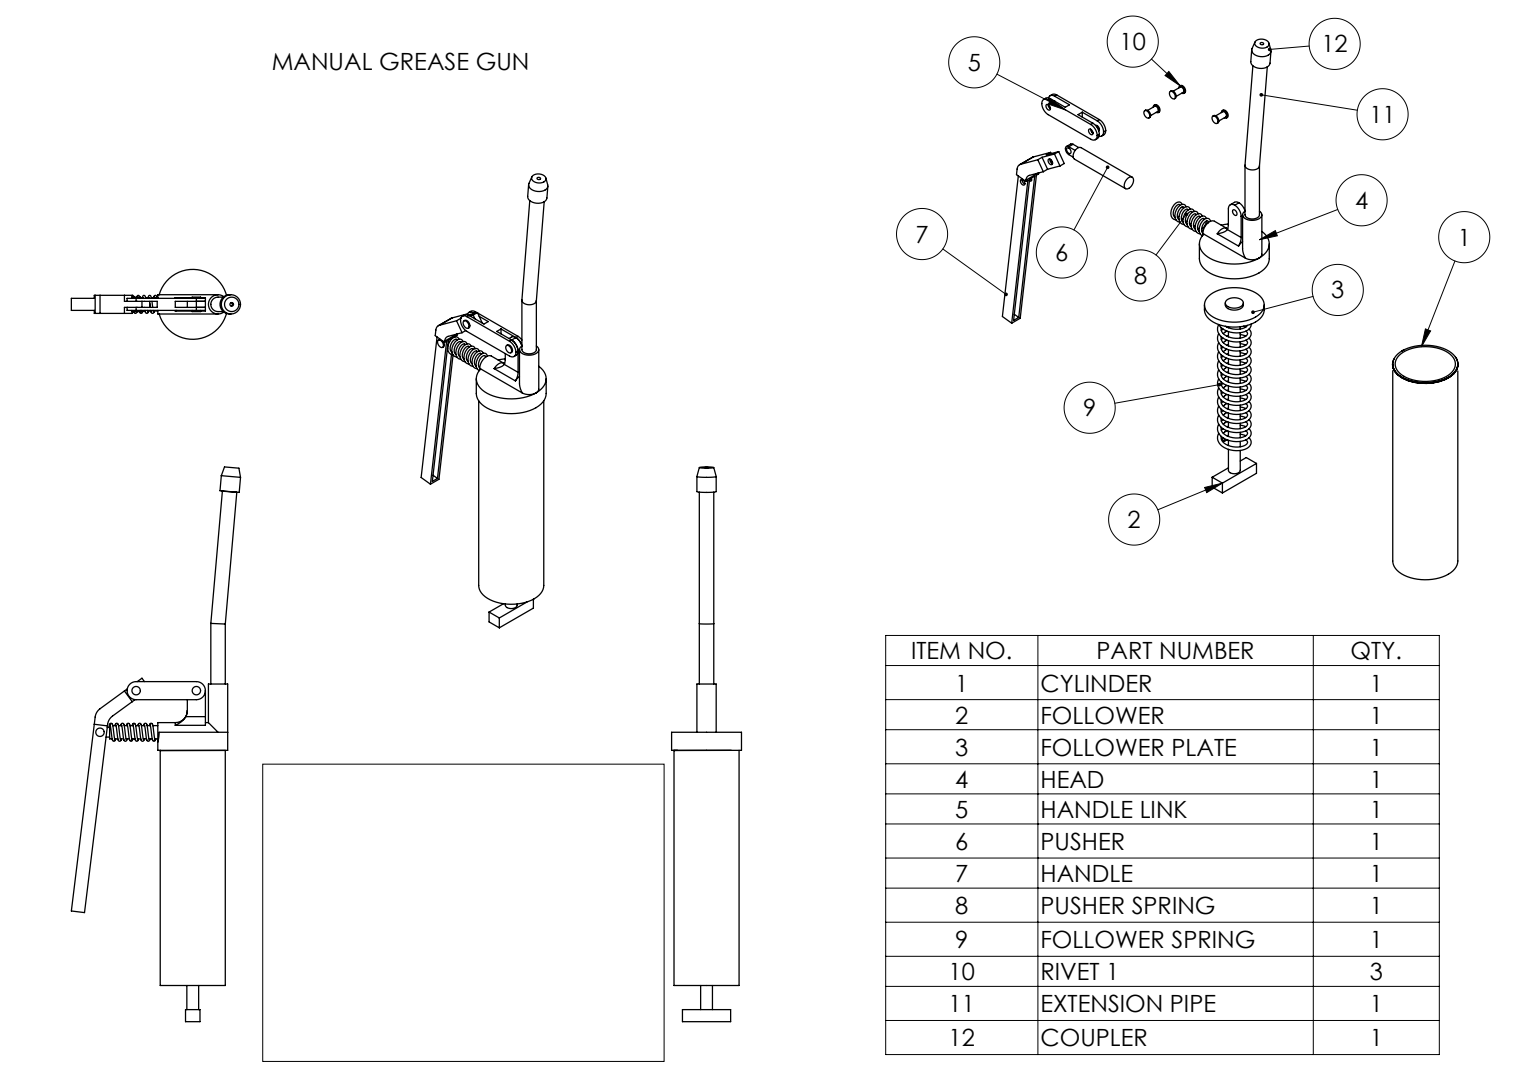
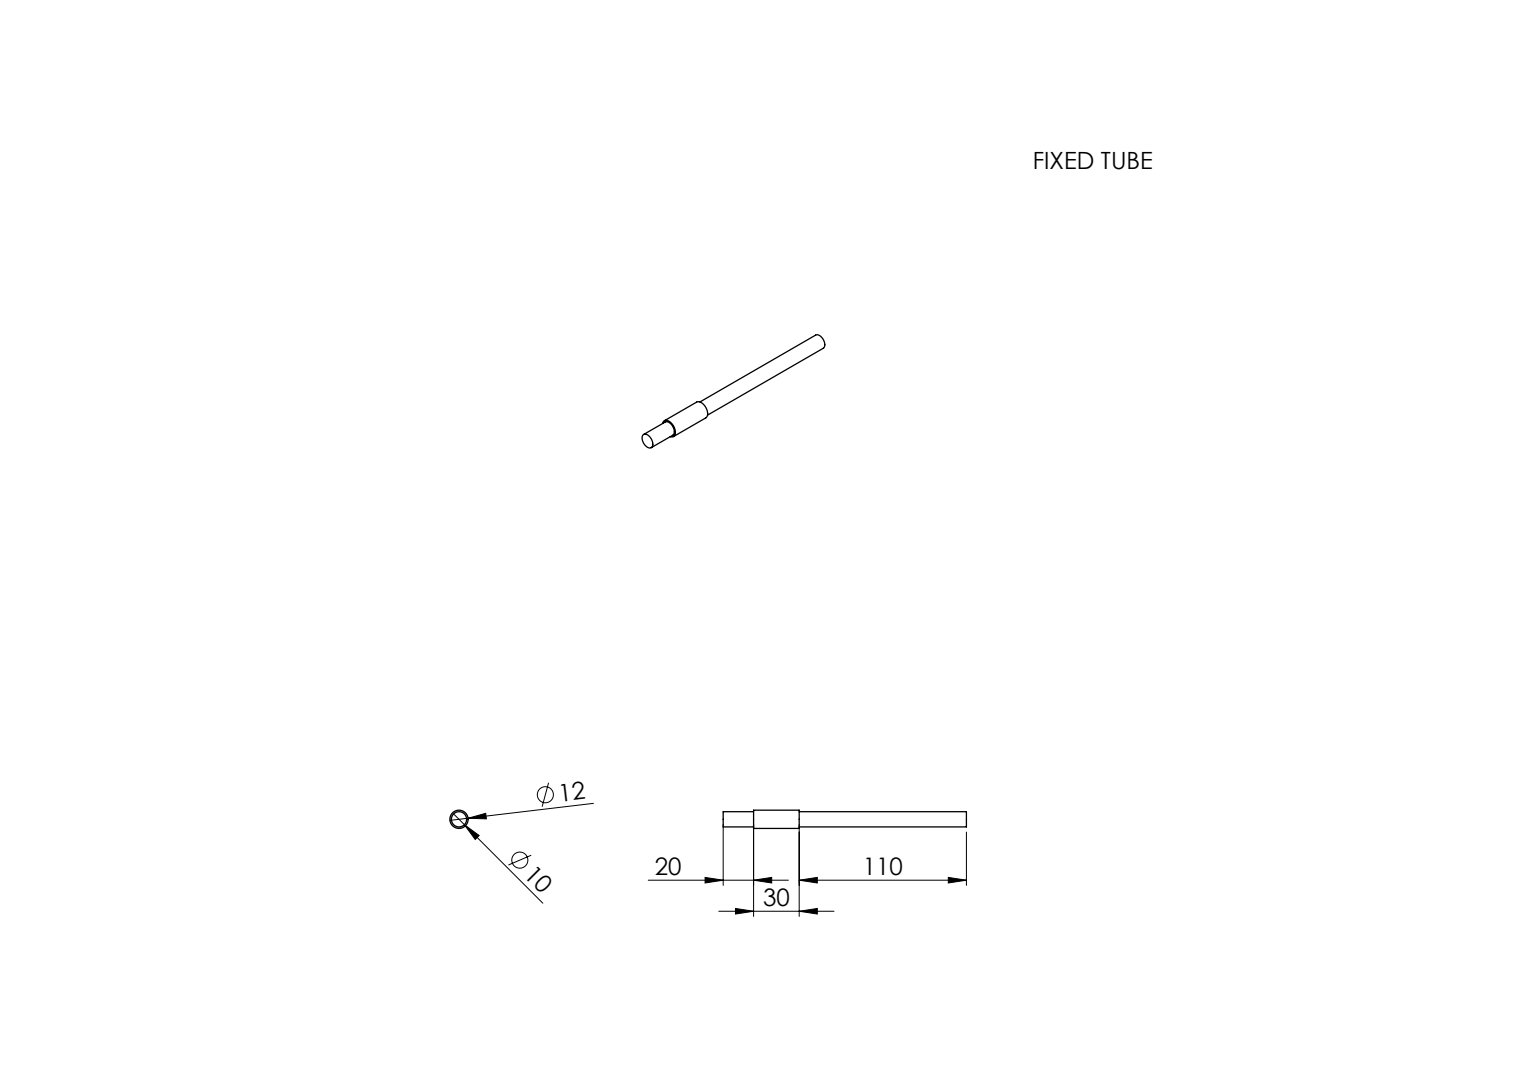
ISO-10303-21;
HEADER;
FILE_DESCRIPTION (('STEP AP214'),
    '1' );
FILE_NAME ('MAS-158',
    '2026-10-31T03:36:27',
    ( '' ),
    ( '' ),
    'SwSTEP 2.0',
    'SolidWorks 2026',
    '' );
FILE_SCHEMA (( 'AUTOMOTIVE_DESIGN' ));
ENDSEC;

DATA;
#1 = CARTESIAN_POINT ( 'NONE',  ( 20.99999999999999645, 6.928203230275506996, -4.556249998770971033 ) ) ;
#3 = ORIENTED_EDGE ( 'NONE', *, *, #2176, .T. ) ;
#2 = CIRCLE ( 'NONE', #23019, 1.000000000000002220 ) ;
#4 = CARTESIAN_POINT ( 'NONE',  ( 28.29077060037018043, 5.407089921784856479, 169.1523531505532674 ) ) ;
#5 = CARTESIAN_POINT ( 'NONE',  ( 6.840914352312096547, 71.36018628210143788, -6.594114490232313663 ) ) ;
#6 = CARTESIAN_POINT ( 'NONE',  ( -3.253724281355068545E-15, 198.6500000012290172, -27.00000000000000355 ) ) ;
#7 = CARTESIAN_POINT ( 'NONE',  ( 10.56230152254411081, 0.000000000000000000, -0.3374999987710014526 ) ) ;
#8 = DIRECTION ( 'NONE',  ( -1.000000000000000000, 0.000000000000000000, 0.000000000000000000 ) ) ;
#9 = CARTESIAN_POINT ( 'NONE',  ( -13.62178482187498396, 196.7843750006145456, 23.59362340125808188 ) ) ;
#10 = DIRECTION ( 'NONE',  ( 0.000000000000000000, 0.000000000000000000, 1.000000000000000000 ) ) ;
#11 = CARTESIAN_POINT ( 'NONE',  ( 31.25278368747686741, 6.928203230275514990, 167.1898537967678351 ) ) ;
#12 = CARTESIAN_POINT ( 'NONE',  ( 1.715153634034445762, 36.67731371789854933, -9.534712964251895073 ) ) ;
#13 = CARTESIAN_POINT ( 'NONE',  ( -1.926257025242585782E-15, 198.3968750006145285, -31.45816453501076637 ) ) ;
#14 = ORIENTED_EDGE ( 'NONE', *, *, #10865, .F. ) ;
#15 = ORIENTED_EDGE ( 'NONE', *, *, #13669, .F. ) ;
#16 = CARTESIAN_POINT ( 'NONE',  ( 18.00000000000000000, 239.6312500012290343, -5.196152422706630247 ) ) ;
#17 = CARTESIAN_POINT ( 'NONE',  ( 6.932735513424201024, 37.25231371789855217, -10.69584247140429412 ) ) ;
#18 = CARTESIAN_POINT ( 'NONE',  ( 19.68408634441911786, -5.407089921784861808, -9.046874999385529748 ) ) ;
#19 = CARTESIAN_POINT ( 'NONE',  ( 15.24356964375000167, -3.323476615752272600, -8.765624999385490668 ) ) ;
#20 = CARTESIAN_POINT ( 'NONE',  ( 13.23911966647199812, 140.7523137178985166, 8.632099005475788900 ) ) ;
#21 = VERTEX_POINT ( 'NONE', #9252 ) ;
#22 = CARTESIAN_POINT ( 'NONE',  ( 13.44051670066911619, -5.407089921784865361, -3.721874999385532679 ) ) ;
#23 = CARTESIAN_POINT ( 'NONE',  ( -13.62178482187500528, 199.2781250006145228, -23.59362340125807123 ) ) ;
#24 = CARTESIAN_POINT ( 'NONE',  ( 24.95044711734591658, -3.604726614523244610, 166.7907448923220954 ) ) ;
#25 = COLOUR_RGB ( '',0.8941176470588234615, 0.8941176470588234615, 0.8941176470588234615 ) ;
#26 = CARTESIAN_POINT ( 'NONE',  ( -33.37127896937850124, 216.5309553116391612, 1.626142955000506873 ) ) ;
#27 = CARTESIAN_POINT ( 'NONE',  ( 26.75643035624999655, 248.1718750006145342, -7.049594010296217766E-16 ) ) ;
#28 =( LENGTH_UNIT ( ) NAMED_UNIT ( * ) SI_UNIT ( .MILLI., .METRE. ) );
#29 = CARTESIAN_POINT ( 'NONE',  ( -17.60279642935561029, 194.9999999999999716, 20.73731651351060989 ) ) ;
#30 = CARTESIAN_POINT ( 'NONE',  ( -63.25669563604515844, 209.8844732041982297, -4.499999999999996447 ) ) ;
#31 = CARTESIAN_POINT ( 'NONE',  ( -50.99330436395489841, 210.1155267958017134, -6.500000000000000888 ) ) ;
#32 = CARTESIAN_POINT ( 'NONE',  ( 37.56819361912707222, 7.646167579472015790E-16, 167.7383919071516516 ) ) ;
#33 = EDGE_LOOP ( 'NONE', ( #36990, #5292, #11130, #31770 ) ) ;
#34 = CARTESIAN_POINT ( 'NONE',  ( 16.56230152254410726, 0.000000000000000000, -10.00000000000000000 ) ) ;
#35 = CARTESIAN_POINT ( 'NONE',  ( 23.99999999999999645, 5.196152422706631135, -0.5437499987709648597 ) ) ;
#36 = CARTESIAN_POINT ( 'NONE',  ( -13.23911966647199812, 25.75231371789854506, -8.632099005475788900 ) ) ;
#37 = CARTESIAN_POINT ( 'NONE',  ( -60.49330436395489130, 210.1155267958016850, -8.500000000000003553 ) ) ;
#38 = CARTESIAN_POINT ( 'NONE',  ( -9.500000000000005329, 141.5101862821014720, -0.1745138560725176813 ) ) ;
#39 = CARTESIAN_POINT ( 'NONE',  ( 2.311890736173175753, 56.12268628210144072, 12.53471296425194836 ) ) ;
#40 = CARTESIAN_POINT ( 'NONE',  ( 13.56230152254411792, -5.196152422706638241, -4.875000000000101252 ) ) ;
#41 = ORIENTED_EDGE ( 'NONE', *, *, #17124, .T. ) ;
#42 = CARTESIAN_POINT ( 'NONE',  ( -39.90997103062156270, 215.5714017266979852, 3.350049139982118618 ) ) ;
#43 = LINE ( 'NONE', #12559, #36906 ) ;
#44 = CARTESIAN_POINT ( 'NONE',  ( 13.62178482187501416, 195.9593750006145569, 23.59362340125806767 ) ) ;
#45 = CARTESIAN_POINT ( 'NONE',  ( 31.45868912971818432, 0.000000000000000000, 169.5433637710095809 ) ) ;
#46 = CARTESIAN_POINT ( 'NONE',  ( 37.19073179189800271, 7.347880794884117764E-16, 166.2186317273649934 ) ) ;
#47 = CARTESIAN_POINT ( 'NONE',  ( 22.60769515458672529, 246.3236538117967029, -6.000000000000004441 ) ) ;
#48 = CARTESIAN_POINT ( 'NONE',  ( 26.75643035624999655, 244.7218750006145456, -3.323476615752271712 ) ) ;
#49 = CARTESIAN_POINT ( 'NONE',  ( 8.843639120294245259, 94.46481371789855075, 3.474262827703527901 ) ) ;
#50 = LINE ( 'NONE', #15224, #14231 ) ;
#51 = VECTOR ( 'NONE', #30355, 1000.000000000000000 ) ;
#52 = ORIENTED_EDGE ( 'NONE', *, *, #4531, .T. ) ;
#53 = CARTESIAN_POINT ( 'NONE',  ( -55.74330436395489841, 210.1155267958017134, -6.500000000000000888 ) ) ;
#54 = CARTESIAN_POINT ( 'NONE',  ( 23.99999999999999645, 245.8562500012290570, -5.196152422706631135 ) ) ;
#55 = VERTEX_POINT ( 'NONE', #18167 ) ;
#56 = CARTESIAN_POINT ( 'NONE',  ( -10.49813415416004858, 106.8273137178985479, 7.228626920338840023 ) ) ;
#57 = CARTESIAN_POINT ( 'NONE',  ( 13.44051670066911441, -5.407089921784865361, -1.021874999385524729 ) ) ;
#58 = CARTESIAN_POINT ( 'NONE',  ( 24.36378002397578868, 0.000000000000000000, 160.0851093307920223 ) ) ;
#59 = CARTESIAN_POINT ( 'NONE',  ( 26.75643035624999655, 3.323476615752271712, -1.340624999385481075 ) ) ;
#60 = CARTESIAN_POINT ( 'NONE',  ( 0.1745138560722779009, 68.58981371789856496, 12.50000000000000355 ) ) ;
#61 = CARTESIAN_POINT ( 'NONE',  ( 27.00000000000001066, 196.1375000000000171, 15.58845726811988897 ) ) ;
#62 = EDGE_CURVE ( 'NONE', #31856, #6278, #12468, .T. ) ;
#63 = ORIENTED_EDGE ( 'NONE', *, *, #14775, .T. ) ;
#64 = ORIENTED_EDGE ( 'NONE', *, *, #31239, .F. ) ;
#65 = ORIENTED_EDGE ( 'NONE', *, *, #28486, .T. ) ;
#66 = CARTESIAN_POINT ( 'NONE',  ( 18.00000000000000355, -5.196152422706632912, -7.518749998770946519 ) ) ;
#67 = CARTESIAN_POINT ( 'NONE',  ( 23.87821517812499650, 4.985214923628404904, -6.140624999385474680 ) ) ;
#68 = CARTESIAN_POINT ( 'NONE',  ( 10.56230152254517307, 3.464101615138364565, -6.224999998771024501 ) ) ;
#69 = CARTESIAN_POINT ( 'NONE',  ( 23.87821517812499650, 246.8968750006145285, -4.985214923628404904 ) ) ;
#70 = CARTESIAN_POINT ( 'NONE',  ( 12.53471296425194836, 44.62268628210144783, -2.311890736173178418 ) ) ;
#71 =( BOUNDED_CURVE ( )  B_SPLINE_CURVE ( 2, ( #25117, #31002, #36483, #31184, #33841, #22103, #11088, #7506, #25303, #25677, #37040, #22287, #37228, #16414, #5388, #22845, #19080, #4648, #7879, #11276, #5022, #24930, #13939, #16602, #28145, #33652, #16967, #25488, #30632, #10526, #31363, #36855, #10899, #7691, #16229, #4836, #13565, #22472, #28510, #14121, #27961, #34021, #8065, #19272, #19642, #36675, #30813, #10713, #22664, #5207, #2366, #16783, #28328, #1992, #34208, #8252, #19826, #3481, #14864, #31546, #34574, #20184, #28698, #32288, #14673, #14488, #2918, #17156, #23026, #25859, #2734, #8803, #31734, #28883, #12011, #11824, #37407, #31918, #8433, #630, #20376, #11637, #14307, #26045, #5947, #34761, #259, #29446, #34943, #8614, #26223, #17711, #6330, #5761, #23395, #72, #23211, #17527, #29061, #17341, #11458, #3105, #8987, #5571, #20744, #20558, #32102, #6133, #29251, #3292, #26411, #445, #23583, #35126, #9176, #17901, #15050, #26599, #12197, #34392, #20002, #7093, #10110, #21503, #12580, #29821, #21681, #33046, #32473, #15615, #24517, #12767, #24336, #33233, #18662, #30202, #27169, #26790, #4043, #21125, #18472, #15240, #20939, #21313, #35877, #26980, #35310, #4415, #12391, #4228, #1192, #9919, #1386, #15997, #12957, #1007, #27545, #6897, #30013, #18847, #24147, #35689, #36067, #15805, #32850, #27355, #9742, #7272, #30392, #1571, #23771, #9365, #6518, #18093, #29634, #3670, #821, #23961, #35504, #9551, #32664, #6705, #18277, #3855, #15431, #16364, #22423, #24885, #34157, #21865, #2129, #13326, #5344 ),
 .UNSPECIFIED., .F., .F. ) 
 B_SPLINE_CURVE_WITH_KNOTS ( ( 3, 2, 2, 2, 2, 2, 2, 2, 2, 2, 2, 2, 2, 2, 2, 2, 2, 2, 2, 2, 2, 2, 2, 2, 2, 2, 2, 2, 2, 2, 2, 2, 2, 2, 2, 2, 2, 2, 2, 2, 2, 2, 2, 2, 2, 2, 2, 2, 2, 2, 2, 2, 2, 2, 2, 2, 2, 2, 2, 2, 2, 2, 2, 2, 2, 2, 2, 2, 2, 2, 2, 2, 2, 2, 2, 2, 2, 2, 2, 2, 2, 2, 2, 2, 2, 2, 2, 2, 2, 2, 2, 2, 2, 2, 2, 2, 3 ),
 ( 0.000000000000000000, 0.01041666666666666609, 0.02083333333333333218, 0.03125000000000000000, 0.04166666666666666435, 0.05208333333333333565, 0.06250000000000000000, 0.07291666666666667129, 0.08333333333333332871, 0.09375000000000000000, 0.1041666666666666713, 0.1145833333333333287, 0.1250000000000000000, 0.1354166666666666574, 0.1458333333333333426, 0.1562500000000000000, 0.1666666666666666574, 0.1770833333333333426, 0.1875000000000000000, 0.1979166666666666574, 0.2083333333333333426, 0.2187500000000000000, 0.2291666666666666574, 0.2395833333333333426, 0.2500000000000000000, 0.2604166666666666852, 0.2708333333333333148, 0.2812500000000000000, 0.2916666666666666852, 0.3020833333333333148, 0.3125000000000000000, 0.3229166666666666852, 0.3333333333333333148, 0.3437500000000000000, 0.3541666666666666852, 0.3645833333333333148, 0.3750000000000000000, 0.3854166666666666852, 0.3958333333333333148, 0.4062500000000000000, 0.4166666666666666852, 0.4270833333333333148, 0.4375000000000000000, 0.4479166666666666852, 0.4583333333333333148, 0.4687500000000000000, 0.4791666666666666852, 0.4895833333333333148, 0.5000000000000000000, 0.5104166666666666297, 0.5208333333333333703, 0.5312500000000000000, 0.5416666666666666297, 0.5520833333333333703, 0.5625000000000000000, 0.5729166666666666297, 0.5833333333333333703, 0.5937500000000000000, 0.6041666666666666297, 0.6145833333333333703, 0.6250000000000000000, 0.6354166666666666297, 0.6458333333333333703, 0.6562500000000000000, 0.6666666666666666297, 0.6770833333333333703, 0.6875000000000000000, 0.6979166666666666297, 0.7083333333333333703, 0.7187500000000000000, 0.7291666666666666297, 0.7395833333333333703, 0.7500000000000000000, 0.7604166666666666297, 0.7708333333333333703, 0.7812500000000000000, 0.7916666666666666297, 0.8020833333333333703, 0.8125000000000000000, 0.8229166666666666297, 0.8333333333333333703, 0.8437500000000000000, 0.8541666666666666297, 0.8645833333333333703, 0.8750000000000000000, 0.8854166666666666297, 0.8958333333333333703, 0.9062500000000000000, 0.9166666666666666297, 0.9270833333333333703, 0.9375000000000000000, 0.9479166666666666297, 0.9583333333333333703, 0.9687500000000000000, 0.9791666666666666297, 0.9895833333333333703, 1.000000000000000000 ),
 .UNSPECIFIED. ) 
 CURVE ( )  GEOMETRIC_REPRESENTATION_ITEM ( )  RATIONAL_B_SPLINE_CURVE ( ( 1.000000000000000000, 0.9659258262890683122, 1.000000000000000000, 0.9659258262890683122, 1.000000000000000000, 0.9659258262890683122, 1.000000000000000000, 0.9659258262890683122, 1.000000000000000000, 0.9659258262890683122, 1.000000000000000000, 0.9659258262890683122, 1.000000000000000000, 0.9659258262890683122, 1.000000000000000000, 0.9659258262890683122, 1.000000000000000000, 0.9659258262890683122, 1.000000000000000000, 0.9659258262890683122, 1.000000000000000000, 0.9659258262890683122, 1.000000000000000000, 0.9659258262890683122, 1.000000000000000000, 0.9659258262890683122, 1.000000000000000000, 0.9659258262890683122, 1.000000000000000000, 0.9659258262890683122, 1.000000000000000000, 0.9659258262890683122, 1.000000000000000000, 0.9659258262890683122, 1.000000000000000000, 0.9659258262890683122, 1.000000000000000000, 0.9659258262890683122, 1.000000000000000000, 0.9659258262890683122, 1.000000000000000000, 0.9659258262890683122, 1.000000000000000000, 0.9659258262890683122, 1.000000000000000000, 0.9659258262890683122, 1.000000000000000000, 0.9659258262890683122, 1.000000000000000000, 0.9659258262890683122, 1.000000000000000000, 0.9659258262890683122, 1.000000000000000000, 0.9659258262890683122, 1.000000000000000000, 0.9659258262890683122, 1.000000000000000000, 0.9659258262890683122, 1.000000000000000000, 0.9659258262890683122, 1.000000000000000000, 0.9659258262890683122, 1.000000000000000000, 0.9659258262890683122, 1.000000000000000000, 0.9659258262890683122, 1.000000000000000000, 0.9659258262890683122, 1.000000000000000000, 0.9659258262890683122, 1.000000000000000000, 0.9659258262890683122, 1.000000000000000000, 0.9659258262890683122, 1.000000000000000000, 0.9659258262890683122, 1.000000000000000000, 0.9659258262890683122, 1.000000000000000000, 0.9659258262890683122, 1.000000000000000000, 0.9659258262890683122, 1.000000000000000000, 0.9659258262890683122, 1.000000000000000000, 0.9659258262890683122, 1.000000000000000000, 0.9659258262890683122, 1.000000000000000000, 0.9659258262890683122, 1.000000000000000000, 0.9659258262890683122, 1.000000000000000000, 0.9659258262890683122, 1.000000000000000000, 0.9659258262890683122, 1.000000000000000000, 0.9659258262890683122, 1.000000000000000000, 0.9659258262890683122, 1.000000000000000000, 0.9659258262890683122, 1.000000000000000000, 0.9659258262890683122, 1.000000000000000000, 0.9659258262890683122, 1.000000000000000000, 0.9659258262890683122, 1.000000000000000000, 0.9659258262890683122, 1.000000000000000000, 0.9659258262890683122, 1.000000000000000000, 0.9659258262890683122, 1.000000000000000000, 0.9659258262890683122, 1.000000000000000000, 0.9659258262890683122, 1.000000000000000000, 0.9659258262890683122, 1.000000000000000000, 0.9659258262890683122, 1.000000000000000000, 0.9659258262890683122, 1.000000000000000000, 0.9659258262890683122, 1.000000000000000000, 0.9659258262890683122, 1.000000000000000000, 0.9659258262890683122, 1.000000000000000000, 0.9659258262890683122, 1.000000000000000000, 0.9659258262890683122, 1.000000000000000000, 0.9659258262890683122, 1.000000000000000000, 0.9659258262890683122, 1.000000000000000000, 0.9659258262890683122, 1.000000000000000000, 0.9659258262890683122, 1.000000000000000000, 0.9659258262890683122, 1.000000000000000000, 0.9659258262890683122, 1.000000000000000000, 0.9659258262890683122, 1.000000000000000000, 0.9659258262890683122, 1.000000000000000000, 0.9659258262890683122, 1.000000000000000000, 0.9659258262890683122, 1.000000000000000000, 0.9659258262890683122, 1.000000000000000000, 0.9659258262890683122, 1.000000000000000000, 0.9659258262890683122, 1.000000000000000000, 0.9659258262890683122, 1.000000000000000000, 0.9659258262890683122, 1.000000000000000000, 0.9659258262890683122, 1.000000000000000000, 0.9659258262890683122, 1.000000000000000000, 0.9659258262890683122, 1.000000000000000000, 0.9659258262890683122, 1.000000000000000000, 0.9659258262890683122, 1.000000000000000000, 0.9659258262890683122, 1.000000000000000000, 0.9659258262890683122, 1.000000000000000000, 0.9659258262890683122, 1.000000000000000000, 0.9659258262890683122, 1.000000000000000000, 0.9659258262890683122, 1.000000000000000000, 0.9659258262890683122, 1.000000000000000000, 0.9659258262890683122, 1.000000000000000000, 0.9659258262890683122, 1.000000000000000000, 0.9659258262890683122, 1.000000000000000000 ) ) 
 REPRESENTATION_ITEM ( '' )  );
#72 = CARTESIAN_POINT ( 'NONE',  ( -49.20461230271183695, 208.1428034533958851, -6.469044688360754414 ) ) ;
#73 = CARTESIAN_POINT ( 'NONE',  ( 19.06670604969950489, 215.1554505341192964, -5.693556627486040966 ) ) ;
#74 = CARTESIAN_POINT ( 'NONE',  ( -39.30877896937850124, 211.0902445701383101, -4.530955311639234040 ) ) ;
#75 = CARTESIAN_POINT ( 'NONE',  ( 33.73804336749152810, 5.196152422706631135, 161.1753621882693892 ) ) ;
#76 = CARTESIAN_POINT ( 'NONE',  ( 0.1745138560722779009, 96.18981371789855928, 12.50000000000000355 ) ) ;
#77 = CARTESIAN_POINT ( 'NONE',  ( -61.28497103062156981, 206.1606490808709111, -2.350049139982163027 ) ) ;
#78 = CARTESIAN_POINT ( 'NONE',  ( -39.90997103062156270, 217.3034525342668815, 4.350049139982096413 ) ) ;
#79 = EDGE_CURVE ( 'NONE', #19909, #6556, #23186, .T. ) ;
#80 = CARTESIAN_POINT ( 'NONE',  ( 23.87821517812499650, 4.985214923628404904, -5.353124999385477700 ) ) ;
#81 = CARTESIAN_POINT ( 'NONE',  ( 10.56230152254410726, 0.000000000000000000, -4.387499998770999277 ) ) ;
#82 = CARTESIAN_POINT ( 'NONE',  ( -3.257655550456946880, 82.10231371789853938, -15.46528703574811736 ) ) ;
#83 = CARTESIAN_POINT ( 'NONE',  ( -60.88169563604516554, 210.1155267958018271, 8.500000000000003553 ) ) ;
#84 = ORIENTED_EDGE ( 'NONE', *, *, #36303, .T. ) ;
#85 = DIRECTION ( 'NONE',  ( -0.000000000000000000, -0.000000000000000000, 1.000000000000000000 ) ) ;
#86 = CARTESIAN_POINT ( 'NONE',  ( -8.715434833791929847, 105.8601862821014521, -8.962234695871762469 ) ) ;
#87 = CARTESIAN_POINT ( 'NONE',  ( 13.04141134922759804, 54.97268628210144215, 8.927990412390657937 ) ) ;
#88 = EDGE_CURVE ( 'NONE', #32501, #27950, #21194, .T. ) ;
#89 = DIRECTION ( 'NONE',  ( -1.000000000000000000, -6.123233995736766036E-17, 0.000000000000000000 ) ) ;
#90 =( BOUNDED_CURVE ( )  B_SPLINE_CURVE ( 2, ( #11851, #8830, #29090, #22871, #2761, #17369, #11485, #23054, #34600 ),
 .UNSPECIFIED., .F., .F. ) 
 B_SPLINE_CURVE_WITH_KNOTS ( ( 3, 2, 2, 2, 3 ),
 ( 0.3125000000000000000, 0.3194444444444444198, 0.3333333333333333148, 0.3472222222222222099, 0.3541666666666666852 ),
 .UNSPECIFIED. ) 
 CURVE ( )  GEOMETRIC_REPRESENTATION_ITEM ( )  RATIONAL_B_SPLINE_CURVE ( ( 0.9330127018922194093, 0.9330127018922194093, 1.000000000000000000, 0.8660254037844387076, 1.000000000000000000, 0.8660254037844387076, 1.000000000000000000, 0.9330127018922190762, 0.9330127018922194093 ) ) 
 REPRESENTATION_ITEM ( '' )  );
#91 = CARTESIAN_POINT ( 'NONE',  ( 36.93903810116746911, 3.604726614523243278, 160.5471114303018680 ) ) ;
#92 = CARTESIAN_POINT ( 'NONE',  ( -0.1745138560725817967, 74.81018628210145494, 15.50000000000000533 ) ) ;
#93 = CARTESIAN_POINT ( 'NONE',  ( 27.24356964375000700, 199.0906250006145228, 15.72908226750537075 ) ) ;
#94 = CARTESIAN_POINT ( 'NONE',  ( 10.31873187879411269, 0.000000000000000000, -10.04062499938554431 ) ) ;
#95 = DIRECTION ( 'NONE',  ( 0.000000000000000000, 0.000000000000000000, 1.000000000000000000 ) ) ;
#96 = CARTESIAN_POINT ( 'NONE',  ( -46.63913769728824121, 206.8500491399821044, -5.686928522499717253 ) ) ;
#97 = CARTESIAN_POINT ( 'NONE',  ( 11.28998163430637725, -3.344369132205555317, -9.999999999999998224 ) ) ;
#98 = CARTESIAN_POINT ( 'NONE',  ( 11.48171059495397728, 45.48518628210145209, 4.944772684328674117 ) ) ;
#99 = CARTESIAN_POINT ( 'NONE',  ( 5.727106289114498080E-15, 196.0625000000000000, 31.17691453623979214 ) ) ;
#100 = DIRECTION ( 'NONE',  ( -1.000000000000000000, 0.000000000000000000, 5.782411586589356653E-16 ) ) ;
#101 = CARTESIAN_POINT ( 'NONE',  ( 9.534712964251900402, 140.1773137178985564, 1.715153634034445540 ) ) ;
#102 = CARTESIAN_POINT ( 'NONE',  ( 26.75643035624999655, 247.8718750006145228, -3.323476615752271268 ) ) ;
#103 = ORIENTED_EDGE ( 'NONE', *, *, #10401, .F. ) ;
#104 = CARTESIAN_POINT ( 'NONE',  ( 15.00000000000000000, 3.464101615137752166, -5.437500000000009770 ) ) ;
#105 = AXIS2_PLACEMENT_3D ( 'NONE', #31796, #37295, #28576 ) ;
#106 = DIRECTION ( 'NONE',  ( 0.9961946980917462113, 0.000000000000000000, -0.08715574274765118534 ) ) ;
#107 = LINE ( 'NONE', #3514, #14620 ) ;
#108 = CARTESIAN_POINT ( 'NONE',  ( 22.80587116629411781, -3.604726614523235284, -3.553124999385526728 ) ) ;
#109 = CARTESIAN_POINT ( 'NONE',  ( 31.18169728485186454, -7.209453229046475009, 166.3773324967488918 ) ) ;
#110 = CARTESIAN_POINT ( 'NONE',  ( 26.99999999999999645, 240.2874999999999659, 3.464101615137751278 ) ) ;
#111 = DIRECTION ( 'NONE',  ( 1.000000000000000000, 0.000000000000000000, 0.000000000000000000 ) ) ;
#112 = CARTESIAN_POINT ( 'NONE',  ( -12.53471296425194659, 67.62268628210145494, 2.311890736173176641 ) ) ;
#113 = VERTEX_POINT ( 'NONE', #15124 ) ;
#114 = ORIENTED_EDGE ( 'NONE', *, *, #15759, .T. ) ;
#115 = CARTESIAN_POINT ( 'NONE',  ( -98.52697526167152375, 63.53212182842481326, 3.000000000000000000 ) ) ;
#116 = VECTOR ( 'NONE', #35899, 1000.000000000000000 ) ;
#117 = CARTESIAN_POINT ( 'NONE',  ( 26.99999999999999645, 194.9750000012290343, -15.58845726811990495 ) ) ;
#118 = DIRECTION ( 'NONE',  ( -0.000000000000000000, 0.000000000000000000, 1.000000000000000000 ) ) ;
#119 = CARTESIAN_POINT ( 'NONE',  ( 21.00000000000000000, 6.646953231504538984, -7.003124999385472726 ) ) ;
#120 = ADVANCED_FACE ( 'NONE', ( #26675 ), #705, .F. ) ;
#121 = CARTESIAN_POINT ( 'NONE',  ( 8.632099005475788900, 46.45231371789854791, -13.23911966647199812 ) ) ;
#122 = CARTESIAN_POINT ( 'NONE',  ( 31.03707322417642800, -6.928203230275514990, 164.7242719189907803 ) ) ;
#123 = CARTESIAN_POINT ( 'NONE',  ( 34.15965927292618431, 5.196152422706637353, 165.9944540390638679 ) ) ;
#124 = CARTESIAN_POINT ( 'NONE',  ( -40.10788769728823411, 214.4690446883608104, 1.321298161741840893 ) ) ;
#125 = CARTESIAN_POINT ( 'NONE',  ( 16.56230152254410726, 0.000000000000000000, -10.00000000000000000 ) ) ;
#126 = CARTESIAN_POINT ( 'NONE',  ( 31.34102887711597774, 6.928203230275506996, 168.1985009298100522 ) ) ;
#127 = CARTESIAN_POINT ( 'NONE',  ( -3.474262827703527901, 23.16481371789855359, 8.843639120294245259 ) ) ;
#128 = EDGE_CURVE ( 'NONE', #11418, #35635, #36670, .T. ) ;
#129 = CARTESIAN_POINT ( 'NONE',  ( -55.74330436395489841, 210.1155267958017134, -6.500000000000000888 ) ) ;
#130 = DIRECTION ( 'NONE',  ( 1.000000000000000000, 0.000000000000000000, 0.000000000000000000 ) ) ;
#131 = DIRECTION ( 'NONE',  ( 0.9961946980917462113, 0.000000000000000000, -0.08715574274765118534 ) ) ;
#132 = CARTESIAN_POINT ( 'NONE',  ( -1.926257025242585782E-15, 195.6968750006145683, -31.45816453501075927 ) ) ;
#133 = CARTESIAN_POINT ( 'NONE',  ( -3.257655550456946880, 137.3023137178985564, -15.46528703574811736 ) ) ;
#134 =( BOUNDED_CURVE ( )  B_SPLINE_CURVE ( 2, ( #28363, #34243, #8285, #7031, #33171, #27292, #31580 ),
 .UNSPECIFIED., .F., .F. ) 
 B_SPLINE_CURVE_WITH_KNOTS ( ( 3, 2, 2, 3 ),
 ( 0.2826086956521732252, 0.2898550724637675158, 0.2971014492753617509, 0.3043478260869560414 ),
 .UNSPECIFIED. ) 
 CURVE ( )  GEOMETRIC_REPRESENTATION_ITEM ( )  RATIONAL_B_SPLINE_CURVE ( ( 1.000000000000012212, 0.8660254037844263841, 1.000000000000000000, 0.8660254037844387076, 1.000000000000000000, 0.8660254037844479225, 0.9999999999999907851 ) ) 
 REPRESENTATION_ITEM ( '' )  );
#135 = ADVANCED_FACE ( 'NONE', ( #36144 ), #26701, .T. ) ;
#136 = EDGE_LOOP ( 'NONE', ( #21590, #33549, #31769, #19071 ) ) ;
#137 = CARTESIAN_POINT ( 'NONE',  ( -4.622313124798576922, 42.03518628210144215, -11.61527771782819762 ) ) ;
#138 = PLANE ( 'NONE',  #16547 ) ;
#139 = CARTESIAN_POINT ( 'NONE',  ( 26.40304527788004663, 2.021082040740327379, -8.000000000000000000 ) ) ;
#140 = CARTESIAN_POINT ( 'NONE',  ( 37.59924285248093412, -3.604726614523238837, 168.0932862683468443 ) ) ;
#141 = CARTESIAN_POINT ( 'NONE',  ( 15.00000000000000178, -3.464101615137757051, -1.256249998770949228 ) ) ;
#142 = CARTESIAN_POINT ( 'NONE',  ( 13.44051670066910908, 5.407089921784862696, -9.721874999385510918 ) ) ;
#143 = CARTESIAN_POINT ( 'NONE',  ( 8.710071997420127943, 82.28518628210146346, 3.796722387233375073 ) ) ;
#144 = CYLINDRICAL_SURFACE ( 'NONE', #32201, 27.00000000000000000 ) ;
#145 = CARTESIAN_POINT ( 'NONE',  ( 22.60769515458672885, 244.9174038105676630, -5.999999999999998224 ) ) ;
#146 = ADVANCED_FACE ( 'NONE', ( #11518 ), #17218, .F. ) ;
#147 = CARTESIAN_POINT ( 'NONE',  ( -12.53471296425194836, 86.02268628210146062, 2.311890736173176641 ) ) ;
#148 = CARTESIAN_POINT ( 'NONE',  ( -13.50000000000000533, 195.0875000012290457, -23.38268590217984411 ) ) ;
#149 = VERTEX_POINT ( 'NONE', #2983 ) ;
#150 = CARTESIAN_POINT ( 'NONE',  ( 36.93740393099094632, -3.604726614523235284, 160.5284327797126025 ) ) ;
#151 = CARTESIAN_POINT ( 'NONE',  ( 15.24356964374999990, 3.323476615752268604, -7.378124999385474503 ) ) ;
#152 = LINE ( 'NONE', #25749, #18668 ) ;
#153 = CARTESIAN_POINT ( 'NONE',  ( 24.98313052087628350, 3.604726614523240613, 167.1643179041065252 ) ) ;
#154 = CARTESIAN_POINT ( 'NONE',  ( 34.06814574304114984, -5.196152422706635576, 164.9484496060674985 ) ) ;
#155 = LINE ( 'NONE', #26123, #10199 ) ;
#156 = CARTESIAN_POINT ( 'NONE',  ( 18.00000000000000355, 248.7249999999999943, 5.196152422706632912 ) ) ;
#157 = CARTESIAN_POINT ( 'NONE',  ( 27.24356964374999279, 197.8156250006145171, -15.72908226750539207 ) ) ;
#158 = CARTESIAN_POINT ( 'NONE',  ( 0.1745138560722779009, 123.7898137178985678, 12.50000000000000355 ) ) ;
#159 = CARTESIAN_POINT ( 'NONE',  ( -4.944772684328673229, 121.3851862821014578, 11.48171059495397728 ) ) ;
#160 = UNCERTAINTY_MEASURE_WITH_UNIT (LENGTH_MEASURE( 1.000000000000000082E-05 ), #19760, 'distance_accuracy_value', 'NONE');
#162 = ORIENTED_EDGE ( 'NONE', *, *, #30521, .T. ) ;
#161 = EDGE_LOOP ( 'NONE', ( #20979, #30282, #30052, #34984, #7724, #7445, #15889, #35352 ) ) ;
#163 = CARTESIAN_POINT ( 'NONE',  ( -13.62178482187498396, 198.5281250006145228, 23.59362340125808188 ) ) ;
#164 = CARTESIAN_POINT ( 'NONE',  ( 23.87821517812500005, 243.1468750006145285, 4.985214923628404016 ) ) ;
#165 = ADVANCED_FACE ( 'NONE', ( #28756 ), #138, .T. ) ;
#166 = CARTESIAN_POINT ( 'NONE',  ( -13.23911966647199812, 90.15231371789855075, -8.632099005475788900 ) ) ;
#167 = AXIS2_PLACEMENT_3D ( 'NONE', #4303, #33308, #24772 ) ;
#168 = CARTESIAN_POINT ( 'NONE',  ( 26.75643035624999655, 3.323476615752271712, -3.140624999385464022 ) ) ;
#169 = CARTESIAN_POINT ( 'NONE',  ( 23.87821517812499650, 246.5593750006145228, -4.985214923628404904 ) ) ;
#170 = CARTESIAN_POINT ( 'NONE',  ( 5.727106289114498080E-15, 197.0750000012290570, 31.17691453623979214 ) ) ;
#171 = CARTESIAN_POINT ( 'NONE',  ( 9.465287035748106703, 84.40231371789855075, -2.064181346179063237 ) ) ;
#172 = CARTESIAN_POINT ( 'NONE',  ( 19.68408634441911076, 5.407089921784857367, -4.790624999385539873 ) ) ;
#173 = CARTESIAN_POINT ( 'NONE',  ( 26.75643035624999655, 241.9093750006145171, -3.323476615752271268 ) ) ;
#174 = CARTESIAN_POINT ( 'NONE',  ( 10.49813415416005213, 47.02731371789855075, -7.228626920338837358 ) ) ;
#175 = EDGE_CURVE ( 'NONE', #2711, #16688, #11211, .T. ) ;
#176 = CARTESIAN_POINT ( 'NONE',  ( 26.99999999999999645, 246.6812500012290457, -7.347880794884117764E-16 ) ) ;
#177 = AXIS2_PLACEMENT_3D ( 'NONE', #6579, #20812, #23648 ) ;
#178 = CARTESIAN_POINT ( 'NONE',  ( 10.49813415415989581, 110.1726862821014521, 7.228626920339068285 ) ) ;
#179 = CARTESIAN_POINT ( 'NONE',  ( 10.56230152254411259, 3.464101615137752166, -4.874999998771025744 ) ) ;
#180 = CARTESIAN_POINT ( 'NONE',  ( -31.99330436395490196, 210.1155267958017134, -6.500000000000000888 ) ) ;
#181 = CARTESIAN_POINT ( 'NONE',  ( -7.228626920339069173, 140.0726862821014720, 10.49813415415989581 ) ) ;
#182 = CARTESIAN_POINT ( 'NONE',  ( 21.00000000000016342, 4.000000000000002665, 50.00000000000000000 ) ) ;
#183 = CARTESIAN_POINT ( 'NONE',  ( -15.46528703574804986, 104.9976862821014549, -3.257655550457287497 ) ) ;
#184 = CARTESIAN_POINT ( 'NONE',  ( 10.49813415415989581, 18.17268628210144499, 7.228626920339069173 ) ) ;
#185 = CARTESIAN_POINT ( 'NONE',  ( 0.000000000000000000, 2.000000000000000000, 0.000000000000000000 ) ) ;
#186 = CARTESIAN_POINT ( 'NONE',  ( 0.000000000000000000, 148.0000000000000000, 0.000000000000000000 ) ) ;
#187 = CARTESIAN_POINT ( 'NONE',  ( 6.840914352312096547, 126.5601862821014834, -6.594114490232313663 ) ) ;
#188 = CARTESIAN_POINT ( 'NONE',  ( 30.87038786627866216, 6.928203230275506996, 162.8190495601146495 ) ) ;
#189 = CARTESIAN_POINT ( 'NONE',  ( 21.00000000000000000, 241.9843750006145058, -6.646953231504538984 ) ) ;
#190 = VERTEX_POINT ( 'NONE', #2796 ) ;
#191 = FACE_OUTER_BOUND ( 'NONE', #37346, .T. ) ;
#192 = CARTESIAN_POINT ( 'NONE',  ( -8.710071997420127943, 68.48518628210145209, -3.796722387233380402 ) ) ;
#193 = CARTESIAN_POINT ( 'NONE',  ( 15.24356964375000167, -3.323476615752272600, -1.453124999385472016 ) ) ;
#195 = EDGE_CURVE ( 'NONE', #23387, #15078, #25492, .T. ) ;
#194 = CARTESIAN_POINT ( 'NONE',  ( 5.999999999999999112, -30.00000000000000000, -19.99999999999999289 ) ) ;
#196 = DIRECTION ( 'NONE',  ( -0.000000000000000000, -0.000000000000000000, 1.000000000000000000 ) ) ;
#197 = CARTESIAN_POINT ( 'NONE',  ( 5.778771075727756162E-15, 195.0218750006145569, 31.45816453501075927 ) ) ;
#198 = EDGE_CURVE ( 'NONE', #717, #36155, #34079, .T. ) ;
#199 = CARTESIAN_POINT ( 'NONE',  ( 0.000000000000000000, 0.000000000000000000, 0.000000000000000000 ) ) ;
#200 = CARTESIAN_POINT ( 'NONE',  ( -7.234628195640263826, 196.8700961906613713, -27.00000000000003553 ) ) ;
#201 = SHAPE_REPRESENTATION ( 'coupler', ( #17215 ), #24466 ) ;
#202 = CARTESIAN_POINT ( 'NONE',  ( -6.594114490232462877, 42.13981371789854791, 6.840914352311949109 ) ) ;
#203 = DIRECTION ( 'NONE',  ( 0.000000000000000000, 0.000000000000000000, -1.000000000000000000 ) ) ;
#204 = ORIENTED_EDGE ( 'NONE', *, *, #34329, .T. ) ;
#205 = VERTEX_POINT ( 'NONE', #8495 ) ;
#206 = CARTESIAN_POINT ( 'NONE',  ( 26.75643035624999655, 249.4843750006145058, 3.323476615752267715 ) ) ;
#207 = CARTESIAN_POINT ( 'NONE',  ( -8.962234695871565293, 35.23981371789855643, -8.715434833792128799 ) ) ;
#208 = CARTESIAN_POINT ( 'NONE',  ( 16.56230152254411436, 7.209453229046482114, -8.859374999385529748 ) ) ;
#209 = CARTESIAN_POINT ( 'NONE',  ( 19.00081571707366379, 5.492723647597353320, -10.23957781181608517 ) ) ;
#210 = CARTESIAN_POINT ( 'NONE',  ( 8.715434833792128799, 19.13981371789855146, -8.962234695871567070 ) ) ;
#211 = EDGE_CURVE ( 'NONE', #2909, #23659, #28387, .T. ) ;
#212 = VERTEX_POINT ( 'NONE', #19884 ) ;
#213 = CARTESIAN_POINT ( 'NONE',  ( 19.68408634441912142, -5.407089921784861808, -3.646874999385540939 ) ) ;
#214 = CARTESIAN_POINT ( 'NONE',  ( 27.24356964374999635, 199.1656250006145399, -15.72908226750539029 ) ) ;
#215 = CARTESIAN_POINT ( 'NONE',  ( 25.06483902970220967, 0.000000000000000000, 168.0982504335675287 ) ) ;
#216 = CARTESIAN_POINT ( 'NONE',  ( -66.02752896937849414, 214.3500491399821897, 7.303452534266821949 ) ) ;
#217 = CARTESIAN_POINT ( 'NONE',  ( 15.24356964375000167, 248.4343750006145513, 3.323476615752272600 ) ) ;
#218 = FILL_AREA_STYLE ('',( #11593 ) ) ;
#219 = CARTESIAN_POINT ( 'NONE',  ( -17.17757150371551944, 194.9999999999999716, 21.09399746705422984 ) ) ;
#220 = CARTESIAN_POINT ( 'NONE',  ( -53.55877896937850124, 211.0902445701383101, -4.530955311639234040 ) ) ;
#221 = CARTESIAN_POINT ( 'NONE',  ( -38.52455436395488420, 205.1570982666397356, 4.673758765035198159 ) ) ;
#222 = EDGE_LOOP ( 'NONE', ( #9327, #12339, #21719, #21080 ) ) ;
#223 = CARTESIAN_POINT ( 'NONE',  ( -28.99999999999999645, 201.9999999999999716, -1.007612034238798379E-23 ) ) ;
#224 = CARTESIAN_POINT ( 'NONE',  ( 20.99999999999997868, 210.0000000000000000, -5.999999999999999112 ) ) ;
#225 = CARTESIAN_POINT ( 'NONE',  ( -13.23911966647199812, 16.55231371789855643, -8.632099005475788900 ) ) ;
#226 = AXIS2_PLACEMENT_3D ( 'NONE', #11748, #5679, #26519 ) ;
#227 = CARTESIAN_POINT ( 'NONE',  ( -57.72247103062156270, 205.6499508600178956, 7.303452534266880569 ) ) ;
#228 = CARTESIAN_POINT ( 'NONE',  ( 7.228626920339068285, 6.672686282101436106, -10.49813415415989581 ) ) ;
#229 = CARTESIAN_POINT ( 'NONE',  ( 11.61527771782819940, 44.33518628210145351, -4.622313124798573369 ) ) ;
#230 = AXIS2_PLACEMENT_3D ( 'NONE', #7909, #4677, #5414 ) ;
#231 = CARTESIAN_POINT ( 'NONE',  ( 10.56230152254410726, 0.000000000000000000, -3.600000000000047606 ) ) ;
#232 = ORIENTED_EDGE ( 'NONE', *, *, #9936, .F. ) ;
#233 = CARTESIAN_POINT ( 'NONE',  ( -36.74330436395489841, 210.1155267958017134, -6.500000000000000888 ) ) ;
#234 = CARTESIAN_POINT ( 'NONE',  ( 21.00000000000000000, 242.4625000000000057, 5.999999999999998224 ) ) ;
#235 = CARTESIAN_POINT ( 'NONE',  ( 13.62178482187501416, 195.0593750006145513, 23.59362340125806767 ) ) ;
#236 = LINE ( 'NONE', #19612, #23826 ) ;
#237 = CARTESIAN_POINT ( 'NONE',  ( 26.99999999999999645, 196.3250000012290570, -15.58845726811990495 ) ) ;
#238 = DIRECTION ( 'NONE',  ( -0.000000000000000000, -0.000000000000000000, 1.000000000000000000 ) ) ;
#239 = CARTESIAN_POINT ( 'NONE',  ( 22.60769515458672885, 246.1388461906613827, 5.999999999999997335 ) ) ;
#240 = CARTESIAN_POINT ( 'NONE',  ( 21.00000000000000000, 244.5718750006145115, 6.646953231504538984 ) ) ;
#241 = CARTESIAN_POINT ( 'NONE',  ( -9.465287035748106703, 89.00231371789853085, 2.064181346179061460 ) ) ;
#242 = CARTESIAN_POINT ( 'NONE',  ( 24.81477950914817754, 0.000000000000000000, 162.4454087870936121 ) ) ;
#243 = ORIENTED_EDGE ( 'NONE', *, *, #7163, .F. ) ;
#244 = CARTESIAN_POINT ( 'NONE',  ( -53.56622103062157692, 211.6261429550005744, 6.530955311639227823 ) ) ;
#245 = CARTESIAN_POINT ( 'NONE',  ( 15.00000000000000000, 246.4562500012290513, 0.000000000000000000 ) ) ;
#246 = CARTESIAN_POINT ( 'NONE',  ( -6.932735513424201912, 106.2523137178985593, 10.69584247140429412 ) ) ;
#247 = CARTESIAN_POINT ( 'NONE',  ( 19.68408634441911076, 5.407089921784862696, -2.146874999385511629 ) ) ;
#248 = CARTESIAN_POINT ( 'NONE',  ( 20.99999999999997868, 246.9625000000000057, 5.999999999999999112 ) ) ;
#249 = CARTESIAN_POINT ( 'NONE',  ( 26.75643035624999655, 3.323476615752271712, -2.240624999385472549 ) ) ;
#250 = CARTESIAN_POINT ( 'NONE',  ( -6.932735513424201912, 69.45231371789856212, 10.69584247140429412 ) ) ;
#251 = CARTESIAN_POINT ( 'NONE',  ( 27.24356964375000345, 198.2843750006145456, -3.336375036156643733E-15 ) ) ;
#252 = ORIENTED_EDGE ( 'NONE', *, *, #5826, .F. ) ;
#253 = VERTEX_POINT ( 'NONE', #25549 ) ;
#254 = ORIENTED_EDGE ( 'NONE', *, *, #1063, .F. ) ;
#255 = CARTESIAN_POINT ( 'NONE',  ( 15.24356964374999990, 3.323476615752268604, -4.678124999385468108 ) ) ;
#256 = CARTESIAN_POINT ( 'NONE',  ( -27.00000000000000355, 195.5000000000000000, 0.000000000000000000 ) ) ;
#257 = CARTESIAN_POINT ( 'NONE',  ( 15.24356964374999990, 246.1468750006145285, 0.000000000000000000 ) ) ;
#258 = CARTESIAN_POINT ( 'NONE',  ( 11.48171059495397728, 36.28518628210144925, 4.944772684328674117 ) ) ;
#259 = CARTESIAN_POINT ( 'NONE',  ( -50.98586230271183695, 206.8500491399821328, 5.686928522499748340 ) ) ;
#260 = EDGE_CURVE ( 'NONE', #23273, #19908, #35667, .T. ) ;
#261 = CARTESIAN_POINT ( 'NONE',  ( 17.34006124879648425, 219.7598366698888981, -4.770645753573318437 ) ) ;
#262 = CARTESIAN_POINT ( 'NONE',  ( -31.39211230271183339, 205.5309553116392465, 1.321298161741817356 ) ) ;
#263 = SHAPE_REPRESENTATION_RELATIONSHIP ( 'NONE' , 'NONE' ,  #10836, #22840 ) ;
#264 = CARTESIAN_POINT ( 'NONE',  ( 27.81970530529572372, -5.196152422706632912, 162.3707280659671994 ) ) ;
#265 = CARTESIAN_POINT ( 'NONE',  ( 11.48171059495408208, 111.7148137178985650, -4.944772684328420986 ) ) ;
#266 = CARTESIAN_POINT ( 'NONE',  ( -65.44122103062156270, 208.9097554298617752, -4.530955311639240257 ) ) ;
#267 = CARTESIAN_POINT ( 'NONE',  ( -66.03497103062157692, 204.4285982733020148, -3.350049139982115509 ) ) ;
#268 = CARTESIAN_POINT ( 'NONE',  ( 26.75643035624999655, 7.049594010296217766E-16, -4.978124999385491023 ) ) ;
#269 = CARTESIAN_POINT ( 'NONE',  ( 24.00000000000000000, -5.196152422706629359, -1.650000000000012568 ) ) ;
#270 = CARTESIAN_POINT ( 'NONE',  ( 13.23911966647199812, 76.35231371789853938, 8.632099005475788900 ) ) ;
#271 = CARTESIAN_POINT ( 'NONE',  ( -52.96502896937850124, 217.3034525342667962, -4.350049139982195001 ) ) ;
#272 = ORIENTED_EDGE ( 'NONE', *, *, #322, .F. ) ;
#273 = FACE_OUTER_BOUND ( 'NONE', #13038, .T. ) ;
#274 = CARTESIAN_POINT ( 'NONE',  ( -0.1745138560725500443, 111.6101862821014521, 12.50000000000000355 ) ) ;
#275 = CARTESIAN_POINT ( 'NONE',  ( 3.257655550457285720, 52.09768628210144925, -15.46528703574804986 ) ) ;
#276 = CARTESIAN_POINT ( 'NONE',  ( 33.95006120609467359, 5.407089921784862696, 162.2014130487530110 ) ) ;
#277 = CARTESIAN_POINT ( 'NONE',  ( -13.23911966647218463, 67.04768628210143788, 8.632099005475506459 ) ) ;
#278 = CARTESIAN_POINT ( 'NONE',  ( -44.35000000000001563, 244.5000000000000000, -5.000000000000001776 ) ) ;
#279 = CARTESIAN_POINT ( 'NONE',  ( 22.80587116629410716, 7.646167579472015790E-16, -9.365624999385563143 ) ) ;
#280 = CARTESIAN_POINT ( 'NONE',  ( 24.71019261795870037, -3.464101615138094559, 161.2499751506078383 ) ) ;
#281 = CARTESIAN_POINT ( 'NONE',  ( -50.59747103062156270, 213.3500491399821328, -5.571401726697985168 ) ) ;
#282 = LINE ( 'NONE', #23417, #32949 ) ;
#283 = CARTESIAN_POINT ( 'NONE',  ( -7.228626920339069173, 48.07268628210143646, 10.49813415415989581 ) ) ;
#284 = CARTESIAN_POINT ( 'NONE',  ( -26.99999999999998934, 195.9875000000000114, 15.58845726811991561 ) ) ;
#285 = DIRECTION ( 'NONE',  ( 1.000000000000000000, 0.000000000000000000, 0.000000000000000000 ) ) ;
#286 = CARTESIAN_POINT ( 'NONE',  ( -6.840914352312096547, 11.56018628210145316, 6.594114490232313663 ) ) ;
#287 = CARTESIAN_POINT ( 'NONE',  ( 20.99999999999999645, 245.9218750006145626, 6.646953231504538984 ) ) ;
#288 = ORIENTED_EDGE ( 'NONE', *, *, #7515, .F. ) ;
#289 = CARTESIAN_POINT ( 'NONE',  ( 15.00000000000000000, 3.464101615137752166, -3.637499999999994849 ) ) ;
#290 = CARTESIAN_POINT ( 'NONE',  ( 34.18580599575048495, -5.196152422706635576, 166.2933124484913492 ) ) ;
#291 = CARTESIAN_POINT ( 'NONE',  ( 20.99999999999999645, 185.0294372515228645, -5.999999999999999112 ) ) ;
#292 = CARTESIAN_POINT ( 'NONE',  ( 10.31873187879411269, 3.604726614523236616, -4.228124999385536320 ) ) ;
#293 = CARTESIAN_POINT ( 'NONE',  ( 34.37331128181295270, -5.407089921784855591, 167.0391835513610488 ) ) ;
#294 =( BOUNDED_SURFACE ( )  B_SPLINE_SURFACE ( 3, 2, ( 
 ( #18814, #1535, #16329, #12732, #30357, #24662, #4381, #10074, #36214, #10256, #21466, #27877, #18433, #18626, #1349, #16146, #21832, #33386, #35842, #32814, #30167, #12921, #7426, #1908, #13478, #15771, #18995, #30552, #27696, #1724, #1160, #24484, #25030, #24849, #4194, #13293, #36399, #22020, #33573, #7609, #36589, #29974, #15579, #27133, #24299, #22575, #25406, #7981, #16516, #20099, #36957, #28063, #16704, #8533, #14222, #33939, #22389, #22760, #19554, #14040, #5486, #31648, #10818, #37144, #28252, #11003, #34121, #8171, #31103, #2098, #5675, #2466, #2281, #11186, #34309, #22946, #28609, #4934, #19746, #5124, #13858, #31283, #30915, #5311, #7796, #19926, #16889, #8353, #28425, #13676, #25589, #31464, #25224, #19373, #22207, #17069, #2646, #25772, #36773, #37324, #34492, #11374, #17256, #28795, #2833, #14405, #25961, #26889, #33756, #178, #26898, #12112, #21043, #17822, #35417, #8900, #545, #14592, #363, #20854, #5864, #23685, #18007, #29736, #12305, #26515, #35231, #26327, #9281, #34673, #20477, #29359, #11927, #32393, #23496, #6433, #3398, #35045, #9093, #6245, #20662, #26144, #29551, #3590, #14967, #15152, #26703, #23879, #734, #32208, #9468, #32580, #28981, #6621, #18197, #3770, #15344, #11556, #23130, #11744, #8718, #20290, #23313, #6047, #31830, #17442, #3022, #34860, #32016, #17633, #29165, #3209, #14783, #7565, #21417, #21604, #4335, #35987, #1117, #1490, #12683, #30311, #21789, #10402, #27092, #15914, #7011, #4153, #1302, #15724, #24254, #32772, #36355, #18770, #18580, #27463, #13064, #1679, #7380, #21233, #12871, #35798, #32960, #9840, #9655, #30122, #24065, #36169, #27274, #24621, #24438, #6807, #10023, #33153, #18383, #35611, #928, #7198, #10215, #33341, #29933, #18951, #13254, #30505, #4525, #21977, #16101, #27653, #24803, #3961, #33522, #19140, #16287, #30689, #4707, #12498, #15535, #25180, #16848, #30870, #16661, #37099, #22164, #2423, #34268, #8494, #28569, #5269, #28386, #5083, #13996, #13435, #36732, #8130, #28207, #25548, #2237, #11148, #34078, #13816, #25363, #22532, #36910, #4893, #22723, #8312, #19701, #19883, #31426, #2607, #31240, #10958, #5447, #25735, #7748, #17029, #14181, #37287, #11335, #22905, #34452, #16474, #20062, #1864, #28019, #22345, #31606, #5633, #27834, #2052, #24984, #10772, #33895, #36542, #10585, #33708, #7937, #19331, #13630, #19513, #31059, #23087, #11700, #3548, #9237, #28944, #6009, #32164, #23454, #17593, #3166, #11886, #31980, #20248, #3356, #23647, #35008, #506, #6202, #29507, #9051, #29124, #20622, #15111, #34631, #14739, #17774, #26287, #320, #29317, #14925, #31788, #26662, #28755, #17404, #23274, #26473, #12072, #35190, #5824, #32538, #14551, #34818, #20811, #692, #23834, #137, #32353, #6392, #17965, #12263, #8676, #8861, #35375, #9426, #2982, #26104, #21003, #20437, #17217, #2795, #14367, #25922, #37467, #11517, #9797, #6968, #21375, #29887, #883, #4982, #24394, #24207, #21563, #7656, #7842, #13524, #26854, #18536, #3918, #1073, #18339, #15301, #6765, #29695, #4799, #32914, #30776, #12643, #12455, #15491, #4110, #24024, #3729, #6578, #30075, #9982, #16377, #35569, #35942, #19415, #33108, #19233, #16565, #1953, #27923, #25080, #9614, #36635, #32728, #22437, #10674, #28110, #12826, #30964, #27047, #22253, #21188, #15682, #33805, #35752, #2141, #13721, #25270, #36821, #10863, #18154, #27233, #1257, #19601, #5356, #14273, #22807, #8580, #25452, #34541, #31511, #25824, #31150, #20149, #23178, #17306, #33983, #17492, #11791, #29027, #28659, #2333, #2697, #28295, #37192, #34171, #37005, #37372, #13904, #11424, #5534, #22991, #11235, #8027, #14641, #22624, #14453, #31696, #5724, #11603, #26190, #34723, #34356, #228, #17121, #28846, #3071, #8401, #11049, #5913, #8216, #2881, #5169, #26009, #19969 ),
 ( #38, #16747, #8767, #20341, #19791, #31883, #31328, #16934, #28476, #2515, #14086, #25637, #8956, #35276, #20902, #17681, #6673, #29218, #23738, #9333, #18246, #1166, #23359, #32443, #6487, #34911, #12164, #15015, #6097, #20527, #23550, #12357, #17869, #26566, #595, #32069, #27139, #24118, #3260, #29981, #3823, #14833, #35095, #26757, #26377, #18058, #29601, #29414, #411, #3638, #11978, #9522, #15208, #787, #23929, #32254, #32634, #35471, #21094, #4013, #29791, #9144, #15400, #26946, #20711, #976, #6295, #21284, #3445, #12552, #35661, #9708, #32820, #6865, #18440, #15585, #7431, #12738, #30173, #1356, #13115, #7245, #36038, #18633, #24305, #27328, #24491, #21651, #4576, #27702, #12927, #18819, #15965, #30363, #10082, #7063, #33205, #30558, #21839, #15778, #4387, #1543, #27518, #24669, #36221, #16153, #4201, #10263, #33391, #19001, #35848, #9890, #21474, #33013, #7003, #26887, #26694, #24055, #9646, #9831, #15527, #29351, #21034, #32385, #3581, #20843, #17809, #9272, #32200, #6799, #35409, #32763, #15144, #3390, #17999, #6612, #26506, #6235, #9085, #32571, #12488, #18373, #14960, #920, #21409, #35601, #21223, #18572, #3952, #29921, #27082, #12104, #1107, #35222, #24430, #12675, #30115, #15335, #32948, #6425, #24244, #23677, #9457, #35789, #538, #4144, #15716, #27267, #1292, #12864, #20654, #23868, #29542, #723, #12296, #18187, #29728, #3761, #7622, #13121, #7810, #10455, #36229, #25236, #21658, #16528, #33770, #10270, #18825, #10640, #1737, #21845, #36600, #33398, #2109, #30369, #7437, #25045, #15972, #22031, #33584, #27708, #4392, #19198, #27524, #19387, #30746, #16341, #13305, #30565, #30929, #4946, #22218, #2296, #28075, #19007, #27890, #13688, #4583, #36785, #1549, #24675, #10830, #4768, #13488, #16159, #22403, #33952, #7993, #33211, #5136, #36973, #16717, #1920, #24863, #19567, #36411, #31117, #28264, #13871, #25421, #7251, #25973, #8547, #5, #14239, #22591, #29183, #37160, #28995, #14419, #11571, #26159, #3225, #192, #25788, #14798, #31661, #5689, #6062, #37337, #5325, #20493, #28624, #34507, #2481, #34687, #11387, #25604, #14608, #11016, #5879, #23145, #11201, #8184, #8733, #2662, #22774, #20305, #34322, #14054, #17272, #2847, #26343, #31846, #11759, #34136, #17458, #8368, #32032, #19758, #19939, #31297, #16901, #28441, #22960, #20113, #31478, #3037, #5502, #28810, #23326, #34877, #17085, #8918, #17649, #12842, #16260, #27248, #30092, #20676, #379, #1087, #27430, #32931, #4124, #15697, #35061, #4678, #1653, #18354, #7539, #1271, #24409, #9110, #11946, #13227, #29903, #19111, #18925, #32743, #12657, #4307, #6779, #35958, #9996, #6983, #3933, #21577, #15507, #24592, #33123, #7168, #18740, #9812, #10185, #13037, #15886, #30661, #1463, #24222, #30281, #36143, #27061, #4497, #35768, #21390, #21762, #33312, #7352, #18552, #30476, #27623, #16074, #23515, #21948, #24776, #33493, #36326, #10373, #34051, #22135, #31030, #27991, #30842, #8098, #7721, #5239, #25335, #16816, #5051, #1838, #8460, #16446, #8280, #31210, #28358, #5415, #20030, #16996, #16634, #31575, #10929, #22504, #22872, #28176, #33681, #37256, #7910, #13787, #19304, #13968, #2206, #4866, #31396, #27810, #22693, #2394, #2021, #24956, #25517, #19483, #13599, #37070, #25149, #36704, #19671, #11116, #5598, #34237, #28536, #13407, #19853, #10743, #11304, #36514, #22316, #10558, #33868, #36883, #2580, #14150, #25704, #34423, #11486, #17556, #29091, #12039, #32499, #17184, #3134, #14702, #28724, #5976, #8831, #37437, #2762, #17370, #6166, #11665, #23055, #26251, #286, #23239, #25888, #11852, #14334, #3320, #23421, #34972, #20403, #26073, #26439, #29280, #32128, #35335, #17740, #28911, #9015, #14891, #5790, #20772, #34601, #8643, #471, #20585, #23606, #20211, #35152, #6357, #9203 ),
 ( #32316, #3508, #14517, #17928, #31760, #29472, #15076, #2947, #26625, #655, #9392, #12226, #23798, #20966, #31944, #101, #34787, #15456, #24361, #32880, #7298, #18689, #15644, #10136, #6927, #30038, #1219, #21341, #9578, #30231, #12986, #12792, #27380, #21528, #18872, #35904, #18499, #9947, #4443, #23989, #4072, #33074, #27194, #7118, #4256, #15832, #21152, #16022, #18118, #6733, #1035, #1410, #24543, #36092, #32689, #21892, #3882, #12606, #21709, #27571, #13168, #27008, #33259, #30421, #1600, #24723, #12418, #24172, #36274, #10319, #18306, #29846, #6545, #35716, #29660, #3696, #15264, #9764, #26817, #846, #35533, #33820, #36652, #19251, #19618, #22639, #16761, #33441, #16947, #11251, #28489, #28125, #1786, #2155, #27756, #10689, #33633, #36461, #13736, #13354, #10878, #30980, #22451, #22267, #7482, #14099, #22081, #13919, #36835, #33998, #11065, #25651, #34186, #7858, #37204, #16580, #25284, #2533, #19430, #24909, #5368, #13542, #4998, #10503, #31164, #8042, #7672, #37019, #19060, #28308, #5187, #30791, #30612, #2347, #25095, #4814, #25469, #16394, #27939, #8231, #19806, #4628, #31341, #16208, #1969, #32083, #34552, #6311, #31524, #8592, #22821, #17135, #8413, #34739, #20354, #28671, #6112, #2709, #23191, #8782, #17694, #610, #34370, #31896, #5925, #19982, #11616, #14467, #5550, #14285, #23003, #11805, #17318, #26021, #49, #25836, #26581, #23564, #37384, #29428, #3273, #11436, #20163, #26204, #31711, #17505, #29040, #28860, #5738, #3084, #2894, #8968, #14653, #241, #23375, #34924, #29233, #20540, #14846, #3462, #26394, #427, #11992, #35109, #9157, #20724, #32268, #17883, #15032, #9728, #4029, #9348, #32458, #3652, #12754, #21300, #15601, #20919, #35864, #1373, #33029, #12179, #33220, #27532, #7259, #6881, #18075, #18456, #6501, #15416, #12374, #15223, #29998, #29617, #27157, #32836, #1180, #26961, #23753, #30379, #803, #30189, #24322, #9906, #27342, #4401, #12944, #991, #15984, #21490, #7080, #18834, #12567, #26772, #21666, #29805, #35676, #23943, #18648, #24133, #35486, #15793, #35292, #4215, #24505, #9535, #21110, #36052, #3838, #32649, #10096, #6690, #18261, #33778, #30937, #16909, #4955, #16724, #13129, #10837, #13313, #22598, #10279, #24871, #1557, #33405, #24683, #13497, #36608, #7444, #22411, #19018, #1928, #25055, #33959, #36237, #21853, #10649, #22227, #30575, #27898, #30753, #4591, #16168, #1746, #28084, #33592, #4776, #16349, #27716, #5331, #2304, #36419, #8191, #19574, #10462, #22041, #16537, #7631, #7817, #19394, #19206, #2116, #13693, #25243, #36794, #8001, #31126, #5143, #28270, #13880, #25428, #36981, #19766, #11024, #34144, #31304, #29001, #17094, #32039, #29190, #17465, #3045, #387, #23334, #26166, #20313, #31486, #8742, #28633, #6269, #14614, #11953, #34695, #14806, #25795, #202, #5510, #17278, #11768, #22781, #34885, #8925, #9118, #3232, #5887, #20501, #5698, #6069, #14062, #37344, #31854, #28819, #26351, #17655, #12, #23522, #2854, #14426, #23153, #25982, #2671, #35069, #20684, #32230, #28450, #2487, #25611, #37168, #11578, #11208, #34330, #8374, #19946, #14246, #11395, #22967, #34514, #8554, #20121, #31669, #29384, #18032, #12328, #27114, #949, #6645, #20878, #33176, #15179, #23902, #18221, #27297, #24461, #760, #12524, #21256, #15369, #32606, #23711, #35444, #4175, #9862, #29575, #3613, #18407, #26726, #9679, #1137, #1328, #6461, #32795, #9492, #21068, #29761, #3792, #26919, #12136, #15746, #35632, #24087, #6831, #29955, #18603, #24277, #569, #3983, #15557, #12705, #35821, #26539, #21441, #3421, #32983, #7036, #30146, #12897, #35252, #36010, #10049, #9306, #14989, #17846, #21625, #32417, #16496, #15938, #36565, #28044, #1512, #7589, #19163, #2077, #22554, #7220, #30713, #4733, #18792, #33546, #36378, #27486 ),
 ( #10607, #13086, #16309, #27855, #13272, #24641, #1888, #4357, #30893, #13459, #25010, #10424, #16123, #13651, #19353, #22186, #25386, #33734, #7399, #7775, #4915, #33363, #10797, #36191, #10235, #25203, #36756, #22371, #21810, #33918, #7961, #19534, #30334, #28231, #18971, #2260, #31082, #30526, #5105, #4548, #21998, #27674, #1700, #16685, #24825, #13839, #36936, #10982, #37308, #8152, #14763, #22744, #14574, #37488, #23110, #11725, #26309, #23297, #11358, #345, #17238, #28779, #29147, #22929, #28407, #6031, #14205, #20084, #25570, #20273, #34474, #11170, #158, #34102, #28965, #8698, #34293, #31264, #34654, #25756, #8336, #11539, #19906, #37123, #2817, #25945, #11911, #31812, #34844, #19726, #5848, #31447, #17617, #5290, #5470, #16870, #2446, #14021, #8517, #31628, #17053, #8882, #28591, #17426, #2628, #3188, #5657, #14388, #3004, #26126, #20460, #32001, #21026, #17798, #6789, #29341, #23860, #35399, #18364, #1281, #23477, #9449, #32561, #35030, #12288, #15133, #6225, #9075, #23668, #12478, #17989, #26685, #715, #20644, #27258, #24233, #3380, #30104, #3942, #32191, #35213, #26878, #14948, #6603, #18178, #29532, #26496, #29718, #527, #9636, #3752, #15326, #909, #32377, #32752, #35591, #24046, #4135, #21213, #9262, #29912, #15518, #12094, #27072, #20834, #6416, #1097, #12665, #35778, #3573, #9821, #21399, #32939, #6993, #18563, #15707, #7921, #7548, #18750, #19121, #7178, #16083, #13047, #30672, #19314, #36524, #4688, #36715, #10196, #1848, #15896, #1662, #22144, #30292, #24965, #30852, #31042, #13612, #27819, #13417, #27633, #10567, #35969, #21772, #16270, #13236, #25160, #33692, #21958, #16457, #24786, #36336, #7731, #10382, #27442, #4877, #28001, #2033, #10755, #22327, #33879, #19495, #33503, #5561, #17146, #4317, #28682, #12853, #24421, #10006, #21588, #33135, #1473, #24603, #36152, #33322, #7361, #18933, #30486, #4507, #23573, #17702, #15042, #34933, #3095, #8978, #620, #20174, #14663, #20549, #26213, #17517, #29051, #23384, #17329, #12189, #14296, #2907, #34750, #12002, #32092, #250, #5750, #18084, #60, #8793, #11814, #23761, #9356, #23202, #6124, #29242, #3283, #14855, #8604, #20365, #26590, #32277, #14479, #26032, #26404, #11627, #437, #35118, #35300, #28872, #9167, #31908, #5938, #20734, #6320, #17892, #34564, #20927, #29437, #3473, #32466, #6509, #2721, #25849, #23014, #37397, #11447, #31722, #3847, #811, #29813, #15231, #27350, #18465, #15800, #35684, #12382, #999, #27164, #9544, #26781, #29625, #4036, #33038, #1380, #23952, #21497, #30387, #18655, #30196, #1564, #24512, #12951, #7087, #32657, #9913, #26970, #24329, #36060, #10104, #35871, #15991, #12575, #4222, #6698, #30006, #21673, #35494, #33227, #7266, #10286, #4408, #18841, #27539, #6889, #13136, #21118, #24142, #24691, #15608, #36244, #1187, #12761, #21860, #33413, #18269, #7451, #3660, #15424, #9736, #21308, #32844, #7825, #22049, #34337, #16358, #25063, #19402, #28458, #25618, #1937, #2124, #22419, #16546, #33787, #24879, #13505, #5339, #11031, #30762, #19216, #19581, #4784, #10845, #2313, #2494, #7639, #33966, #36616, #22236, #30946, #4964, #27906, #13321, #16917, #36802, #10657, #8008, #31133, #19774, #25436, #1755, #28092, #13701, #25252, #5150, #27725, #16731, #4598, #28277, #13887, #36988, #22606, #36428, #34151, #8198, #10471, #16175, #19025, #31311, #14069, #37175, #33600, #11216, #22788, #30582, #34893, #17852, #3240, #6078, #210, #11404, #26174, #5706, #3053, #14812, #32047, #14623, #32236, #17286, #8933, #22975, #34703, #17663, #2679, #20510, #26357, #26546, #9124, #23342, #29198, #23161, #393, #31494, #28827, #11776, #8750, #20691, #11959, #17474, #23529, #20321, #31862, #35075, #5896, #34523, #6275, #29391, #3427, #14995, #575, #12142, #23718, #29009, #8382 ),
 ( #2862, #19953, #5517, #17102, #28641, #14254, #14436, #25803, #37352, #20130, #8563, #31677, #25990, #20, #11586, #7227, #23909, #12714, #3799, #956, #35640, #12531, #21076, #29582, #33183, #15564, #15377, #24284, #35829, #36017, #4182, #18038, #9686, #32614, #29768, #9499, #6468, #35451, #20884, #32990, #24094, #21450, #26926, #3620, #6652, #32802, #15186, #32423, #35258, #21263, #1144, #7043, #26733, #27121, #10056, #9869, #18610, #18800, #30154, #15754, #27305, #767, #1336, #18228, #29962, #12906, #24470, #3990, #21632, #6838, #30341, #12335, #18416, #4366, #15945, #27498, #1519, #13093, #9313, #2086, #25212, #1895, #10805, #10242, #33557, #4922, #13466, #25394, #36763, #33742, #28240, #25018, #10616, #19360, #36574, #27681, #22378, #31089, #30901, #7968, #13659, #36944, #16503, #22195, #28051, #22561, #4556, #7782, #33926, #19542, #5113, #16692, #2269, #1707, #34108, #36198, #24833, #18979, #8160, #4740, #13846, #16131, #10989, #19734, #13279, #31272, #24648, #5297, #16878, #36385, #21818, #28413, #16316, #10432, #2454, #22005, #7596, #33370, #7407, #30536, #19172, #30720, #27863, #23304, #25762, #35036, #22750, #37315, #14027, #8342, #37130, #25952, #11546, #19912, #34850, #31454, #14395, #37495, #8889, #29348, #25576, #23119, #34662, #11176, #2824, #5665, #34299, #5477, #14213, #3011, #8525, #17245, #28787, #17060, #17805, #14771, #28597, #20651, #32007, #2634, #11365, #17432, #22936, #8707, #20280, #20091, #34482, #31819, #31636, #166, #5855, #28971, #14581, #26133, #20467, #11732, #6037, #32197, #17624, #29153, #3194, #26316, #353, #11918, #23484, #9081, #6231, #915, #32759, #533, #27079, #30111, #24240, #3387, #24427, #18756, #35975, #35598, #9268, #9643, #35219, #6609, #3578, #23865, #21405, #32382, #12100, #12484, #29917, #18183, #14957, #21593, #29539, #32945, #6795, #3948, #18569, #33143, #4141, #29724, #7186, #24052, #21220, #10012, #3758, #18370, #15524, #26503, #1104, #15713, #23674, #12672, #15138, #20840, #6422, #26691, #17996, #720, #12293, #15332, #35786, #35404, #9827, #9454, #26884, #6999, #27264, #21031, #32568, #1289, #12860, #8116, #19128, #21964, #13053, #30298, #30492, #19320, #24792, #33510, #7554, #27449, #34067, #31048, #10204, #36899, #10761, #1479, #4513, #33698, #24609, #30677, #4695, #36343, #36158, #16277, #21778, #16463, #27824, #24971, #1854, #1669, #2039, #4883, #7737, #10947, #30858, #16088, #36530, #28007, #18940, #33885, #33328, #7368, #13618, #13423, #22151, #27639, #25167, #19501, #36721, #4324, #13804, #15903, #25352, #10574, #13243, #22333, #10388, #7927, #5069, #16650, #28193, #2223, #22521, #17201, #8661, #22889, #31227, #304, #8297, #121, #23071, #20230, #34803, #11869, #8848, #34438, #23438, #2779, #14353, #14722, #8478, #13983, #29108, #37273, #5617, #11134, #5808, #20047, #34254, #23259, #19688, #14536, #31774, #19869, #16833, #17389, #11320, #31413, #34617, #5432, #22712, #31593, #25535, #14166, #5995, #11685, #17013, #28554, #28930, #2595, #11503, #2966, #3153, #25720, #26090, #28740, #25907, #37453, #20421, #31964, #37087, #17576, #26270, #34991, #5256, #28374, #2410, #15475, #29300, #20986, #32336, #3530, #20792, #17759, #9221, #32145, #6751, #35359, #32711, #15096, #3338, #17947, #6563, #26457, #6186, #9034, #32519, #12438, #18325, #14907, #867, #9783, #35553, #9598, #18520, #3903, #29869, #24007, #12057, #26838, #6374, #3714, #27029, #1053, #15284, #32899, #29492, #21171, #23630, #9410, #12627, #491, #24191, #35737, #27216, #21359, #6951, #30059, #23817, #4093, #35173, #26646, #15665, #18138, #1240, #12811, #29680, #24380, #20606, #675, #12246, #4464, #15852, #16227, #24929, #10342, #13374, #19079, #30811, #21913, #27591, #33462, #4834, #4277, #16042, #7504, #1620, #13191, #24745 ),
 ( #36294, #36482, #10711, #35925, #30631, #4647, #9967, #27778, #33093, #21547, #10155, #19271, #1807, #10524, #16413, #7138, #27960, #22102, #18710, #33651, #7690, #30250, #1991, #21730, #27399, #13563, #25116, #7319, #36674, #1430, #13007, #24563, #36114, #33280, #18893, #30443, #29419, #21291, #12365, #32449, #9716, #6493, #23744, #26952, #24124, #10088, #35666, #9896, #6303, #4020, #18067, #15785, #3452, #29609, #32259, #26572, #17874, #6681, #29797, #601, #15592, #12170, #32640, #18253, #27148, #15022, #35282, #3829, #15408, #9340, #21102, #23935, #20910, #3644, #15214, #32827, #26763, #35478, #9527, #794, #36044, #33019, #982, #1364, #12744, #12558, #6871, #18447, #29989, #1172, #24312, #35855, #21480, #7071, #18639, #30181, #4207, #27333, #12935, #24498, #18730, #18540, #6583, #1077, #1261, #29892, #27238, #9618, #23838, #12459, #12647, #21007, #26666, #3553, #15495, #6972, #12831, #12268, #32919, #4297, #30079, #4114, #13026, #35946, #24398, #15686, #18158, #21380, #887, #35757, #9986, #21567, #9801, #27419, #15115, #3733, #35573, #33112, #24212, #3922, #29699, #18914, #24028, #21193, #27051, #24582, #10175, #32732, #7156, #30271, #15874, #18344, #9429, #6769, #1451, #36134, #15306, #26858, #21750, #33302, #7341, #696, #35379, #32541, #7899, #36502, #33671, #30832, #7711, #16250, #24764, #28348, #10733, #10547, #19473, #31019, #31203, #36873, #13214, #4856, #27799, #24946, #8086, #5041, #33483, #27981, #28165, #19293, #16622, #22123, #36315, #1827, #2011, #10363, #16064, #30466, #16434, #33858, #2195, #1643, #22306, #5228, #13776, #25324, #2385, #10919, #22494, #34041, #7527, #19660, #13396, #25139, #16806, #13959, #36693, #25508, #13586, #37061, #19101, #11108, #22683, #21936, #34227, #8270, #4486, #27611, #30651, #4667, #34592, #5967, #5406, #28717, #92, #8635, #20576, #31935, #28902, #23412, #20203, #5782, #14507, #31752, #22864, #17546, #26242, #26063, #3124, #34778, #32119, #11654, #17360, #23230, #17729, #37246, #2937, #8821, #20394, #29082, #14692, #277, #34413, #29271, #11843, #34963, #12031, #9006, #6155, #23599, #3310, #14882, #26428, #23048, #14141, #463, #37427, #35144, #11295, #19843, #31386, #8452, #16988, #28528, #2570, #25695, #20021, #31567, #5589, #11476, #17176, #2754, #14325, #25879, #3874, #1026, #24535, #12599, #24354, #20763, #18490, #20958, #30222, #17919, #32489, #9195, #3499, #32308, #21143, #6725, #15068, #30030, #26618, #9569, #32681, #4062, #6349, #29463, #18298, #29838, #648, #35524, #839, #12218, #23789, #9382, #35707, #3689, #12407, #23980, #35328, #12978, #9939, #6537, #15822, #27186, #18110, #29653, #24163, #15256, #15448, #26999, #26809, #9758, #21333, #32872, #6919, #15635, #1211, #12784, #35896, #21519, #33065, #7109, #18680, #4248, #27372, #1402, #36642, #24716, #2147, #18864, #27563, #10681, #33623, #27930, #33250, #22260, #25276, #19422, #36084, #19608, #13910, #31156, #30783, #4434, #4806, #30411, #1779, #36266, #19053, #16571, #1592, #7290, #7664, #25087, #13345, #10127, #16753, #10311, #28116, #1961, #16386, #30972, #13532, #10870, #33812, #36453, #7849, #33990, #16015, #10493, #4988, #22072, #24902, #19241, #13728, #13160, #8034, #21701, #21883, #30604, #36828, #22443, #5176, #33433, #7474, #4621, #16199, #28301, #2339, #27749, #8406, #9104, #29371, #23510, #3220, #31333, #19973, #12317, #18019, #37197, #25643, #26527, #11240, #17835, #9294, #35432, #14091, #3409, #31516, #29178, #26339, #14792, #22813, #19797, #23891, #6258, #5540, #14978, #558, #26715, #32406, #8222, #374, #34360, #17127, #3601, #12124, #28482, #35056, #23699, #11941, #35242, #20671, #5361, #32219, #20867, #16939, #11056, #25460, #6446, #29564, #15167, #34178, #747, #9480, #21056, #32594, #6634, #18208, #29750, #3781 ),
 ( #37012, #22631, #2523, #16111, #30321, #15925, #30132, #1500, #938, #24265, #33163, #4164, #27663, #27474, #24448, #18961, #15734, #1315, #10034, #27284, #18394, #13076, #21800, #30515, #15355, #10225, #24631, #3972, #12512, #4346, #32970, #15545, #36180, #27103, #6819, #21613, #7209, #30699, #18781, #4535, #26910, #33352, #1127, #36366, #24076, #12692, #35621, #9667, #21244, #12883, #35998, #32783, #7388, #29944, #1687, #13262, #24814, #35809, #9851, #10413, #21988, #21429, #33535, #7023, #18590, #7575, #19151, #31252, #36743, #7947, #33906, #1875, #8506, #5457, #22175, #11345, #22731, #13447, #4902, #8140, #36553, #5093, #16672, #10783, #24997, #28219, #10594, #28395, #31070, #36922, #19523, #13639, #14006, #19893, #2064, #34280, #10968, #16484, #22542, #5279, #30880, #8323, #33720, #7761, #16858, #2247, #34090, #19341, #2433, #31435, #25558, #4719, #25744, #20071, #37296, #19712, #28032, #37110, #25191, #13826, #22357, #25373, #17039, #11158, #28578, #2616, #14192, #22917, #16296, #34462, #27844, #12082, #35018, #20633, #9249, #23848, #20822, #8871, #35386, #14752, #26296, #26672, #34829, #25933, #3560, #11710, #17605, #23098, #17786, #20448, #8686, #32177, #20260, #35199, #14375, #34641, #6213, #29136, #23465, #28765, #29329, #32363, #14937, #31616, #15121, #9435, #702, #332, #37476, #11898, #11528, #31990, #31798, #14562, #23656, #5836, #2805, #3176, #3366, #6019, #5644, #12275, #17414, #6402, #9062, #26484, #17975, #17227, #29519, #515, #28954, #2993, #26114, #147, #23285, #15312, #30473, #1084, #6980, #12465, #7165, #9809, #35579, #24589, #21013, #15883, #33120, #9624, #18164, #9993, #12654, #21201, #35955, #32740, #24034, #15694, #12840, #36323, #24406, #36141, #32547, #30278, #6776, #4494, #29705, #18351, #6590, #26865, #3739, #32928, #18549, #895, #4305, #29900, #21387, #30089, #27427, #3930, #15504, #4121, #27245, #27058, #1268, #24219, #35765, #21574, #18737, #1461, #13034, #10182, #21759, #33309, #24773, #7349, #18922, #27620, #16071, #1650, #13222, #13784, #4675, #10740, #22313, #16443, #19108, #33865, #7536, #34048, #36701, #5048, #2018, #19301, #19668, #25514, #7718, #28355, #16631, #10555, #28173, #2203, #25146, #13404, #8095, #16813, #25331, #31207, #36880, #22690, #10926, #7907, #22501, #8277, #27807, #19480, #5236, #31027, #2391, #13965, #37067, #24953, #19850, #21945, #22132, #4863, #11113, #34234, #31392, #36511, #25701, #30839, #27988, #5412, #16993, #28533, #13596, #2578, #14147, #10370, #33490, #16256, #30659, #1835, #33678, #11483, #37433, #283, #23052, #29088, #20582, #9202, #25885, #14699, #5787, #2944, #98, #14514, #34598, #31572, #35150, #17553, #17367, #26248, #11849, #469, #6163, #20027, #11662, #8640, #31757, #14888, #23418, #2759, #34784, #34969, #26070, #9012, #28908, #5595, #20208, #8828, #17181, #22869, #37253, #23236, #3131, #32126, #8457, #17737, #12037, #29277, #3317, #20770, #26435, #23605, #32314, #14331, #6355, #20400, #31941, #17926, #29470, #5973, #3506, #15074, #11301, #34419, #28721, #35902, #20964, #1217, #33072, #7296, #27378, #4070, #27192, #3880, #12790, #12224, #35531, #6925, #15453, #1408, #24359, #35714, #30229, #27006, #12605, #32497, #9945, #7116, #18870, #12984, #15642, #21525, #1033, #18687, #23795, #9576, #18496, #24170, #24540, #4254, #9763, #15829, #21339, #32878, #30036, #36090, #29658, #10134, #21707, #33257, #30419, #4440, #26624, #654, #35334, #9390, #6543, #18116, #3694, #15262, #26815, #844, #12415, #23987, #21149, #32687, #6731, #18304, #29844, #25282, #36649, #4812, #19058, #31339, #13352, #22079, #16392, #25467, #22637, #36459, #10687, #19428, #13539, #30789, #21890, #10499, #2345, #8040, #27754, #16206, #16577, #1784, #7855, #36833, #37017, #4626, #30978, #33630, #19248 ) ),
 .UNSPECIFIED., .T., .F., .F. ) 
 B_SPLINE_SURFACE_WITH_KNOTS ( ( 4, 3, 4 ),
 ( 3, 2, 2, 2, 2, 2, 2, 2, 2, 2, 2, 2, 2, 2, 2, 2, 2, 2, 2, 2, 2, 2, 2, 2, 2, 2, 2, 2, 2, 2, 2, 2, 2, 2, 2, 2, 2, 2, 2, 2, 2, 2, 2, 2, 2, 2, 2, 2, 2, 2, 2, 2, 2, 2, 2, 2, 2, 2, 2, 2, 2, 2, 2, 2, 2, 2, 2, 2, 2, 2, 2, 2, 2, 2, 2, 2, 2, 2, 2, 2, 2, 2, 2, 2, 2, 2, 2, 2, 2, 2, 2, 2, 2, 2, 2, 2, 2, 2, 2, 2, 2, 2, 2, 2, 2, 2, 2, 2, 2, 2, 2, 2, 2, 2, 2, 2, 2, 2, 2, 2, 2, 2, 2, 2, 2, 2, 2, 2, 2, 2, 2, 2, 2, 2, 2, 2, 2, 2, 2, 2, 2, 2, 2, 2, 2, 2, 2, 2, 2, 2, 2, 2, 2, 2, 2, 2, 2, 2, 2, 2, 2, 2, 2, 2, 2, 2, 2, 2, 2, 2, 2, 2, 2, 2, 2, 2, 2, 2, 2, 2, 2, 2, 2, 2, 2, 2, 2, 2, 2, 2, 2, 2, 2, 2, 2, 2, 2, 2, 2, 2, 2, 2, 2, 2, 2, 2, 2, 2, 2, 2, 2, 2, 2, 2, 2, 2, 2, 2, 2, 2, 2, 2, 2, 2, 2, 2, 2, 2, 2, 2, 2, 2, 2, 2, 2, 2, 2, 2, 2, 2, 3 ),
 ( 0.000000000000000000, 0.5000000000000000000, 1.000000000000000000 ),
 ( 0.000000000000000000, 0.004166666666666666609, 0.008333333333333333218, 0.01250000000000000069, 0.01666666666666666644, 0.02083333333333333218, 0.02500000000000000139, 0.02916666666666666713, 0.03333333333333333287, 0.03749999999999999861, 0.04166666666666666435, 0.04583333333333333010, 0.05000000000000000278, 0.05416666666666666852, 0.05833333333333333426, 0.06250000000000000000, 0.06666666666666666574, 0.07083333333333333148, 0.07499999999999999722, 0.07916666666666666297, 0.08333333333333332871, 0.08749999999999999445, 0.09166666666666666019, 0.09583333333333333981, 0.1000000000000000056, 0.1041666666666666713, 0.1083333333333333370, 0.1125000000000000028, 0.1166666666666666685, 0.1208333333333333343, 0.1250000000000000000, 0.1291666666666666796, 0.1333333333333333315, 0.1375000000000000111, 0.1416666666666666630, 0.1458333333333333426, 0.1499999999999999944, 0.1541666666666666741, 0.1583333333333333259, 0.1625000000000000056, 0.1666666666666666574, 0.1708333333333333370, 0.1749999999999999889, 0.1791666666666666685, 0.1833333333333333204, 0.1875000000000000000, 0.1916666666666666796, 0.1958333333333333315, 0.2000000000000000111, 0.2041666666666666630, 0.2083333333333333426, 0.2124999999999999944, 0.2166666666666666741, 0.2208333333333333259, 0.2250000000000000056, 0.2291666666666666574, 0.2333333333333333370, 0.2374999999999999889, 0.2416666666666666685, 0.2458333333333333204, 0.2500000000000000000, 0.2541666666666666519, 0.2583333333333333592, 0.2625000000000000111, 0.2666666666666666630, 0.2708333333333333148, 0.2750000000000000222, 0.2791666666666666741, 0.2833333333333333259, 0.2874999999999999778, 0.2916666666666666852, 0.2958333333333333370, 0.2999999999999999889, 0.3041666666666666408, 0.3083333333333333481, 0.3125000000000000000, 0.3166666666666666519, 0.3208333333333333592, 0.3250000000000000111, 0.3291666666666666630, 0.3333333333333333148, 0.3375000000000000222, 0.3416666666666666741, 0.3458333333333333259, 0.3499999999999999778, 0.3541666666666666852, 0.3583333333333333370, 0.3624999999999999889, 0.3666666666666666408, 0.3708333333333333481, 0.3750000000000000000, 0.3791666666666666519, 0.3833333333333333592, 0.3875000000000000111, 0.3916666666666666630, 0.3958333333333333148, 0.4000000000000000222, 0.4041666666666666741, 0.4083333333333333259, 0.4124999999999999778, 0.4166666666666666852, 0.4208333333333333370, 0.4249999999999999889, 0.4291666666666666408, 0.4333333333333333481, 0.4375000000000000000, 0.4416666666666666519, 0.4458333333333333592, 0.4500000000000000111, 0.4541666666666666630, 0.4583333333333333148, 0.4625000000000000222, 0.4666666666666666741, 0.4708333333333333259, 0.4749999999999999778, 0.4791666666666666852, 0.4833333333333333370, 0.4874999999999999889, 0.4916666666666666408, 0.4958333333333333481, 0.5000000000000000000, 0.5041666666666666519, 0.5083333333333333037, 0.5124999999999999556, 0.5166666666666667185, 0.5208333333333333703, 0.5250000000000000222, 0.5291666666666666741, 0.5333333333333333259, 0.5374999999999999778, 0.5416666666666666297, 0.5458333333333332815, 0.5500000000000000444, 0.5541666666666666963, 0.5583333333333333481, 0.5625000000000000000, 0.5666666666666666519, 0.5708333333333333037, 0.5749999999999999556, 0.5791666666666667185, 0.5833333333333333703, 0.5875000000000000222, 0.5916666666666666741, 0.5958333333333333259, 0.5999999999999999778, 0.6041666666666666297, 0.6083333333333332815, 0.6125000000000000444, 0.6166666666666666963, 0.6208333333333333481, 0.6250000000000000000, 0.6291666666666666519, 0.6333333333333333037, 0.6374999999999999556, 0.6416666666666667185, 0.6458333333333333703, 0.6500000000000000222, 0.6541666666666666741, 0.6583333333333333259, 0.6624999999999999778, 0.6666666666666666297, 0.6708333333333332815, 0.6750000000000000444, 0.6791666666666666963, 0.6833333333333333481, 0.6875000000000000000, 0.6916666666666666519, 0.6958333333333333037, 0.6999999999999999556, 0.7041666666666667185, 0.7083333333333333703, 0.7125000000000000222, 0.7166666666666666741, 0.7208333333333333259, 0.7249999999999999778, 0.7291666666666666297, 0.7333333333333332815, 0.7375000000000000444, 0.7416666666666666963, 0.7458333333333333481, 0.7500000000000000000, 0.7541666666666666519, 0.7583333333333333037, 0.7624999999999999556, 0.7666666666666667185, 0.7708333333333333703, 0.7750000000000000222, 0.7791666666666666741, 0.7833333333333333259, 0.7874999999999999778, 0.7916666666666666297, 0.7958333333333332815, 0.8000000000000000444, 0.8041666666666666963, 0.8083333333333333481, 0.8125000000000000000, 0.8166666666666666519, 0.8208333333333333037, 0.8249999999999999556, 0.8291666666666667185, 0.8333333333333333703, 0.8375000000000000222, 0.8416666666666666741, 0.8458333333333333259, 0.8499999999999999778, 0.8541666666666666297, 0.8583333333333332815, 0.8625000000000000444, 0.8666666666666666963, 0.8708333333333333481, 0.8750000000000000000, 0.8791666666666666519, 0.8833333333333333037, 0.8874999999999999556, 0.8916666666666667185, 0.8958333333333333703, 0.9000000000000000222, 0.9041666666666666741, 0.9083333333333333259, 0.9124999999999999778, 0.9166666666666666297, 0.9208333333333332815, 0.9250000000000000444, 0.9291666666666666963, 0.9333333333333333481, 0.9375000000000000000, 0.9416666666666666519, 0.9458333333333333037, 0.9499999999999999556, 0.9541666666666667185, 0.9583333333333333703, 0.9625000000000000222, 0.9666666666666666741, 0.9708333333333333259, 0.9749999999999999778, 0.9791666666666666297, 0.9833333333333332815, 0.9875000000000000444, 0.9916666666666666963, 0.9958333333333333481, 1.000000000000000000 ),
 .UNSPECIFIED. ) 
 GEOMETRIC_REPRESENTATION_ITEM ( )  RATIONAL_B_SPLINE_SURFACE ( (
 ( 1.000000000000000000, 0.9807852804032304306, 1.000000000000000000, 0.9807852804032304306, 1.000000000000000000, 0.9807852804032304306, 1.000000000000000000, 0.9807852804032304306, 1.000000000000000000, 0.9807852804032304306, 1.000000000000000000, 0.9807852804032304306, 1.000000000000000000, 0.9807852804032304306, 1.000000000000000000, 0.9807852804032304306, 1.000000000000000000, 0.9807852804032304306, 1.000000000000000000, 0.9807852804032304306, 1.000000000000000000, 0.9807852804032304306, 1.000000000000000000, 0.9807852804032304306, 1.000000000000000000, 0.9807852804032304306, 1.000000000000000000, 0.9807852804032304306, 1.000000000000000000, 0.9807852804032304306, 1.000000000000000000, 0.9807852804032304306, 1.000000000000000000, 0.9807852804032304306, 1.000000000000000000, 0.9807852804032304306, 1.000000000000000000, 0.9807852804032304306, 1.000000000000000000, 0.9807852804032304306, 1.000000000000000000, 0.9807852804032304306, 1.000000000000000000, 0.9807852804032304306, 1.000000000000000000, 0.9807852804032304306, 1.000000000000000000, 0.9807852804032304306, 1.000000000000000000, 0.9807852804032304306, 1.000000000000000000, 0.9807852804032304306, 1.000000000000000000, 0.9807852804032304306, 1.000000000000000000, 0.9807852804032304306, 1.000000000000000000, 0.9807852804032304306, 1.000000000000000000, 0.9807852804032304306, 1.000000000000000000, 0.9807852804032304306, 1.000000000000000000, 0.9807852804032304306, 1.000000000000000000, 0.9807852804032304306, 1.000000000000000000, 0.9807852804032304306, 1.000000000000000000, 0.9807852804032304306, 1.000000000000000000, 0.9807852804032304306, 1.000000000000000000, 0.9807852804032304306, 1.000000000000000000, 0.9807852804032304306, 1.000000000000000000, 0.9807852804032304306, 1.000000000000000000, 0.9807852804032304306, 1.000000000000000000, 0.9807852804032304306, 1.000000000000000000, 0.9807852804032304306, 1.000000000000000000, 0.9807852804032304306, 1.000000000000000000, 0.9807852804032304306, 1.000000000000000000, 0.9807852804032304306, 1.000000000000000000, 0.9807852804032304306, 1.000000000000000000, 0.9807852804032304306, 1.000000000000000000, 0.9807852804032304306, 1.000000000000000000, 0.9807852804032304306, 1.000000000000000000, 0.9807852804032304306, 1.000000000000000000, 0.9807852804032304306, 1.000000000000000000, 0.9807852804032304306, 1.000000000000000000, 0.9807852804032304306, 1.000000000000000000, 0.9807852804032304306, 1.000000000000000000, 0.9807852804032304306, 1.000000000000000000, 0.9807852804032304306, 1.000000000000000000, 0.9807852804032304306, 1.000000000000000000, 0.9807852804032304306, 1.000000000000000000, 0.9807852804032304306, 1.000000000000000000, 0.9807852804032304306, 1.000000000000000000, 0.9807852804032304306, 1.000000000000000000, 0.9807852804032304306, 1.000000000000000000, 0.9807852804032304306, 1.000000000000000000, 0.9807852804032304306, 1.000000000000000000, 0.9807852804032304306, 1.000000000000000000, 0.9807852804032304306, 1.000000000000000000, 0.9807852804032304306, 1.000000000000000000, 0.9807852804032304306, 1.000000000000000000, 0.9807852804032304306, 1.000000000000000000, 0.9807852804032304306, 1.000000000000000000, 0.9807852804032304306, 1.000000000000000000, 0.9807852804032304306, 1.000000000000000000, 0.9807852804032304306, 1.000000000000000000, 0.9807852804032304306, 1.000000000000000000, 0.9807852804032304306, 1.000000000000000000, 0.9807852804032304306, 1.000000000000000000, 0.9807852804032304306, 1.000000000000000000, 0.9807852804032304306, 1.000000000000000000, 0.9807852804032304306, 1.000000000000000000, 0.9807852804032304306, 1.000000000000000000, 0.9807852804032304306, 1.000000000000000000, 0.9807852804032304306, 1.000000000000000000, 0.9807852804032304306, 1.000000000000000000, 0.9807852804032304306, 1.000000000000000000, 0.9807852804032304306, 1.000000000000000000, 0.9807852804032304306, 1.000000000000000000, 0.9807852804032304306, 1.000000000000000000, 0.9807852804032304306, 1.000000000000000000, 0.9807852804032304306, 1.000000000000000000, 0.9807852804032304306, 1.000000000000000000, 0.9807852804032304306, 1.000000000000000000, 0.9807852804032304306, 1.000000000000000000, 0.9807852804032304306, 1.000000000000000000, 0.9807852804032304306, 1.000000000000000000, 0.9807852804032304306, 1.000000000000000000, 0.9807852804032304306, 1.000000000000000000, 0.9807852804032304306, 1.000000000000000000, 0.9807852804032304306, 1.000000000000000000, 0.9807852804032304306, 1.000000000000000000, 0.9807852804032304306, 1.000000000000000000, 0.9807852804032304306, 1.000000000000000000, 0.9807852804032304306, 1.000000000000000000, 0.9807852804032304306, 1.000000000000000000, 0.9807852804032304306, 1.000000000000000000, 0.9807852804032304306, 1.000000000000000000, 0.9807852804032304306, 1.000000000000000000, 0.9807852804032304306, 1.000000000000000000, 0.9807852804032304306, 1.000000000000000000, 0.9807852804032304306, 1.000000000000000000, 0.9807852804032304306, 1.000000000000000000, 0.9807852804032304306, 1.000000000000000000, 0.9807852804032304306, 1.000000000000000000, 0.9807852804032304306, 1.000000000000000000, 0.9807852804032304306, 1.000000000000000000, 0.9807852804032304306, 1.000000000000000000, 0.9807852804032304306, 1.000000000000000000, 0.9807852804032304306, 1.000000000000000000, 0.9807852804032304306, 1.000000000000000000, 0.9807852804032304306, 1.000000000000000000, 0.9807852804032304306, 1.000000000000000000, 0.9807852804032304306, 1.000000000000000000, 0.9807852804032304306, 1.000000000000000000, 0.9807852804032304306, 1.000000000000000000, 0.9807852804032304306, 1.000000000000000000, 0.9807852804032304306, 1.000000000000000000, 0.9807852804032304306, 1.000000000000000000, 0.9807852804032304306, 1.000000000000000000, 0.9807852804032304306, 1.000000000000000000, 0.9807852804032304306, 1.000000000000000000, 0.9807852804032304306, 1.000000000000000000, 0.9807852804032304306, 1.000000000000000000, 0.9807852804032304306, 1.000000000000000000, 0.9807852804032304306, 1.000000000000000000, 0.9807852804032304306, 1.000000000000000000, 0.9807852804032304306, 1.000000000000000000, 0.9807852804032304306, 1.000000000000000000, 0.9807852804032304306, 1.000000000000000000, 0.9807852804032304306, 1.000000000000000000, 0.9807852804032304306, 1.000000000000000000, 0.9807852804032304306, 1.000000000000000000, 0.9807852804032304306, 1.000000000000000000, 0.9807852804032304306, 1.000000000000000000, 0.9807852804032304306, 1.000000000000000000, 0.9807852804032304306, 1.000000000000000000, 0.9807852804032304306, 1.000000000000000000, 0.9807852804032304306, 1.000000000000000000, 0.9807852804032304306, 1.000000000000000000, 0.9807852804032304306, 1.000000000000000000, 0.9807852804032304306, 1.000000000000000000, 0.9807852804032304306, 1.000000000000000000, 0.9807852804032304306, 1.000000000000000000, 0.9807852804032304306, 1.000000000000000000, 0.9807852804032304306, 1.000000000000000000, 0.9807852804032304306, 1.000000000000000000, 0.9807852804032304306, 1.000000000000000000, 0.9807852804032304306, 1.000000000000000000, 0.9807852804032304306, 1.000000000000000000, 0.9807852804032304306, 1.000000000000000000, 0.9807852804032304306, 1.000000000000000000, 0.9807852804032304306, 1.000000000000000000, 0.9807852804032304306, 1.000000000000000000, 0.9807852804032304306, 1.000000000000000000, 0.9807852804032304306, 1.000000000000000000, 0.9807852804032304306, 1.000000000000000000, 0.9807852804032304306, 1.000000000000000000, 0.9807852804032304306, 1.000000000000000000, 0.9807852804032304306, 1.000000000000000000, 0.9807852804032304306, 1.000000000000000000, 0.9807852804032304306, 1.000000000000000000, 0.9807852804032304306, 1.000000000000000000, 0.9807852804032304306, 1.000000000000000000, 0.9807852804032304306, 1.000000000000000000, 0.9807852804032304306, 1.000000000000000000, 0.9807852804032304306, 1.000000000000000000, 0.9807852804032304306, 1.000000000000000000, 0.9807852804032304306, 1.000000000000000000, 0.9807852804032304306, 1.000000000000000000, 0.9807852804032304306, 1.000000000000000000, 0.9807852804032304306, 1.000000000000000000, 0.9807852804032304306, 1.000000000000000000, 0.9807852804032304306, 1.000000000000000000, 0.9807852804032304306, 1.000000000000000000, 0.9807852804032304306, 1.000000000000000000, 0.9807852804032304306, 1.000000000000000000, 0.9807852804032304306, 1.000000000000000000, 0.9807852804032304306, 1.000000000000000000, 0.9807852804032304306, 1.000000000000000000, 0.9807852804032304306, 1.000000000000000000, 0.9807852804032304306, 1.000000000000000000, 0.9807852804032304306, 1.000000000000000000, 0.9807852804032304306, 1.000000000000000000, 0.9807852804032304306, 1.000000000000000000, 0.9807852804032304306, 1.000000000000000000, 0.9807852804032304306, 1.000000000000000000, 0.9807852804032304306, 1.000000000000000000, 0.9807852804032304306, 1.000000000000000000, 0.9807852804032304306, 1.000000000000000000, 0.9807852804032304306, 1.000000000000000000, 0.9807852804032304306, 1.000000000000000000, 0.9807852804032304306, 1.000000000000000000, 0.9807852804032304306, 1.000000000000000000, 0.9807852804032304306, 1.000000000000000000, 0.9807852804032304306, 1.000000000000000000, 0.9807852804032304306, 1.000000000000000000, 0.9807852804032304306, 1.000000000000000000, 0.9807852804032304306, 1.000000000000000000, 0.9807852804032304306, 1.000000000000000000, 0.9807852804032304306, 1.000000000000000000, 0.9807852804032304306, 1.000000000000000000, 0.9807852804032304306, 1.000000000000000000, 0.9807852804032304306, 1.000000000000000000, 0.9807852804032304306, 1.000000000000000000, 0.9807852804032304306, 1.000000000000000000, 0.9807852804032304306, 1.000000000000000000, 0.9807852804032304306, 1.000000000000000000, 0.9807852804032304306, 1.000000000000000000, 0.9807852804032304306, 1.000000000000000000, 0.9807852804032304306, 1.000000000000000000, 0.9807852804032304306, 1.000000000000000000, 0.9807852804032304306, 1.000000000000000000, 0.9807852804032304306, 1.000000000000000000, 0.9807852804032304306, 1.000000000000000000, 0.9807852804032304306, 1.000000000000000000, 0.9807852804032304306, 1.000000000000000000, 0.9807852804032304306, 1.000000000000000000, 0.9807852804032304306, 1.000000000000000000, 0.9807852804032304306, 1.000000000000000000, 0.9807852804032304306, 1.000000000000000000, 0.9807852804032304306, 1.000000000000000000, 0.9807852804032304306, 1.000000000000000000, 0.9807852804032304306, 1.000000000000000000, 0.9807852804032304306, 1.000000000000000000, 0.9807852804032304306, 1.000000000000000000, 0.9807852804032304306, 1.000000000000000000, 0.9807852804032304306, 1.000000000000000000, 0.9807852804032304306, 1.000000000000000000, 0.9807852804032304306, 1.000000000000000000, 0.9807852804032304306, 1.000000000000000000, 0.9807852804032304306, 1.000000000000000000, 0.9807852804032304306, 1.000000000000000000),
 ( 0.3333333333333333703, 0.3269284268010768657, 0.3333333333333333703, 0.3269284268010768657, 0.3333333333333333703, 0.3269284268010768657, 0.3333333333333333703, 0.3269284268010768657, 0.3333333333333333703, 0.3269284268010768657, 0.3333333333333333703, 0.3269284268010768657, 0.3333333333333333703, 0.3269284268010768657, 0.3333333333333333703, 0.3269284268010768657, 0.3333333333333333703, 0.3269284268010768657, 0.3333333333333333703, 0.3269284268010768657, 0.3333333333333333703, 0.3269284268010768657, 0.3333333333333333703, 0.3269284268010768657, 0.3333333333333333703, 0.3269284268010768657, 0.3333333333333333703, 0.3269284268010768657, 0.3333333333333333703, 0.3269284268010768657, 0.3333333333333333703, 0.3269284268010768657, 0.3333333333333333703, 0.3269284268010768657, 0.3333333333333333703, 0.3269284268010768657, 0.3333333333333333703, 0.3269284268010768657, 0.3333333333333333703, 0.3269284268010768657, 0.3333333333333333703, 0.3269284268010768657, 0.3333333333333333703, 0.3269284268010768657, 0.3333333333333333703, 0.3269284268010768657, 0.3333333333333333703, 0.3269284268010768657, 0.3333333333333333703, 0.3269284268010768657, 0.3333333333333333703, 0.3269284268010768657, 0.3333333333333333703, 0.3269284268010768657, 0.3333333333333333703, 0.3269284268010768657, 0.3333333333333333703, 0.3269284268010768657, 0.3333333333333333703, 0.3269284268010768657, 0.3333333333333333703, 0.3269284268010768657, 0.3333333333333333703, 0.3269284268010768657, 0.3333333333333333703, 0.3269284268010768657, 0.3333333333333333703, 0.3269284268010768657, 0.3333333333333333703, 0.3269284268010768657, 0.3333333333333333703, 0.3269284268010768657, 0.3333333333333333703, 0.3269284268010768657, 0.3333333333333333703, 0.3269284268010768657, 0.3333333333333333703, 0.3269284268010768657, 0.3333333333333333703, 0.3269284268010768657, 0.3333333333333333703, 0.3269284268010768657, 0.3333333333333333703, 0.3269284268010768657, 0.3333333333333333703, 0.3269284268010768657, 0.3333333333333333703, 0.3269284268010768657, 0.3333333333333333703, 0.3269284268010768657, 0.3333333333333333703, 0.3269284268010768657, 0.3333333333333333703, 0.3269284268010768657, 0.3333333333333333703, 0.3269284268010768657, 0.3333333333333333703, 0.3269284268010768657, 0.3333333333333333703, 0.3269284268010768657, 0.3333333333333333703, 0.3269284268010768657, 0.3333333333333333703, 0.3269284268010768657, 0.3333333333333333703, 0.3269284268010768657, 0.3333333333333333703, 0.3269284268010768657, 0.3333333333333333703, 0.3269284268010768657, 0.3333333333333333703, 0.3269284268010768657, 0.3333333333333333703, 0.3269284268010768657, 0.3333333333333333703, 0.3269284268010768657, 0.3333333333333333703, 0.3269284268010768657, 0.3333333333333333703, 0.3269284268010768657, 0.3333333333333333703, 0.3269284268010768657, 0.3333333333333333703, 0.3269284268010768657, 0.3333333333333333703, 0.3269284268010768657, 0.3333333333333333703, 0.3269284268010768657, 0.3333333333333333703, 0.3269284268010768657, 0.3333333333333333703, 0.3269284268010768657, 0.3333333333333333703, 0.3269284268010768657, 0.3333333333333333703, 0.3269284268010768657, 0.3333333333333333703, 0.3269284268010768657, 0.3333333333333333703, 0.3269284268010768657, 0.3333333333333333703, 0.3269284268010768657, 0.3333333333333333703, 0.3269284268010768657, 0.3333333333333333703, 0.3269284268010768657, 0.3333333333333333703, 0.3269284268010768657, 0.3333333333333333703, 0.3269284268010768657, 0.3333333333333333703, 0.3269284268010768657, 0.3333333333333333703, 0.3269284268010768657, 0.3333333333333333703, 0.3269284268010768657, 0.3333333333333333703, 0.3269284268010768657, 0.3333333333333333703, 0.3269284268010768657, 0.3333333333333333703, 0.3269284268010768657, 0.3333333333333333703, 0.3269284268010768657, 0.3333333333333333703, 0.3269284268010768657, 0.3333333333333333703, 0.3269284268010768657, 0.3333333333333333703, 0.3269284268010768657, 0.3333333333333333703, 0.3269284268010768657, 0.3333333333333333703, 0.3269284268010768657, 0.3333333333333333703, 0.3269284268010768657, 0.3333333333333333703, 0.3269284268010768657, 0.3333333333333333703, 0.3269284268010768657, 0.3333333333333333703, 0.3269284268010768657, 0.3333333333333333703, 0.3269284268010768657, 0.3333333333333333703, 0.3269284268010768657, 0.3333333333333333703, 0.3269284268010768657, 0.3333333333333333703, 0.3269284268010768657, 0.3333333333333333703, 0.3269284268010768657, 0.3333333333333333703, 0.3269284268010768657, 0.3333333333333333703, 0.3269284268010768657, 0.3333333333333333703, 0.3269284268010768657, 0.3333333333333333703, 0.3269284268010768657, 0.3333333333333333703, 0.3269284268010768657, 0.3333333333333333703, 0.3269284268010768657, 0.3333333333333333703, 0.3269284268010768657, 0.3333333333333333703, 0.3269284268010768657, 0.3333333333333333703, 0.3269284268010768657, 0.3333333333333333703, 0.3269284268010768657, 0.3333333333333333703, 0.3269284268010768657, 0.3333333333333333703, 0.3269284268010768657, 0.3333333333333333703, 0.3269284268010768657, 0.3333333333333333703, 0.3269284268010768657, 0.3333333333333333703, 0.3269284268010768657, 0.3333333333333333703, 0.3269284268010768657, 0.3333333333333333703, 0.3269284268010768657, 0.3333333333333333703, 0.3269284268010768657, 0.3333333333333333703, 0.3269284268010768657, 0.3333333333333333703, 0.3269284268010768657, 0.3333333333333333703, 0.3269284268010768657, 0.3333333333333333703, 0.3269284268010768657, 0.3333333333333333703, 0.3269284268010768657, 0.3333333333333333703, 0.3269284268010768657, 0.3333333333333333703, 0.3269284268010768657, 0.3333333333333333703, 0.3269284268010768657, 0.3333333333333333703, 0.3269284268010768657, 0.3333333333333333703, 0.3269284268010768657, 0.3333333333333333703, 0.3269284268010768657, 0.3333333333333333703, 0.3269284268010768657, 0.3333333333333333703, 0.3269284268010768657, 0.3333333333333333703, 0.3269284268010768657, 0.3333333333333333703, 0.3269284268010768657, 0.3333333333333333703, 0.3269284268010768657, 0.3333333333333333703, 0.3269284268010768657, 0.3333333333333333703, 0.3269284268010768657, 0.3333333333333333703, 0.3269284268010768657, 0.3333333333333333703, 0.3269284268010768657, 0.3333333333333333703, 0.3269284268010768657, 0.3333333333333333703, 0.3269284268010768657, 0.3333333333333333703, 0.3269284268010768657, 0.3333333333333333703, 0.3269284268010768657, 0.3333333333333333703, 0.3269284268010768657, 0.3333333333333333703, 0.3269284268010768657, 0.3333333333333333703, 0.3269284268010768657, 0.3333333333333333703, 0.3269284268010768657, 0.3333333333333333703, 0.3269284268010768657, 0.3333333333333333703, 0.3269284268010768657, 0.3333333333333333703, 0.3269284268010768657, 0.3333333333333333703, 0.3269284268010768657, 0.3333333333333333703, 0.3269284268010768657, 0.3333333333333333703, 0.3269284268010768657, 0.3333333333333333703, 0.3269284268010768657, 0.3333333333333333703, 0.3269284268010768657, 0.3333333333333333703, 0.3269284268010768657, 0.3333333333333333703, 0.3269284268010768657, 0.3333333333333333703, 0.3269284268010768657, 0.3333333333333333703, 0.3269284268010768657, 0.3333333333333333703, 0.3269284268010768657, 0.3333333333333333703, 0.3269284268010768657, 0.3333333333333333703, 0.3269284268010768657, 0.3333333333333333703, 0.3269284268010768657, 0.3333333333333333703, 0.3269284268010768657, 0.3333333333333333703, 0.3269284268010768657, 0.3333333333333333703, 0.3269284268010768657, 0.3333333333333333703, 0.3269284268010768657, 0.3333333333333333703, 0.3269284268010768657, 0.3333333333333333703, 0.3269284268010768657, 0.3333333333333333703, 0.3269284268010768657, 0.3333333333333333703, 0.3269284268010768657, 0.3333333333333333703, 0.3269284268010768657, 0.3333333333333333703, 0.3269284268010768657, 0.3333333333333333703, 0.3269284268010768657, 0.3333333333333333703, 0.3269284268010768657, 0.3333333333333333703, 0.3269284268010768657, 0.3333333333333333703, 0.3269284268010768657, 0.3333333333333333703, 0.3269284268010768657, 0.3333333333333333703, 0.3269284268010768657, 0.3333333333333333703, 0.3269284268010768657, 0.3333333333333333703, 0.3269284268010768657, 0.3333333333333333703, 0.3269284268010768657, 0.3333333333333333703, 0.3269284268010768657, 0.3333333333333333703, 0.3269284268010768657, 0.3333333333333333703, 0.3269284268010768657, 0.3333333333333333703, 0.3269284268010768657, 0.3333333333333333703, 0.3269284268010768657, 0.3333333333333333703, 0.3269284268010768657, 0.3333333333333333703, 0.3269284268010768657, 0.3333333333333333703, 0.3269284268010768657, 0.3333333333333333703, 0.3269284268010768657, 0.3333333333333333703, 0.3269284268010768657, 0.3333333333333333703, 0.3269284268010768657, 0.3333333333333333703, 0.3269284268010768657, 0.3333333333333333703, 0.3269284268010768657, 0.3333333333333333703, 0.3269284268010768657, 0.3333333333333333703, 0.3269284268010768657, 0.3333333333333333703, 0.3269284268010768657, 0.3333333333333333703, 0.3269284268010768657, 0.3333333333333333703, 0.3269284268010768657, 0.3333333333333333703, 0.3269284268010768657, 0.3333333333333333703, 0.3269284268010768657, 0.3333333333333333703, 0.3269284268010768657, 0.3333333333333333703, 0.3269284268010768657, 0.3333333333333333703, 0.3269284268010768657, 0.3333333333333333703, 0.3269284268010768657, 0.3333333333333333703, 0.3269284268010768657, 0.3333333333333333703, 0.3269284268010768657, 0.3333333333333333703, 0.3269284268010768657, 0.3333333333333333703, 0.3269284268010768657, 0.3333333333333333703, 0.3269284268010768657, 0.3333333333333333703, 0.3269284268010768657, 0.3333333333333333703, 0.3269284268010768657, 0.3333333333333333703, 0.3269284268010768657, 0.3333333333333333703, 0.3269284268010768657, 0.3333333333333333703, 0.3269284268010768657, 0.3333333333333333703, 0.3269284268010768657, 0.3333333333333333703, 0.3269284268010768657, 0.3333333333333333703, 0.3269284268010768657, 0.3333333333333333703, 0.3269284268010768657, 0.3333333333333333703, 0.3269284268010768657, 0.3333333333333333703, 0.3269284268010768657, 0.3333333333333333703, 0.3269284268010768657, 0.3333333333333333703, 0.3269284268010768657, 0.3333333333333333703, 0.3269284268010768657, 0.3333333333333333703, 0.3269284268010768657, 0.3333333333333333703, 0.3269284268010768657, 0.3333333333333333703, 0.3269284268010768657, 0.3333333333333333703, 0.3269284268010768657, 0.3333333333333333703, 0.3269284268010768657, 0.3333333333333333703, 0.3269284268010768657, 0.3333333333333333703, 0.3269284268010768657, 0.3333333333333333703, 0.3269284268010768657, 0.3333333333333333703, 0.3269284268010768657, 0.3333333333333333703, 0.3269284268010768657, 0.3333333333333333703, 0.3269284268010768657, 0.3333333333333333703, 0.3269284268010768657, 0.3333333333333333703, 0.3269284268010768657, 0.3333333333333333703, 0.3269284268010768657, 0.3333333333333333703, 0.3269284268010768657, 0.3333333333333333703, 0.3269284268010768657, 0.3333333333333333703, 0.3269284268010768657, 0.3333333333333333703, 0.3269284268010768657, 0.3333333333333333703, 0.3269284268010768657, 0.3333333333333333703, 0.3269284268010768657, 0.3333333333333333703),
 ( 0.3333333333333333703, 0.3269284268010768657, 0.3333333333333333703, 0.3269284268010768657, 0.3333333333333333703, 0.3269284268010768657, 0.3333333333333333703, 0.3269284268010768657, 0.3333333333333333703, 0.3269284268010768657, 0.3333333333333333703, 0.3269284268010768657, 0.3333333333333333703, 0.3269284268010768657, 0.3333333333333333703, 0.3269284268010768657, 0.3333333333333333703, 0.3269284268010768657, 0.3333333333333333703, 0.3269284268010768657, 0.3333333333333333703, 0.3269284268010768657, 0.3333333333333333703, 0.3269284268010768657, 0.3333333333333333703, 0.3269284268010768657, 0.3333333333333333703, 0.3269284268010768657, 0.3333333333333333703, 0.3269284268010768657, 0.3333333333333333703, 0.3269284268010768657, 0.3333333333333333703, 0.3269284268010768657, 0.3333333333333333703, 0.3269284268010768657, 0.3333333333333333703, 0.3269284268010768657, 0.3333333333333333703, 0.3269284268010768657, 0.3333333333333333703, 0.3269284268010768657, 0.3333333333333333703, 0.3269284268010768657, 0.3333333333333333703, 0.3269284268010768657, 0.3333333333333333703, 0.3269284268010768657, 0.3333333333333333703, 0.3269284268010768657, 0.3333333333333333703, 0.3269284268010768657, 0.3333333333333333703, 0.3269284268010768657, 0.3333333333333333703, 0.3269284268010768657, 0.3333333333333333703, 0.3269284268010768657, 0.3333333333333333703, 0.3269284268010768657, 0.3333333333333333703, 0.3269284268010768657, 0.3333333333333333703, 0.3269284268010768657, 0.3333333333333333703, 0.3269284268010768657, 0.3333333333333333703, 0.3269284268010768657, 0.3333333333333333703, 0.3269284268010768657, 0.3333333333333333703, 0.3269284268010768657, 0.3333333333333333703, 0.3269284268010768657, 0.3333333333333333703, 0.3269284268010768657, 0.3333333333333333703, 0.3269284268010768657, 0.3333333333333333703, 0.3269284268010768657, 0.3333333333333333703, 0.3269284268010768657, 0.3333333333333333703, 0.3269284268010768657, 0.3333333333333333703, 0.3269284268010768657, 0.3333333333333333703, 0.3269284268010768657, 0.3333333333333333703, 0.3269284268010768657, 0.3333333333333333703, 0.3269284268010768657, 0.3333333333333333703, 0.3269284268010768657, 0.3333333333333333703, 0.3269284268010768657, 0.3333333333333333703, 0.3269284268010768657, 0.3333333333333333703, 0.3269284268010768657, 0.3333333333333333703, 0.3269284268010768657, 0.3333333333333333703, 0.3269284268010768657, 0.3333333333333333703, 0.3269284268010768657, 0.3333333333333333703, 0.3269284268010768657, 0.3333333333333333703, 0.3269284268010768657, 0.3333333333333333703, 0.3269284268010768657, 0.3333333333333333703, 0.3269284268010768657, 0.3333333333333333703, 0.3269284268010768657, 0.3333333333333333703, 0.3269284268010768657, 0.3333333333333333703, 0.3269284268010768657, 0.3333333333333333703, 0.3269284268010768657, 0.3333333333333333703, 0.3269284268010768657, 0.3333333333333333703, 0.3269284268010768657, 0.3333333333333333703, 0.3269284268010768657, 0.3333333333333333703, 0.3269284268010768657, 0.3333333333333333703, 0.3269284268010768657, 0.3333333333333333703, 0.3269284268010768657, 0.3333333333333333703, 0.3269284268010768657, 0.3333333333333333703, 0.3269284268010768657, 0.3333333333333333703, 0.3269284268010768657, 0.3333333333333333703, 0.3269284268010768657, 0.3333333333333333703, 0.3269284268010768657, 0.3333333333333333703, 0.3269284268010768657, 0.3333333333333333703, 0.3269284268010768657, 0.3333333333333333703, 0.3269284268010768657, 0.3333333333333333703, 0.3269284268010768657, 0.3333333333333333703, 0.3269284268010768657, 0.3333333333333333703, 0.3269284268010768657, 0.3333333333333333703, 0.3269284268010768657, 0.3333333333333333703, 0.3269284268010768657, 0.3333333333333333703, 0.3269284268010768657, 0.3333333333333333703, 0.3269284268010768657, 0.3333333333333333703, 0.3269284268010768657, 0.3333333333333333703, 0.3269284268010768657, 0.3333333333333333703, 0.3269284268010768657, 0.3333333333333333703, 0.3269284268010768657, 0.3333333333333333703, 0.3269284268010768657, 0.3333333333333333703, 0.3269284268010768657, 0.3333333333333333703, 0.3269284268010768657, 0.3333333333333333703, 0.3269284268010768657, 0.3333333333333333703, 0.3269284268010768657, 0.3333333333333333703, 0.3269284268010768657, 0.3333333333333333703, 0.3269284268010768657, 0.3333333333333333703, 0.3269284268010768657, 0.3333333333333333703, 0.3269284268010768657, 0.3333333333333333703, 0.3269284268010768657, 0.3333333333333333703, 0.3269284268010768657, 0.3333333333333333703, 0.3269284268010768657, 0.3333333333333333703, 0.3269284268010768657, 0.3333333333333333703, 0.3269284268010768657, 0.3333333333333333703, 0.3269284268010768657, 0.3333333333333333703, 0.3269284268010768657, 0.3333333333333333703, 0.3269284268010768657, 0.3333333333333333703, 0.3269284268010768657, 0.3333333333333333703, 0.3269284268010768657, 0.3333333333333333703, 0.3269284268010768657, 0.3333333333333333703, 0.3269284268010768657, 0.3333333333333333703, 0.3269284268010768657, 0.3333333333333333703, 0.3269284268010768657, 0.3333333333333333703, 0.3269284268010768657, 0.3333333333333333703, 0.3269284268010768657, 0.3333333333333333703, 0.3269284268010768657, 0.3333333333333333703, 0.3269284268010768657, 0.3333333333333333703, 0.3269284268010768657, 0.3333333333333333703, 0.3269284268010768657, 0.3333333333333333703, 0.3269284268010768657, 0.3333333333333333703, 0.3269284268010768657, 0.3333333333333333703, 0.3269284268010768657, 0.3333333333333333703, 0.3269284268010768657, 0.3333333333333333703, 0.3269284268010768657, 0.3333333333333333703, 0.3269284268010768657, 0.3333333333333333703, 0.3269284268010768657, 0.3333333333333333703, 0.3269284268010768657, 0.3333333333333333703, 0.3269284268010768657, 0.3333333333333333703, 0.3269284268010768657, 0.3333333333333333703, 0.3269284268010768657, 0.3333333333333333703, 0.3269284268010768657, 0.3333333333333333703, 0.3269284268010768657, 0.3333333333333333703, 0.3269284268010768657, 0.3333333333333333703, 0.3269284268010768657, 0.3333333333333333703, 0.3269284268010768657, 0.3333333333333333703, 0.3269284268010768657, 0.3333333333333333703, 0.3269284268010768657, 0.3333333333333333703, 0.3269284268010768657, 0.3333333333333333703, 0.3269284268010768657, 0.3333333333333333703, 0.3269284268010768657, 0.3333333333333333703, 0.3269284268010768657, 0.3333333333333333703, 0.3269284268010768657, 0.3333333333333333703, 0.3269284268010768657, 0.3333333333333333703, 0.3269284268010768657, 0.3333333333333333703, 0.3269284268010768657, 0.3333333333333333703, 0.3269284268010768657, 0.3333333333333333703, 0.3269284268010768657, 0.3333333333333333703, 0.3269284268010768657, 0.3333333333333333703, 0.3269284268010768657, 0.3333333333333333703, 0.3269284268010768657, 0.3333333333333333703, 0.3269284268010768657, 0.3333333333333333703, 0.3269284268010768657, 0.3333333333333333703, 0.3269284268010768657, 0.3333333333333333703, 0.3269284268010768657, 0.3333333333333333703, 0.3269284268010768657, 0.3333333333333333703, 0.3269284268010768657, 0.3333333333333333703, 0.3269284268010768657, 0.3333333333333333703, 0.3269284268010768657, 0.3333333333333333703, 0.3269284268010768657, 0.3333333333333333703, 0.3269284268010768657, 0.3333333333333333703, 0.3269284268010768657, 0.3333333333333333703, 0.3269284268010768657, 0.3333333333333333703, 0.3269284268010768657, 0.3333333333333333703, 0.3269284268010768657, 0.3333333333333333703, 0.3269284268010768657, 0.3333333333333333703, 0.3269284268010768657, 0.3333333333333333703, 0.3269284268010768657, 0.3333333333333333703, 0.3269284268010768657, 0.3333333333333333703, 0.3269284268010768657, 0.3333333333333333703, 0.3269284268010768657, 0.3333333333333333703, 0.3269284268010768657, 0.3333333333333333703, 0.3269284268010768657, 0.3333333333333333703, 0.3269284268010768657, 0.3333333333333333703, 0.3269284268010768657, 0.3333333333333333703, 0.3269284268010768657, 0.3333333333333333703, 0.3269284268010768657, 0.3333333333333333703, 0.3269284268010768657, 0.3333333333333333703, 0.3269284268010768657, 0.3333333333333333703, 0.3269284268010768657, 0.3333333333333333703, 0.3269284268010768657, 0.3333333333333333703, 0.3269284268010768657, 0.3333333333333333703, 0.3269284268010768657, 0.3333333333333333703, 0.3269284268010768657, 0.3333333333333333703, 0.3269284268010768657, 0.3333333333333333703, 0.3269284268010768657, 0.3333333333333333703, 0.3269284268010768657, 0.3333333333333333703, 0.3269284268010768657, 0.3333333333333333703, 0.3269284268010768657, 0.3333333333333333703, 0.3269284268010768657, 0.3333333333333333703, 0.3269284268010768657, 0.3333333333333333703, 0.3269284268010768657, 0.3333333333333333703, 0.3269284268010768657, 0.3333333333333333703, 0.3269284268010768657, 0.3333333333333333703, 0.3269284268010768657, 0.3333333333333333703, 0.3269284268010768657, 0.3333333333333333703, 0.3269284268010768657, 0.3333333333333333703, 0.3269284268010768657, 0.3333333333333333703, 0.3269284268010768657, 0.3333333333333333703, 0.3269284268010768657, 0.3333333333333333703, 0.3269284268010768657, 0.3333333333333333703, 0.3269284268010768657, 0.3333333333333333703, 0.3269284268010768657, 0.3333333333333333703, 0.3269284268010768657, 0.3333333333333333703, 0.3269284268010768657, 0.3333333333333333703, 0.3269284268010768657, 0.3333333333333333703, 0.3269284268010768657, 0.3333333333333333703, 0.3269284268010768657, 0.3333333333333333703, 0.3269284268010768657, 0.3333333333333333703, 0.3269284268010768657, 0.3333333333333333703, 0.3269284268010768657, 0.3333333333333333703, 0.3269284268010768657, 0.3333333333333333703, 0.3269284268010768657, 0.3333333333333333703, 0.3269284268010768657, 0.3333333333333333703, 0.3269284268010768657, 0.3333333333333333703, 0.3269284268010768657, 0.3333333333333333703, 0.3269284268010768657, 0.3333333333333333703, 0.3269284268010768657, 0.3333333333333333703, 0.3269284268010768657, 0.3333333333333333703, 0.3269284268010768657, 0.3333333333333333703, 0.3269284268010768657, 0.3333333333333333703, 0.3269284268010768657, 0.3333333333333333703, 0.3269284268010768657, 0.3333333333333333703, 0.3269284268010768657, 0.3333333333333333703, 0.3269284268010768657, 0.3333333333333333703, 0.3269284268010768657, 0.3333333333333333703, 0.3269284268010768657, 0.3333333333333333703, 0.3269284268010768657, 0.3333333333333333703, 0.3269284268010768657, 0.3333333333333333703, 0.3269284268010768657, 0.3333333333333333703, 0.3269284268010768657, 0.3333333333333333703, 0.3269284268010768657, 0.3333333333333333703, 0.3269284268010768657, 0.3333333333333333703, 0.3269284268010768657, 0.3333333333333333703, 0.3269284268010768657, 0.3333333333333333703, 0.3269284268010768657, 0.3333333333333333703, 0.3269284268010768657, 0.3333333333333333703, 0.3269284268010768657, 0.3333333333333333703, 0.3269284268010768657, 0.3333333333333333703, 0.3269284268010768657, 0.3333333333333333703, 0.3269284268010768657, 0.3333333333333333703, 0.3269284268010768657, 0.3333333333333333703, 0.3269284268010768657, 0.3333333333333333703, 0.3269284268010768657, 0.3333333333333333703, 0.3269284268010768657, 0.3333333333333333703),
 ( 1.000000000000000000, 0.9807852804032304306, 1.000000000000000000, 0.9807852804032304306, 1.000000000000000000, 0.9807852804032304306, 1.000000000000000000, 0.9807852804032304306, 1.000000000000000000, 0.9807852804032304306, 1.000000000000000000, 0.9807852804032304306, 1.000000000000000000, 0.9807852804032304306, 1.000000000000000000, 0.9807852804032304306, 1.000000000000000000, 0.9807852804032304306, 1.000000000000000000, 0.9807852804032304306, 1.000000000000000000, 0.9807852804032304306, 1.000000000000000000, 0.9807852804032304306, 1.000000000000000000, 0.9807852804032304306, 1.000000000000000000, 0.9807852804032304306, 1.000000000000000000, 0.9807852804032304306, 1.000000000000000000, 0.9807852804032304306, 1.000000000000000000, 0.9807852804032304306, 1.000000000000000000, 0.9807852804032304306, 1.000000000000000000, 0.9807852804032304306, 1.000000000000000000, 0.9807852804032304306, 1.000000000000000000, 0.9807852804032304306, 1.000000000000000000, 0.9807852804032304306, 1.000000000000000000, 0.9807852804032304306, 1.000000000000000000, 0.9807852804032304306, 1.000000000000000000, 0.9807852804032304306, 1.000000000000000000, 0.9807852804032304306, 1.000000000000000000, 0.9807852804032304306, 1.000000000000000000, 0.9807852804032304306, 1.000000000000000000, 0.9807852804032304306, 1.000000000000000000, 0.9807852804032304306, 1.000000000000000000, 0.9807852804032304306, 1.000000000000000000, 0.9807852804032304306, 1.000000000000000000, 0.9807852804032304306, 1.000000000000000000, 0.9807852804032304306, 1.000000000000000000, 0.9807852804032304306, 1.000000000000000000, 0.9807852804032304306, 1.000000000000000000, 0.9807852804032304306, 1.000000000000000000, 0.9807852804032304306, 1.000000000000000000, 0.9807852804032304306, 1.000000000000000000, 0.9807852804032304306, 1.000000000000000000, 0.9807852804032304306, 1.000000000000000000, 0.9807852804032304306, 1.000000000000000000, 0.9807852804032304306, 1.000000000000000000, 0.9807852804032304306, 1.000000000000000000, 0.9807852804032304306, 1.000000000000000000, 0.9807852804032304306, 1.000000000000000000, 0.9807852804032304306, 1.000000000000000000, 0.9807852804032304306, 1.000000000000000000, 0.9807852804032304306, 1.000000000000000000, 0.9807852804032304306, 1.000000000000000000, 0.9807852804032304306, 1.000000000000000000, 0.9807852804032304306, 1.000000000000000000, 0.9807852804032304306, 1.000000000000000000, 0.9807852804032304306, 1.000000000000000000, 0.9807852804032304306, 1.000000000000000000, 0.9807852804032304306, 1.000000000000000000, 0.9807852804032304306, 1.000000000000000000, 0.9807852804032304306, 1.000000000000000000, 0.9807852804032304306, 1.000000000000000000, 0.9807852804032304306, 1.000000000000000000, 0.9807852804032304306, 1.000000000000000000, 0.9807852804032304306, 1.000000000000000000, 0.9807852804032304306, 1.000000000000000000, 0.9807852804032304306, 1.000000000000000000, 0.9807852804032304306, 1.000000000000000000, 0.9807852804032304306, 1.000000000000000000, 0.9807852804032304306, 1.000000000000000000, 0.9807852804032304306, 1.000000000000000000, 0.9807852804032304306, 1.000000000000000000, 0.9807852804032304306, 1.000000000000000000, 0.9807852804032304306, 1.000000000000000000, 0.9807852804032304306, 1.000000000000000000, 0.9807852804032304306, 1.000000000000000000, 0.9807852804032304306, 1.000000000000000000, 0.9807852804032304306, 1.000000000000000000, 0.9807852804032304306, 1.000000000000000000, 0.9807852804032304306, 1.000000000000000000, 0.9807852804032304306, 1.000000000000000000, 0.9807852804032304306, 1.000000000000000000, 0.9807852804032304306, 1.000000000000000000, 0.9807852804032304306, 1.000000000000000000, 0.9807852804032304306, 1.000000000000000000, 0.9807852804032304306, 1.000000000000000000, 0.9807852804032304306, 1.000000000000000000, 0.9807852804032304306, 1.000000000000000000, 0.9807852804032304306, 1.000000000000000000, 0.9807852804032304306, 1.000000000000000000, 0.9807852804032304306, 1.000000000000000000, 0.9807852804032304306, 1.000000000000000000, 0.9807852804032304306, 1.000000000000000000, 0.9807852804032304306, 1.000000000000000000, 0.9807852804032304306, 1.000000000000000000, 0.9807852804032304306, 1.000000000000000000, 0.9807852804032304306, 1.000000000000000000, 0.9807852804032304306, 1.000000000000000000, 0.9807852804032304306, 1.000000000000000000, 0.9807852804032304306, 1.000000000000000000, 0.9807852804032304306, 1.000000000000000000, 0.9807852804032304306, 1.000000000000000000, 0.9807852804032304306, 1.000000000000000000, 0.9807852804032304306, 1.000000000000000000, 0.9807852804032304306, 1.000000000000000000, 0.9807852804032304306, 1.000000000000000000, 0.9807852804032304306, 1.000000000000000000, 0.9807852804032304306, 1.000000000000000000, 0.9807852804032304306, 1.000000000000000000, 0.9807852804032304306, 1.000000000000000000, 0.9807852804032304306, 1.000000000000000000, 0.9807852804032304306, 1.000000000000000000, 0.9807852804032304306, 1.000000000000000000, 0.9807852804032304306, 1.000000000000000000, 0.9807852804032304306, 1.000000000000000000, 0.9807852804032304306, 1.000000000000000000, 0.9807852804032304306, 1.000000000000000000, 0.9807852804032304306, 1.000000000000000000, 0.9807852804032304306, 1.000000000000000000, 0.9807852804032304306, 1.000000000000000000, 0.9807852804032304306, 1.000000000000000000, 0.9807852804032304306, 1.000000000000000000, 0.9807852804032304306, 1.000000000000000000, 0.9807852804032304306, 1.000000000000000000, 0.9807852804032304306, 1.000000000000000000, 0.9807852804032304306, 1.000000000000000000, 0.9807852804032304306, 1.000000000000000000, 0.9807852804032304306, 1.000000000000000000, 0.9807852804032304306, 1.000000000000000000, 0.9807852804032304306, 1.000000000000000000, 0.9807852804032304306, 1.000000000000000000, 0.9807852804032304306, 1.000000000000000000, 0.9807852804032304306, 1.000000000000000000, 0.9807852804032304306, 1.000000000000000000, 0.9807852804032304306, 1.000000000000000000, 0.9807852804032304306, 1.000000000000000000, 0.9807852804032304306, 1.000000000000000000, 0.9807852804032304306, 1.000000000000000000, 0.9807852804032304306, 1.000000000000000000, 0.9807852804032304306, 1.000000000000000000, 0.9807852804032304306, 1.000000000000000000, 0.9807852804032304306, 1.000000000000000000, 0.9807852804032304306, 1.000000000000000000, 0.9807852804032304306, 1.000000000000000000, 0.9807852804032304306, 1.000000000000000000, 0.9807852804032304306, 1.000000000000000000, 0.9807852804032304306, 1.000000000000000000, 0.9807852804032304306, 1.000000000000000000, 0.9807852804032304306, 1.000000000000000000, 0.9807852804032304306, 1.000000000000000000, 0.9807852804032304306, 1.000000000000000000, 0.9807852804032304306, 1.000000000000000000, 0.9807852804032304306, 1.000000000000000000, 0.9807852804032304306, 1.000000000000000000, 0.9807852804032304306, 1.000000000000000000, 0.9807852804032304306, 1.000000000000000000, 0.9807852804032304306, 1.000000000000000000, 0.9807852804032304306, 1.000000000000000000, 0.9807852804032304306, 1.000000000000000000, 0.9807852804032304306, 1.000000000000000000, 0.9807852804032304306, 1.000000000000000000, 0.9807852804032304306, 1.000000000000000000, 0.9807852804032304306, 1.000000000000000000, 0.9807852804032304306, 1.000000000000000000, 0.9807852804032304306, 1.000000000000000000, 0.9807852804032304306, 1.000000000000000000, 0.9807852804032304306, 1.000000000000000000, 0.9807852804032304306, 1.000000000000000000, 0.9807852804032304306, 1.000000000000000000, 0.9807852804032304306, 1.000000000000000000, 0.9807852804032304306, 1.000000000000000000, 0.9807852804032304306, 1.000000000000000000, 0.9807852804032304306, 1.000000000000000000, 0.9807852804032304306, 1.000000000000000000, 0.9807852804032304306, 1.000000000000000000, 0.9807852804032304306, 1.000000000000000000, 0.9807852804032304306, 1.000000000000000000, 0.9807852804032304306, 1.000000000000000000, 0.9807852804032304306, 1.000000000000000000, 0.9807852804032304306, 1.000000000000000000, 0.9807852804032304306, 1.000000000000000000, 0.9807852804032304306, 1.000000000000000000, 0.9807852804032304306, 1.000000000000000000, 0.9807852804032304306, 1.000000000000000000, 0.9807852804032304306, 1.000000000000000000, 0.9807852804032304306, 1.000000000000000000, 0.9807852804032304306, 1.000000000000000000, 0.9807852804032304306, 1.000000000000000000, 0.9807852804032304306, 1.000000000000000000, 0.9807852804032304306, 1.000000000000000000, 0.9807852804032304306, 1.000000000000000000, 0.9807852804032304306, 1.000000000000000000, 0.9807852804032304306, 1.000000000000000000, 0.9807852804032304306, 1.000000000000000000, 0.9807852804032304306, 1.000000000000000000, 0.9807852804032304306, 1.000000000000000000, 0.9807852804032304306, 1.000000000000000000, 0.9807852804032304306, 1.000000000000000000, 0.9807852804032304306, 1.000000000000000000, 0.9807852804032304306, 1.000000000000000000, 0.9807852804032304306, 1.000000000000000000, 0.9807852804032304306, 1.000000000000000000, 0.9807852804032304306, 1.000000000000000000, 0.9807852804032304306, 1.000000000000000000, 0.9807852804032304306, 1.000000000000000000, 0.9807852804032304306, 1.000000000000000000, 0.9807852804032304306, 1.000000000000000000, 0.9807852804032304306, 1.000000000000000000, 0.9807852804032304306, 1.000000000000000000, 0.9807852804032304306, 1.000000000000000000, 0.9807852804032304306, 1.000000000000000000, 0.9807852804032304306, 1.000000000000000000, 0.9807852804032304306, 1.000000000000000000, 0.9807852804032304306, 1.000000000000000000, 0.9807852804032304306, 1.000000000000000000, 0.9807852804032304306, 1.000000000000000000, 0.9807852804032304306, 1.000000000000000000, 0.9807852804032304306, 1.000000000000000000, 0.9807852804032304306, 1.000000000000000000, 0.9807852804032304306, 1.000000000000000000, 0.9807852804032304306, 1.000000000000000000, 0.9807852804032304306, 1.000000000000000000, 0.9807852804032304306, 1.000000000000000000, 0.9807852804032304306, 1.000000000000000000, 0.9807852804032304306, 1.000000000000000000, 0.9807852804032304306, 1.000000000000000000, 0.9807852804032304306, 1.000000000000000000, 0.9807852804032304306, 1.000000000000000000, 0.9807852804032304306, 1.000000000000000000, 0.9807852804032304306, 1.000000000000000000, 0.9807852804032304306, 1.000000000000000000, 0.9807852804032304306, 1.000000000000000000, 0.9807852804032304306, 1.000000000000000000, 0.9807852804032304306, 1.000000000000000000, 0.9807852804032304306, 1.000000000000000000, 0.9807852804032304306, 1.000000000000000000, 0.9807852804032304306, 1.000000000000000000, 0.9807852804032304306, 1.000000000000000000, 0.9807852804032304306, 1.000000000000000000, 0.9807852804032304306, 1.000000000000000000, 0.9807852804032304306, 1.000000000000000000, 0.9807852804032304306, 1.000000000000000000, 0.9807852804032304306, 1.000000000000000000),
 ( 0.3333333333333333703, 0.3269284268010768657, 0.3333333333333333703, 0.3269284268010768657, 0.3333333333333333703, 0.3269284268010768657, 0.3333333333333333703, 0.3269284268010768657, 0.3333333333333333703, 0.3269284268010768657, 0.3333333333333333703, 0.3269284268010768657, 0.3333333333333333703, 0.3269284268010768657, 0.3333333333333333703, 0.3269284268010768657, 0.3333333333333333703, 0.3269284268010768657, 0.3333333333333333703, 0.3269284268010768657, 0.3333333333333333703, 0.3269284268010768657, 0.3333333333333333703, 0.3269284268010768657, 0.3333333333333333703, 0.3269284268010768657, 0.3333333333333333703, 0.3269284268010768657, 0.3333333333333333703, 0.3269284268010768657, 0.3333333333333333703, 0.3269284268010768657, 0.3333333333333333703, 0.3269284268010768657, 0.3333333333333333703, 0.3269284268010768657, 0.3333333333333333703, 0.3269284268010768657, 0.3333333333333333703, 0.3269284268010768657, 0.3333333333333333703, 0.3269284268010768657, 0.3333333333333333703, 0.3269284268010768657, 0.3333333333333333703, 0.3269284268010768657, 0.3333333333333333703, 0.3269284268010768657, 0.3333333333333333703, 0.3269284268010768657, 0.3333333333333333703, 0.3269284268010768657, 0.3333333333333333703, 0.3269284268010768657, 0.3333333333333333703, 0.3269284268010768657, 0.3333333333333333703, 0.3269284268010768657, 0.3333333333333333703, 0.3269284268010768657, 0.3333333333333333703, 0.3269284268010768657, 0.3333333333333333703, 0.3269284268010768657, 0.3333333333333333703, 0.3269284268010768657, 0.3333333333333333703, 0.3269284268010768657, 0.3333333333333333703, 0.3269284268010768657, 0.3333333333333333703, 0.3269284268010768657, 0.3333333333333333703, 0.3269284268010768657, 0.3333333333333333703, 0.3269284268010768657, 0.3333333333333333703, 0.3269284268010768657, 0.3333333333333333703, 0.3269284268010768657, 0.3333333333333333703, 0.3269284268010768657, 0.3333333333333333703, 0.3269284268010768657, 0.3333333333333333703, 0.3269284268010768657, 0.3333333333333333703, 0.3269284268010768657, 0.3333333333333333703, 0.3269284268010768657, 0.3333333333333333703, 0.3269284268010768657, 0.3333333333333333703, 0.3269284268010768657, 0.3333333333333333703, 0.3269284268010768657, 0.3333333333333333703, 0.3269284268010768657, 0.3333333333333333703, 0.3269284268010768657, 0.3333333333333333703, 0.3269284268010768657, 0.3333333333333333703, 0.3269284268010768657, 0.3333333333333333703, 0.3269284268010768657, 0.3333333333333333703, 0.3269284268010768657, 0.3333333333333333703, 0.3269284268010768657, 0.3333333333333333703, 0.3269284268010768657, 0.3333333333333333703, 0.3269284268010768657, 0.3333333333333333703, 0.3269284268010768657, 0.3333333333333333703, 0.3269284268010768657, 0.3333333333333333703, 0.3269284268010768657, 0.3333333333333333703, 0.3269284268010768657, 0.3333333333333333703, 0.3269284268010768657, 0.3333333333333333703, 0.3269284268010768657, 0.3333333333333333703, 0.3269284268010768657, 0.3333333333333333703, 0.3269284268010768657, 0.3333333333333333703, 0.3269284268010768657, 0.3333333333333333703, 0.3269284268010768657, 0.3333333333333333703, 0.3269284268010768657, 0.3333333333333333703, 0.3269284268010768657, 0.3333333333333333703, 0.3269284268010768657, 0.3333333333333333703, 0.3269284268010768657, 0.3333333333333333703, 0.3269284268010768657, 0.3333333333333333703, 0.3269284268010768657, 0.3333333333333333703, 0.3269284268010768657, 0.3333333333333333703, 0.3269284268010768657, 0.3333333333333333703, 0.3269284268010768657, 0.3333333333333333703, 0.3269284268010768657, 0.3333333333333333703, 0.3269284268010768657, 0.3333333333333333703, 0.3269284268010768657, 0.3333333333333333703, 0.3269284268010768657, 0.3333333333333333703, 0.3269284268010768657, 0.3333333333333333703, 0.3269284268010768657, 0.3333333333333333703, 0.3269284268010768657, 0.3333333333333333703, 0.3269284268010768657, 0.3333333333333333703, 0.3269284268010768657, 0.3333333333333333703, 0.3269284268010768657, 0.3333333333333333703, 0.3269284268010768657, 0.3333333333333333703, 0.3269284268010768657, 0.3333333333333333703, 0.3269284268010768657, 0.3333333333333333703, 0.3269284268010768657, 0.3333333333333333703, 0.3269284268010768657, 0.3333333333333333703, 0.3269284268010768657, 0.3333333333333333703, 0.3269284268010768657, 0.3333333333333333703, 0.3269284268010768657, 0.3333333333333333703, 0.3269284268010768657, 0.3333333333333333703, 0.3269284268010768657, 0.3333333333333333703, 0.3269284268010768657, 0.3333333333333333703, 0.3269284268010768657, 0.3333333333333333703, 0.3269284268010768657, 0.3333333333333333703, 0.3269284268010768657, 0.3333333333333333703, 0.3269284268010768657, 0.3333333333333333703, 0.3269284268010768657, 0.3333333333333333703, 0.3269284268010768657, 0.3333333333333333703, 0.3269284268010768657, 0.3333333333333333703, 0.3269284268010768657, 0.3333333333333333703, 0.3269284268010768657, 0.3333333333333333703, 0.3269284268010768657, 0.3333333333333333703, 0.3269284268010768657, 0.3333333333333333703, 0.3269284268010768657, 0.3333333333333333703, 0.3269284268010768657, 0.3333333333333333703, 0.3269284268010768657, 0.3333333333333333703, 0.3269284268010768657, 0.3333333333333333703, 0.3269284268010768657, 0.3333333333333333703, 0.3269284268010768657, 0.3333333333333333703, 0.3269284268010768657, 0.3333333333333333703, 0.3269284268010768657, 0.3333333333333333703, 0.3269284268010768657, 0.3333333333333333703, 0.3269284268010768657, 0.3333333333333333703, 0.3269284268010768657, 0.3333333333333333703, 0.3269284268010768657, 0.3333333333333333703, 0.3269284268010768657, 0.3333333333333333703, 0.3269284268010768657, 0.3333333333333333703, 0.3269284268010768657, 0.3333333333333333703, 0.3269284268010768657, 0.3333333333333333703, 0.3269284268010768657, 0.3333333333333333703, 0.3269284268010768657, 0.3333333333333333703, 0.3269284268010768657, 0.3333333333333333703, 0.3269284268010768657, 0.3333333333333333703, 0.3269284268010768657, 0.3333333333333333703, 0.3269284268010768657, 0.3333333333333333703, 0.3269284268010768657, 0.3333333333333333703, 0.3269284268010768657, 0.3333333333333333703, 0.3269284268010768657, 0.3333333333333333703, 0.3269284268010768657, 0.3333333333333333703, 0.3269284268010768657, 0.3333333333333333703, 0.3269284268010768657, 0.3333333333333333703, 0.3269284268010768657, 0.3333333333333333703, 0.3269284268010768657, 0.3333333333333333703, 0.3269284268010768657, 0.3333333333333333703, 0.3269284268010768657, 0.3333333333333333703, 0.3269284268010768657, 0.3333333333333333703, 0.3269284268010768657, 0.3333333333333333703, 0.3269284268010768657, 0.3333333333333333703, 0.3269284268010768657, 0.3333333333333333703, 0.3269284268010768657, 0.3333333333333333703, 0.3269284268010768657, 0.3333333333333333703, 0.3269284268010768657, 0.3333333333333333703, 0.3269284268010768657, 0.3333333333333333703, 0.3269284268010768657, 0.3333333333333333703, 0.3269284268010768657, 0.3333333333333333703, 0.3269284268010768657, 0.3333333333333333703, 0.3269284268010768657, 0.3333333333333333703, 0.3269284268010768657, 0.3333333333333333703, 0.3269284268010768657, 0.3333333333333333703, 0.3269284268010768657, 0.3333333333333333703, 0.3269284268010768657, 0.3333333333333333703, 0.3269284268010768657, 0.3333333333333333703, 0.3269284268010768657, 0.3333333333333333703, 0.3269284268010768657, 0.3333333333333333703, 0.3269284268010768657, 0.3333333333333333703, 0.3269284268010768657, 0.3333333333333333703, 0.3269284268010768657, 0.3333333333333333703, 0.3269284268010768657, 0.3333333333333333703, 0.3269284268010768657, 0.3333333333333333703, 0.3269284268010768657, 0.3333333333333333703, 0.3269284268010768657, 0.3333333333333333703, 0.3269284268010768657, 0.3333333333333333703, 0.3269284268010768657, 0.3333333333333333703, 0.3269284268010768657, 0.3333333333333333703, 0.3269284268010768657, 0.3333333333333333703, 0.3269284268010768657, 0.3333333333333333703, 0.3269284268010768657, 0.3333333333333333703, 0.3269284268010768657, 0.3333333333333333703, 0.3269284268010768657, 0.3333333333333333703, 0.3269284268010768657, 0.3333333333333333703, 0.3269284268010768657, 0.3333333333333333703, 0.3269284268010768657, 0.3333333333333333703, 0.3269284268010768657, 0.3333333333333333703, 0.3269284268010768657, 0.3333333333333333703, 0.3269284268010768657, 0.3333333333333333703, 0.3269284268010768657, 0.3333333333333333703, 0.3269284268010768657, 0.3333333333333333703, 0.3269284268010768657, 0.3333333333333333703, 0.3269284268010768657, 0.3333333333333333703, 0.3269284268010768657, 0.3333333333333333703, 0.3269284268010768657, 0.3333333333333333703, 0.3269284268010768657, 0.3333333333333333703, 0.3269284268010768657, 0.3333333333333333703, 0.3269284268010768657, 0.3333333333333333703, 0.3269284268010768657, 0.3333333333333333703, 0.3269284268010768657, 0.3333333333333333703, 0.3269284268010768657, 0.3333333333333333703, 0.3269284268010768657, 0.3333333333333333703, 0.3269284268010768657, 0.3333333333333333703, 0.3269284268010768657, 0.3333333333333333703, 0.3269284268010768657, 0.3333333333333333703, 0.3269284268010768657, 0.3333333333333333703, 0.3269284268010768657, 0.3333333333333333703, 0.3269284268010768657, 0.3333333333333333703, 0.3269284268010768657, 0.3333333333333333703, 0.3269284268010768657, 0.3333333333333333703, 0.3269284268010768657, 0.3333333333333333703, 0.3269284268010768657, 0.3333333333333333703, 0.3269284268010768657, 0.3333333333333333703, 0.3269284268010768657, 0.3333333333333333703, 0.3269284268010768657, 0.3333333333333333703, 0.3269284268010768657, 0.3333333333333333703, 0.3269284268010768657, 0.3333333333333333703, 0.3269284268010768657, 0.3333333333333333703, 0.3269284268010768657, 0.3333333333333333703, 0.3269284268010768657, 0.3333333333333333703, 0.3269284268010768657, 0.3333333333333333703, 0.3269284268010768657, 0.3333333333333333703, 0.3269284268010768657, 0.3333333333333333703, 0.3269284268010768657, 0.3333333333333333703, 0.3269284268010768657, 0.3333333333333333703, 0.3269284268010768657, 0.3333333333333333703, 0.3269284268010768657, 0.3333333333333333703, 0.3269284268010768657, 0.3333333333333333703, 0.3269284268010768657, 0.3333333333333333703, 0.3269284268010768657, 0.3333333333333333703, 0.3269284268010768657, 0.3333333333333333703, 0.3269284268010768657, 0.3333333333333333703, 0.3269284268010768657, 0.3333333333333333703, 0.3269284268010768657, 0.3333333333333333703, 0.3269284268010768657, 0.3333333333333333703, 0.3269284268010768657, 0.3333333333333333703, 0.3269284268010768657, 0.3333333333333333703, 0.3269284268010768657, 0.3333333333333333703, 0.3269284268010768657, 0.3333333333333333703, 0.3269284268010768657, 0.3333333333333333703, 0.3269284268010768657, 0.3333333333333333703, 0.3269284268010768657, 0.3333333333333333703, 0.3269284268010768657, 0.3333333333333333703, 0.3269284268010768657, 0.3333333333333333703, 0.3269284268010768657, 0.3333333333333333703, 0.3269284268010768657, 0.3333333333333333703, 0.3269284268010768657, 0.3333333333333333703, 0.3269284268010768657, 0.3333333333333333703, 0.3269284268010768657, 0.3333333333333333703),
 ( 0.3333333333333333703, 0.3269284268010768657, 0.3333333333333333703, 0.3269284268010768657, 0.3333333333333333703, 0.3269284268010768657, 0.3333333333333333703, 0.3269284268010768657, 0.3333333333333333703, 0.3269284268010768657, 0.3333333333333333703, 0.3269284268010768657, 0.3333333333333333703, 0.3269284268010768657, 0.3333333333333333703, 0.3269284268010768657, 0.3333333333333333703, 0.3269284268010768657, 0.3333333333333333703, 0.3269284268010768657, 0.3333333333333333703, 0.3269284268010768657, 0.3333333333333333703, 0.3269284268010768657, 0.3333333333333333703, 0.3269284268010768657, 0.3333333333333333703, 0.3269284268010768657, 0.3333333333333333703, 0.3269284268010768657, 0.3333333333333333703, 0.3269284268010768657, 0.3333333333333333703, 0.3269284268010768657, 0.3333333333333333703, 0.3269284268010768657, 0.3333333333333333703, 0.3269284268010768657, 0.3333333333333333703, 0.3269284268010768657, 0.3333333333333333703, 0.3269284268010768657, 0.3333333333333333703, 0.3269284268010768657, 0.3333333333333333703, 0.3269284268010768657, 0.3333333333333333703, 0.3269284268010768657, 0.3333333333333333703, 0.3269284268010768657, 0.3333333333333333703, 0.3269284268010768657, 0.3333333333333333703, 0.3269284268010768657, 0.3333333333333333703, 0.3269284268010768657, 0.3333333333333333703, 0.3269284268010768657, 0.3333333333333333703, 0.3269284268010768657, 0.3333333333333333703, 0.3269284268010768657, 0.3333333333333333703, 0.3269284268010768657, 0.3333333333333333703, 0.3269284268010768657, 0.3333333333333333703, 0.3269284268010768657, 0.3333333333333333703, 0.3269284268010768657, 0.3333333333333333703, 0.3269284268010768657, 0.3333333333333333703, 0.3269284268010768657, 0.3333333333333333703, 0.3269284268010768657, 0.3333333333333333703, 0.3269284268010768657, 0.3333333333333333703, 0.3269284268010768657, 0.3333333333333333703, 0.3269284268010768657, 0.3333333333333333703, 0.3269284268010768657, 0.3333333333333333703, 0.3269284268010768657, 0.3333333333333333703, 0.3269284268010768657, 0.3333333333333333703, 0.3269284268010768657, 0.3333333333333333703, 0.3269284268010768657, 0.3333333333333333703, 0.3269284268010768657, 0.3333333333333333703, 0.3269284268010768657, 0.3333333333333333703, 0.3269284268010768657, 0.3333333333333333703, 0.3269284268010768657, 0.3333333333333333703, 0.3269284268010768657, 0.3333333333333333703, 0.3269284268010768657, 0.3333333333333333703, 0.3269284268010768657, 0.3333333333333333703, 0.3269284268010768657, 0.3333333333333333703, 0.3269284268010768657, 0.3333333333333333703, 0.3269284268010768657, 0.3333333333333333703, 0.3269284268010768657, 0.3333333333333333703, 0.3269284268010768657, 0.3333333333333333703, 0.3269284268010768657, 0.3333333333333333703, 0.3269284268010768657, 0.3333333333333333703, 0.3269284268010768657, 0.3333333333333333703, 0.3269284268010768657, 0.3333333333333333703, 0.3269284268010768657, 0.3333333333333333703, 0.3269284268010768657, 0.3333333333333333703, 0.3269284268010768657, 0.3333333333333333703, 0.3269284268010768657, 0.3333333333333333703, 0.3269284268010768657, 0.3333333333333333703, 0.3269284268010768657, 0.3333333333333333703, 0.3269284268010768657, 0.3333333333333333703, 0.3269284268010768657, 0.3333333333333333703, 0.3269284268010768657, 0.3333333333333333703, 0.3269284268010768657, 0.3333333333333333703, 0.3269284268010768657, 0.3333333333333333703, 0.3269284268010768657, 0.3333333333333333703, 0.3269284268010768657, 0.3333333333333333703, 0.3269284268010768657, 0.3333333333333333703, 0.3269284268010768657, 0.3333333333333333703, 0.3269284268010768657, 0.3333333333333333703, 0.3269284268010768657, 0.3333333333333333703, 0.3269284268010768657, 0.3333333333333333703, 0.3269284268010768657, 0.3333333333333333703, 0.3269284268010768657, 0.3333333333333333703, 0.3269284268010768657, 0.3333333333333333703, 0.3269284268010768657, 0.3333333333333333703, 0.3269284268010768657, 0.3333333333333333703, 0.3269284268010768657, 0.3333333333333333703, 0.3269284268010768657, 0.3333333333333333703, 0.3269284268010768657, 0.3333333333333333703, 0.3269284268010768657, 0.3333333333333333703, 0.3269284268010768657, 0.3333333333333333703, 0.3269284268010768657, 0.3333333333333333703, 0.3269284268010768657, 0.3333333333333333703, 0.3269284268010768657, 0.3333333333333333703, 0.3269284268010768657, 0.3333333333333333703, 0.3269284268010768657, 0.3333333333333333703, 0.3269284268010768657, 0.3333333333333333703, 0.3269284268010768657, 0.3333333333333333703, 0.3269284268010768657, 0.3333333333333333703, 0.3269284268010768657, 0.3333333333333333703, 0.3269284268010768657, 0.3333333333333333703, 0.3269284268010768657, 0.3333333333333333703, 0.3269284268010768657, 0.3333333333333333703, 0.3269284268010768657, 0.3333333333333333703, 0.3269284268010768657, 0.3333333333333333703, 0.3269284268010768657, 0.3333333333333333703, 0.3269284268010768657, 0.3333333333333333703, 0.3269284268010768657, 0.3333333333333333703, 0.3269284268010768657, 0.3333333333333333703, 0.3269284268010768657, 0.3333333333333333703, 0.3269284268010768657, 0.3333333333333333703, 0.3269284268010768657, 0.3333333333333333703, 0.3269284268010768657, 0.3333333333333333703, 0.3269284268010768657, 0.3333333333333333703, 0.3269284268010768657, 0.3333333333333333703, 0.3269284268010768657, 0.3333333333333333703, 0.3269284268010768657, 0.3333333333333333703, 0.3269284268010768657, 0.3333333333333333703, 0.3269284268010768657, 0.3333333333333333703, 0.3269284268010768657, 0.3333333333333333703, 0.3269284268010768657, 0.3333333333333333703, 0.3269284268010768657, 0.3333333333333333703, 0.3269284268010768657, 0.3333333333333333703, 0.3269284268010768657, 0.3333333333333333703, 0.3269284268010768657, 0.3333333333333333703, 0.3269284268010768657, 0.3333333333333333703, 0.3269284268010768657, 0.3333333333333333703, 0.3269284268010768657, 0.3333333333333333703, 0.3269284268010768657, 0.3333333333333333703, 0.3269284268010768657, 0.3333333333333333703, 0.3269284268010768657, 0.3333333333333333703, 0.3269284268010768657, 0.3333333333333333703, 0.3269284268010768657, 0.3333333333333333703, 0.3269284268010768657, 0.3333333333333333703, 0.3269284268010768657, 0.3333333333333333703, 0.3269284268010768657, 0.3333333333333333703, 0.3269284268010768657, 0.3333333333333333703, 0.3269284268010768657, 0.3333333333333333703, 0.3269284268010768657, 0.3333333333333333703, 0.3269284268010768657, 0.3333333333333333703, 0.3269284268010768657, 0.3333333333333333703, 0.3269284268010768657, 0.3333333333333333703, 0.3269284268010768657, 0.3333333333333333703, 0.3269284268010768657, 0.3333333333333333703, 0.3269284268010768657, 0.3333333333333333703, 0.3269284268010768657, 0.3333333333333333703, 0.3269284268010768657, 0.3333333333333333703, 0.3269284268010768657, 0.3333333333333333703, 0.3269284268010768657, 0.3333333333333333703, 0.3269284268010768657, 0.3333333333333333703, 0.3269284268010768657, 0.3333333333333333703, 0.3269284268010768657, 0.3333333333333333703, 0.3269284268010768657, 0.3333333333333333703, 0.3269284268010768657, 0.3333333333333333703, 0.3269284268010768657, 0.3333333333333333703, 0.3269284268010768657, 0.3333333333333333703, 0.3269284268010768657, 0.3333333333333333703, 0.3269284268010768657, 0.3333333333333333703, 0.3269284268010768657, 0.3333333333333333703, 0.3269284268010768657, 0.3333333333333333703, 0.3269284268010768657, 0.3333333333333333703, 0.3269284268010768657, 0.3333333333333333703, 0.3269284268010768657, 0.3333333333333333703, 0.3269284268010768657, 0.3333333333333333703, 0.3269284268010768657, 0.3333333333333333703, 0.3269284268010768657, 0.3333333333333333703, 0.3269284268010768657, 0.3333333333333333703, 0.3269284268010768657, 0.3333333333333333703, 0.3269284268010768657, 0.3333333333333333703, 0.3269284268010768657, 0.3333333333333333703, 0.3269284268010768657, 0.3333333333333333703, 0.3269284268010768657, 0.3333333333333333703, 0.3269284268010768657, 0.3333333333333333703, 0.3269284268010768657, 0.3333333333333333703, 0.3269284268010768657, 0.3333333333333333703, 0.3269284268010768657, 0.3333333333333333703, 0.3269284268010768657, 0.3333333333333333703, 0.3269284268010768657, 0.3333333333333333703, 0.3269284268010768657, 0.3333333333333333703, 0.3269284268010768657, 0.3333333333333333703, 0.3269284268010768657, 0.3333333333333333703, 0.3269284268010768657, 0.3333333333333333703, 0.3269284268010768657, 0.3333333333333333703, 0.3269284268010768657, 0.3333333333333333703, 0.3269284268010768657, 0.3333333333333333703, 0.3269284268010768657, 0.3333333333333333703, 0.3269284268010768657, 0.3333333333333333703, 0.3269284268010768657, 0.3333333333333333703, 0.3269284268010768657, 0.3333333333333333703, 0.3269284268010768657, 0.3333333333333333703, 0.3269284268010768657, 0.3333333333333333703, 0.3269284268010768657, 0.3333333333333333703, 0.3269284268010768657, 0.3333333333333333703, 0.3269284268010768657, 0.3333333333333333703, 0.3269284268010768657, 0.3333333333333333703, 0.3269284268010768657, 0.3333333333333333703, 0.3269284268010768657, 0.3333333333333333703, 0.3269284268010768657, 0.3333333333333333703, 0.3269284268010768657, 0.3333333333333333703, 0.3269284268010768657, 0.3333333333333333703, 0.3269284268010768657, 0.3333333333333333703, 0.3269284268010768657, 0.3333333333333333703, 0.3269284268010768657, 0.3333333333333333703, 0.3269284268010768657, 0.3333333333333333703, 0.3269284268010768657, 0.3333333333333333703, 0.3269284268010768657, 0.3333333333333333703, 0.3269284268010768657, 0.3333333333333333703, 0.3269284268010768657, 0.3333333333333333703, 0.3269284268010768657, 0.3333333333333333703, 0.3269284268010768657, 0.3333333333333333703, 0.3269284268010768657, 0.3333333333333333703, 0.3269284268010768657, 0.3333333333333333703, 0.3269284268010768657, 0.3333333333333333703, 0.3269284268010768657, 0.3333333333333333703, 0.3269284268010768657, 0.3333333333333333703, 0.3269284268010768657, 0.3333333333333333703, 0.3269284268010768657, 0.3333333333333333703, 0.3269284268010768657, 0.3333333333333333703, 0.3269284268010768657, 0.3333333333333333703, 0.3269284268010768657, 0.3333333333333333703, 0.3269284268010768657, 0.3333333333333333703, 0.3269284268010768657, 0.3333333333333333703, 0.3269284268010768657, 0.3333333333333333703, 0.3269284268010768657, 0.3333333333333333703, 0.3269284268010768657, 0.3333333333333333703, 0.3269284268010768657, 0.3333333333333333703, 0.3269284268010768657, 0.3333333333333333703, 0.3269284268010768657, 0.3333333333333333703, 0.3269284268010768657, 0.3333333333333333703, 0.3269284268010768657, 0.3333333333333333703, 0.3269284268010768657, 0.3333333333333333703, 0.3269284268010768657, 0.3333333333333333703, 0.3269284268010768657, 0.3333333333333333703, 0.3269284268010768657, 0.3333333333333333703, 0.3269284268010768657, 0.3333333333333333703, 0.3269284268010768657, 0.3333333333333333703, 0.3269284268010768657, 0.3333333333333333703, 0.3269284268010768657, 0.3333333333333333703, 0.3269284268010768657, 0.3333333333333333703, 0.3269284268010768657, 0.3333333333333333703, 0.3269284268010768657, 0.3333333333333333703),
 ( 1.000000000000000000, 0.9807852804032304306, 1.000000000000000000, 0.9807852804032304306, 1.000000000000000000, 0.9807852804032304306, 1.000000000000000000, 0.9807852804032304306, 1.000000000000000000, 0.9807852804032304306, 1.000000000000000000, 0.9807852804032304306, 1.000000000000000000, 0.9807852804032304306, 1.000000000000000000, 0.9807852804032304306, 1.000000000000000000, 0.9807852804032304306, 1.000000000000000000, 0.9807852804032304306, 1.000000000000000000, 0.9807852804032304306, 1.000000000000000000, 0.9807852804032304306, 1.000000000000000000, 0.9807852804032304306, 1.000000000000000000, 0.9807852804032304306, 1.000000000000000000, 0.9807852804032304306, 1.000000000000000000, 0.9807852804032304306, 1.000000000000000000, 0.9807852804032304306, 1.000000000000000000, 0.9807852804032304306, 1.000000000000000000, 0.9807852804032304306, 1.000000000000000000, 0.9807852804032304306, 1.000000000000000000, 0.9807852804032304306, 1.000000000000000000, 0.9807852804032304306, 1.000000000000000000, 0.9807852804032304306, 1.000000000000000000, 0.9807852804032304306, 1.000000000000000000, 0.9807852804032304306, 1.000000000000000000, 0.9807852804032304306, 1.000000000000000000, 0.9807852804032304306, 1.000000000000000000, 0.9807852804032304306, 1.000000000000000000, 0.9807852804032304306, 1.000000000000000000, 0.9807852804032304306, 1.000000000000000000, 0.9807852804032304306, 1.000000000000000000, 0.9807852804032304306, 1.000000000000000000, 0.9807852804032304306, 1.000000000000000000, 0.9807852804032304306, 1.000000000000000000, 0.9807852804032304306, 1.000000000000000000, 0.9807852804032304306, 1.000000000000000000, 0.9807852804032304306, 1.000000000000000000, 0.9807852804032304306, 1.000000000000000000, 0.9807852804032304306, 1.000000000000000000, 0.9807852804032304306, 1.000000000000000000, 0.9807852804032304306, 1.000000000000000000, 0.9807852804032304306, 1.000000000000000000, 0.9807852804032304306, 1.000000000000000000, 0.9807852804032304306, 1.000000000000000000, 0.9807852804032304306, 1.000000000000000000, 0.9807852804032304306, 1.000000000000000000, 0.9807852804032304306, 1.000000000000000000, 0.9807852804032304306, 1.000000000000000000, 0.9807852804032304306, 1.000000000000000000, 0.9807852804032304306, 1.000000000000000000, 0.9807852804032304306, 1.000000000000000000, 0.9807852804032304306, 1.000000000000000000, 0.9807852804032304306, 1.000000000000000000, 0.9807852804032304306, 1.000000000000000000, 0.9807852804032304306, 1.000000000000000000, 0.9807852804032304306, 1.000000000000000000, 0.9807852804032304306, 1.000000000000000000, 0.9807852804032304306, 1.000000000000000000, 0.9807852804032304306, 1.000000000000000000, 0.9807852804032304306, 1.000000000000000000, 0.9807852804032304306, 1.000000000000000000, 0.9807852804032304306, 1.000000000000000000, 0.9807852804032304306, 1.000000000000000000, 0.9807852804032304306, 1.000000000000000000, 0.9807852804032304306, 1.000000000000000000, 0.9807852804032304306, 1.000000000000000000, 0.9807852804032304306, 1.000000000000000000, 0.9807852804032304306, 1.000000000000000000, 0.9807852804032304306, 1.000000000000000000, 0.9807852804032304306, 1.000000000000000000, 0.9807852804032304306, 1.000000000000000000, 0.9807852804032304306, 1.000000000000000000, 0.9807852804032304306, 1.000000000000000000, 0.9807852804032304306, 1.000000000000000000, 0.9807852804032304306, 1.000000000000000000, 0.9807852804032304306, 1.000000000000000000, 0.9807852804032304306, 1.000000000000000000, 0.9807852804032304306, 1.000000000000000000, 0.9807852804032304306, 1.000000000000000000, 0.9807852804032304306, 1.000000000000000000, 0.9807852804032304306, 1.000000000000000000, 0.9807852804032304306, 1.000000000000000000, 0.9807852804032304306, 1.000000000000000000, 0.9807852804032304306, 1.000000000000000000, 0.9807852804032304306, 1.000000000000000000, 0.9807852804032304306, 1.000000000000000000, 0.9807852804032304306, 1.000000000000000000, 0.9807852804032304306, 1.000000000000000000, 0.9807852804032304306, 1.000000000000000000, 0.9807852804032304306, 1.000000000000000000, 0.9807852804032304306, 1.000000000000000000, 0.9807852804032304306, 1.000000000000000000, 0.9807852804032304306, 1.000000000000000000, 0.9807852804032304306, 1.000000000000000000, 0.9807852804032304306, 1.000000000000000000, 0.9807852804032304306, 1.000000000000000000, 0.9807852804032304306, 1.000000000000000000, 0.9807852804032304306, 1.000000000000000000, 0.9807852804032304306, 1.000000000000000000, 0.9807852804032304306, 1.000000000000000000, 0.9807852804032304306, 1.000000000000000000, 0.9807852804032304306, 1.000000000000000000, 0.9807852804032304306, 1.000000000000000000, 0.9807852804032304306, 1.000000000000000000, 0.9807852804032304306, 1.000000000000000000, 0.9807852804032304306, 1.000000000000000000, 0.9807852804032304306, 1.000000000000000000, 0.9807852804032304306, 1.000000000000000000, 0.9807852804032304306, 1.000000000000000000, 0.9807852804032304306, 1.000000000000000000, 0.9807852804032304306, 1.000000000000000000, 0.9807852804032304306, 1.000000000000000000, 0.9807852804032304306, 1.000000000000000000, 0.9807852804032304306, 1.000000000000000000, 0.9807852804032304306, 1.000000000000000000, 0.9807852804032304306, 1.000000000000000000, 0.9807852804032304306, 1.000000000000000000, 0.9807852804032304306, 1.000000000000000000, 0.9807852804032304306, 1.000000000000000000, 0.9807852804032304306, 1.000000000000000000, 0.9807852804032304306, 1.000000000000000000, 0.9807852804032304306, 1.000000000000000000, 0.9807852804032304306, 1.000000000000000000, 0.9807852804032304306, 1.000000000000000000, 0.9807852804032304306, 1.000000000000000000, 0.9807852804032304306, 1.000000000000000000, 0.9807852804032304306, 1.000000000000000000, 0.9807852804032304306, 1.000000000000000000, 0.9807852804032304306, 1.000000000000000000, 0.9807852804032304306, 1.000000000000000000, 0.9807852804032304306, 1.000000000000000000, 0.9807852804032304306, 1.000000000000000000, 0.9807852804032304306, 1.000000000000000000, 0.9807852804032304306, 1.000000000000000000, 0.9807852804032304306, 1.000000000000000000, 0.9807852804032304306, 1.000000000000000000, 0.9807852804032304306, 1.000000000000000000, 0.9807852804032304306, 1.000000000000000000, 0.9807852804032304306, 1.000000000000000000, 0.9807852804032304306, 1.000000000000000000, 0.9807852804032304306, 1.000000000000000000, 0.9807852804032304306, 1.000000000000000000, 0.9807852804032304306, 1.000000000000000000, 0.9807852804032304306, 1.000000000000000000, 0.9807852804032304306, 1.000000000000000000, 0.9807852804032304306, 1.000000000000000000, 0.9807852804032304306, 1.000000000000000000, 0.9807852804032304306, 1.000000000000000000, 0.9807852804032304306, 1.000000000000000000, 0.9807852804032304306, 1.000000000000000000, 0.9807852804032304306, 1.000000000000000000, 0.9807852804032304306, 1.000000000000000000, 0.9807852804032304306, 1.000000000000000000, 0.9807852804032304306, 1.000000000000000000, 0.9807852804032304306, 1.000000000000000000, 0.9807852804032304306, 1.000000000000000000, 0.9807852804032304306, 1.000000000000000000, 0.9807852804032304306, 1.000000000000000000, 0.9807852804032304306, 1.000000000000000000, 0.9807852804032304306, 1.000000000000000000, 0.9807852804032304306, 1.000000000000000000, 0.9807852804032304306, 1.000000000000000000, 0.9807852804032304306, 1.000000000000000000, 0.9807852804032304306, 1.000000000000000000, 0.9807852804032304306, 1.000000000000000000, 0.9807852804032304306, 1.000000000000000000, 0.9807852804032304306, 1.000000000000000000, 0.9807852804032304306, 1.000000000000000000, 0.9807852804032304306, 1.000000000000000000, 0.9807852804032304306, 1.000000000000000000, 0.9807852804032304306, 1.000000000000000000, 0.9807852804032304306, 1.000000000000000000, 0.9807852804032304306, 1.000000000000000000, 0.9807852804032304306, 1.000000000000000000, 0.9807852804032304306, 1.000000000000000000, 0.9807852804032304306, 1.000000000000000000, 0.9807852804032304306, 1.000000000000000000, 0.9807852804032304306, 1.000000000000000000, 0.9807852804032304306, 1.000000000000000000, 0.9807852804032304306, 1.000000000000000000, 0.9807852804032304306, 1.000000000000000000, 0.9807852804032304306, 1.000000000000000000, 0.9807852804032304306, 1.000000000000000000, 0.9807852804032304306, 1.000000000000000000, 0.9807852804032304306, 1.000000000000000000, 0.9807852804032304306, 1.000000000000000000, 0.9807852804032304306, 1.000000000000000000, 0.9807852804032304306, 1.000000000000000000, 0.9807852804032304306, 1.000000000000000000, 0.9807852804032304306, 1.000000000000000000, 0.9807852804032304306, 1.000000000000000000, 0.9807852804032304306, 1.000000000000000000, 0.9807852804032304306, 1.000000000000000000, 0.9807852804032304306, 1.000000000000000000, 0.9807852804032304306, 1.000000000000000000, 0.9807852804032304306, 1.000000000000000000, 0.9807852804032304306, 1.000000000000000000, 0.9807852804032304306, 1.000000000000000000, 0.9807852804032304306, 1.000000000000000000, 0.9807852804032304306, 1.000000000000000000, 0.9807852804032304306, 1.000000000000000000, 0.9807852804032304306, 1.000000000000000000, 0.9807852804032304306, 1.000000000000000000, 0.9807852804032304306, 1.000000000000000000, 0.9807852804032304306, 1.000000000000000000, 0.9807852804032304306, 1.000000000000000000, 0.9807852804032304306, 1.000000000000000000, 0.9807852804032304306, 1.000000000000000000, 0.9807852804032304306, 1.000000000000000000, 0.9807852804032304306, 1.000000000000000000, 0.9807852804032304306, 1.000000000000000000, 0.9807852804032304306, 1.000000000000000000, 0.9807852804032304306, 1.000000000000000000, 0.9807852804032304306, 1.000000000000000000, 0.9807852804032304306, 1.000000000000000000, 0.9807852804032304306, 1.000000000000000000, 0.9807852804032304306, 1.000000000000000000, 0.9807852804032304306, 1.000000000000000000, 0.9807852804032304306, 1.000000000000000000, 0.9807852804032304306, 1.000000000000000000, 0.9807852804032304306, 1.000000000000000000, 0.9807852804032304306, 1.000000000000000000, 0.9807852804032304306, 1.000000000000000000, 0.9807852804032304306, 1.000000000000000000, 0.9807852804032304306, 1.000000000000000000, 0.9807852804032304306, 1.000000000000000000, 0.9807852804032304306, 1.000000000000000000, 0.9807852804032304306, 1.000000000000000000, 0.9807852804032304306, 1.000000000000000000, 0.9807852804032304306, 1.000000000000000000, 0.9807852804032304306, 1.000000000000000000, 0.9807852804032304306, 1.000000000000000000, 0.9807852804032304306, 1.000000000000000000, 0.9807852804032304306, 1.000000000000000000, 0.9807852804032304306, 1.000000000000000000, 0.9807852804032304306, 1.000000000000000000, 0.9807852804032304306, 1.000000000000000000, 0.9807852804032304306, 1.000000000000000000, 0.9807852804032304306, 1.000000000000000000, 0.9807852804032304306, 1.000000000000000000) ) ) 
 REPRESENTATION_ITEM ( '' )  SURFACE ( )  );
#295 = CARTESIAN_POINT ( 'NONE',  ( 26.99999999999999645, 241.6374999999999886, 3.464101615137751278 ) ) ;
#296 = CARTESIAN_POINT ( 'NONE',  ( 5.727106289114498080E-15, 199.2125000000000057, 31.17691453623979214 ) ) ;
#297 = CARTESIAN_POINT ( 'NONE',  ( 8.962234695871762469, 62.16018628210144215, -8.715434833791931624 ) ) ;
#298 = ORIENTED_EDGE ( 'NONE', *, *, #35567, .F. ) ;
#299 = EDGE_LOOP ( 'NONE', ( #11498, #11713, #35971, #5755 ) ) ;
#300 = CARTESIAN_POINT ( 'NONE',  ( 24.61867908796596183, 0.000000000000000000, 160.2039707163872038 ) ) ;
#301 = LINE ( 'NONE', #23435, #5184 ) ;
#302 = DIRECTION ( 'NONE',  ( -0.000000000000000000, -1.000000000000000000, -0.000000000000000000 ) ) ;
#303 = CARTESIAN_POINT ( 'NONE',  ( 15.24356964374999990, 3.323476615752268604, -6.028124999385455318 ) ) ;
#304 = CARTESIAN_POINT ( 'NONE',  ( 13.04141134922778988, 47.02731371789855075, -8.927990412390371944 ) ) ;
#305 = DIRECTION ( 'NONE',  ( 0.000000000000000000, -1.000000000000000000, 0.000000000000000000 ) ) ;
#306 = CARTESIAN_POINT ( 'NONE',  ( 15.24356964374999990, 239.9593750006145285, 0.000000000000000000 ) ) ;
#307 = CARTESIAN_POINT ( 'NONE',  ( -65.43377896937850835, 208.9097554298617183, 4.530955311639234040 ) ) ;
#308 = DIRECTION ( 'NONE',  ( 0.000000000000000000, 0.000000000000000000, 1.000000000000000000 ) ) ;
#309 = CARTESIAN_POINT ( 'NONE',  ( 28.35571312319377313, 5.196152422706630247, 168.4973254592314618 ) ) ;
#310 = CARTESIAN_POINT ( 'NONE',  ( 9.534712964251900402, 20.57731371789854435, 1.715153634034445540 ) ) ;
#311 = CARTESIAN_POINT ( 'NONE',  ( -65.83705436395487709, 205.3262412349647263, -4.842901733360204020 ) ) ;
#312 = CARTESIAN_POINT ( 'NONE',  ( -48.61086230271182984, 214.1499508600178387, -7.418979330068641964 ) ) ;
#313 = AXIS2_PLACEMENT_3D ( 'NONE', #22514, #37081, #34061 ) ;
#314 =( BOUNDED_CURVE ( )  B_SPLINE_CURVE ( 2, ( #13110, #21469, #7242, #4198, #30360, #25227, #30737 ),
 .UNSPECIFIED., .F., .F. ) 
 B_SPLINE_CURVE_WITH_KNOTS ( ( 3, 2, 2, 3 ),
 ( 0.5000000000000013323, 0.5072463768115947902, 0.5144927536231880261, 0.5217391304347814840 ),
 .UNSPECIFIED. ) 
 CURVE ( )  GEOMETRIC_REPRESENTATION_ITEM ( )  RATIONAL_B_SPLINE_CURVE ( ( 0.9999999999999753530, 0.8660254037844633546, 1.000000000000000000, 0.8660254037844387076, 1.000000000000000000, 0.8660254037844592467, 0.9999999999999794609 ) ) 
 REPRESENTATION_ITEM ( '' )  );
#315 = APPLICATION_PROTOCOL_DEFINITION ( 'draft international standard', 'automotive_design', 1998, #8119 ) ;
#316 = CARTESIAN_POINT ( 'NONE',  ( 25.00272249592519103, 194.9999999999998863, 10.65893590749716324 ) ) ;
#317 = CARTESIAN_POINT ( 'NONE',  ( -27.24356964375000345, 195.8093750006145513, 0.000000000000000000 ) ) ;
#318 = CARTESIAN_POINT ( 'NONE',  ( 5.770363421894130873, 128.9648137178985792, -14.38691631536193860 ) ) ;
#319 = EDGE_LOOP ( 'NONE', ( #2535, #440, #17456, #4187 ) ) ;
#320 = CARTESIAN_POINT ( 'NONE',  ( -0.1745138560725500443, 47.21018628210143930, 12.50000000000000355 ) ) ;
#321 = CARTESIAN_POINT ( 'NONE',  ( 15.00000000000000000, 244.6187500012290741, -3.464101615137752610 ) ) ;
#322 = EDGE_CURVE ( 'NONE', #20414, #21332, #8073, .T. ) ;
#323 = CARTESIAN_POINT ( 'NONE',  ( 21.00000000000016342, -4.000000000000002665, 50.00000000000000000 ) ) ;
#324 = CARTESIAN_POINT ( 'NONE',  ( 37.56655944895057075, 3.604726614523243278, 167.7197132565624713 ) ) ;
#325 = CARTESIAN_POINT ( 'NONE',  ( 21.00000000000000000, 6.928203230275506996, -1.406249998770969123 ) ) ;
#326 = CARTESIAN_POINT ( 'NONE',  ( 13.44051670066911264, -5.407089921784865361, -10.02187499938553294 ) ) ;
#327 = CARTESIAN_POINT ( 'NONE',  ( -69.79538769728823411, 211.8571965466040012, -6.469044688360769513 ) ) ;
#328 = CARTESIAN_POINT ( 'NONE',  ( 13.44051670066911441, 5.407089921784856479, -2.915624999385552307 ) ) ;
#329 = CARTESIAN_POINT ( 'NONE',  ( 3.796722387233379514, 52.38518628210145778, -8.710071997420127943 ) ) ;
#330 = FACE_OUTER_BOUND ( 'NONE', #17009, .T. ) ;
#331 = DIRECTION ( 'NONE',  ( 0.000000000000000000, -0.000000000000000000, -1.000000000000000000 ) ) ;
#332 = CARTESIAN_POINT ( 'NONE',  ( -2.660918448318275509, 93.49768628210145494, 12.46528703574805874 ) ) ;
#333 = CARTESIAN_POINT ( 'NONE',  ( 26.99999999999999645, 199.8125000000000000, -15.58845726811990495 ) ) ;
#334 = CARTESIAN_POINT ( 'NONE',  ( -20.80563922340697403, 195.0000000000000284, -17.20829382900668136 ) ) ;
#335 = EDGE_LOOP ( 'NONE', ( #19344, #12527, #16125, #26950 ) ) ;
#336 = CARTESIAN_POINT ( 'NONE',  ( 24.36378002397578868, 0.000000000000000000, 160.0851093307920223 ) ) ;
#337 = AXIS2_PLACEMENT_3D ( 'NONE', #15365, #24083, #35628 ) ;
#338 = CARTESIAN_POINT ( 'NONE',  ( 26.75643035624999655, -3.323476615752267715, -8.053124999385453009 ) ) ;
#339 = CARTESIAN_POINT ( 'NONE',  ( -1.926257025242585782E-15, 196.5968750006145456, -31.45816453501076637 ) ) ;
#340 = CARTESIAN_POINT ( 'NONE',  ( 37.21031035046954116, 7.646167579472024665E-16, 163.6477674281124450 ) ) ;
#341 = CARTESIAN_POINT ( 'NONE',  ( 25.01414827068343172, -3.464101615137761048, 164.7242041589784947 ) ) ;
#342 = CARTESIAN_POINT ( 'NONE',  ( 10.56230152254331323, 3.464101615137297419, -9.037500000000031619 ) ) ;
#343 = CARTESIAN_POINT ( 'NONE',  ( 26.99999999999999645, 249.3249999999999886, -7.347880794884117764E-16 ) ) ;
#344 = CARTESIAN_POINT ( 'NONE',  ( 13.62178482187499640, 197.4031250006145228, -23.59362340125807123 ) ) ;
#345 = CARTESIAN_POINT ( 'NONE',  ( -7.228626920338836470, 127.5273137178985792, -10.49813415416005213 ) ) ;
#346 = APPLICATION_CONTEXT ( 'automotive_design' ) ;
#347 = CARTESIAN_POINT ( 'NONE',  ( 0.1745138560725515708, 116.2101862821014606, -12.50000000000000355 ) ) ;
#349 = ORIENTED_EDGE ( 'NONE', *, *, #34489, .T. ) ;
#348 = ORIENTED_EDGE ( 'NONE', *, *, #4481, .T. ) ;
#350 = CARTESIAN_POINT ( 'NONE',  ( 27.24356964375000700, 195.0406250006145399, 15.72908226750537075 ) ) ;
#351 = CARTESIAN_POINT ( 'NONE',  ( 21.00000000000000000, 241.5343750006145171, -6.646953231504538984 ) ) ;
#352 = EDGE_CURVE ( 'NONE', #13050, #23173, #13433, .T. ) ;
#353 = CARTESIAN_POINT ( 'NONE',  ( 6.092822981423662299, 86.41481371789855359, 14.25334919248795096 ) ) ;
#354 = CARTESIAN_POINT ( 'NONE',  ( 18.12178482187500350, -4.985214923628407568, -4.678124999385496530 ) ) ;
#355 = CARTESIAN_POINT ( 'NONE',  ( 15.24356964375000167, 248.0968750006145456, 3.323476615752272600 ) ) ;
#356 =( BOUNDED_CURVE ( )  B_SPLINE_CURVE ( 2, ( #17925, #26623, #26814, #31940, #5972, #15073, #12223, #29469, #653 ),
 .UNSPECIFIED., .F., .F. ) 
 B_SPLINE_CURVE_WITH_KNOTS ( ( 3, 2, 2, 2, 3 ),
 ( 0.7934782608695651884, 0.7971014492753623060, 0.8043478260869565410, 0.8115942028985507761, 0.8152173913043478937 ),
 .UNSPECIFIED. ) 
 CURVE ( )  GEOMETRIC_REPRESENTATION_ITEM ( )  RATIONAL_B_SPLINE_CURVE ( ( 0.9330127018922194093, 0.9330127018922194093, 1.000000000000000000, 0.8660254037844387076, 1.000000000000000000, 0.8660254037844387076, 1.000000000000000000, 0.9330127018922182991, 0.9330127018922192983 ) ) 
 REPRESENTATION_ITEM ( '' )  );
#357 = CARTESIAN_POINT ( 'NONE',  ( 13.49999999999999645, 196.3625000012290513, -23.38268590217984766 ) ) ;
#358 = CARTESIAN_POINT ( 'NONE',  ( 8.710071997420211432, 84.11481371789855643, -3.796722387233181895 ) ) ;
#359 = CARTESIAN_POINT ( 'NONE',  ( 22.80587116629411071, 3.604726614523238837, -5.728124999385511451 ) ) ;
#360 = CARTESIAN_POINT ( 'NONE',  ( 23.87821517812499650, 241.9468750006145115, -4.985214923628404904 ) ) ;
#361 = CARTESIAN_POINT ( 'NONE',  ( 4.944772684328420986, 40.41481371789855359, 11.48171059495408208 ) ) ;
#362 = CYLINDRICAL_SURFACE ( 'NONE', #12150, 2.649999999999999467 ) ;
#363 = CARTESIAN_POINT ( 'NONE',  ( 4.944772684328679446, 107.5851862821014464, -11.48171059495397373 ) ) ;
#364 = CARTESIAN_POINT ( 'NONE',  ( 10.56230152254410726, 0.000000000000000000, -4.387499998770999277 ) ) ;
#365 = CARTESIAN_POINT ( 'NONE',  ( -36.54538769728823411, 211.8571965466039444, -6.469044688360768625 ) ) ;
#366 = CARTESIAN_POINT ( 'NONE',  ( -8.962234695871760692, 140.3601862821014379, 8.715434833791933400 ) ) ;
#367 = CARTESIAN_POINT ( 'NONE',  ( 0.000000000000000000, 210.0000000000000284, 0.000000000000000000 ) ) ;
#368 = CARTESIAN_POINT ( 'NONE',  ( 11.08355503943142750, 80.56018628210146915, -10.83675517735155225 ) ) ;
#369 = CARTESIAN_POINT ( 'NONE',  ( 12.48663586349064403, 194.9999999999999716, 24.21355016816918493 ) ) ;
#370 = FACE_BOUND ( 'NONE', #668, .T. ) ;
#371 = CARTESIAN_POINT ( 'NONE',  ( 0.3500000000000065281, 244.5000000000000000, 2.500000000000000000 ) ) ;
#372 = CARTESIAN_POINT ( 'NONE',  ( -8.843639120294326972, 113.3351862821014606, 3.474262827703335166 ) ) ;
#373 = DIRECTION ( 'NONE',  ( 0.000000000000000000, 0.000000000000000000, -1.000000000000000000 ) ) ;
#374 = CARTESIAN_POINT ( 'NONE',  ( -11.08355503943142573, 11.56018628210145316, 10.83675517735155402 ) ) ;
#375 = FACE_OUTER_BOUND ( 'NONE', #36390, .T. ) ;
#376 = CARTESIAN_POINT ( 'NONE',  ( 23.87821517812499650, 241.4968750006144944, -4.985214923628404904 ) ) ;
#377 = ORIENTED_EDGE ( 'NONE', *, *, #18191, .T. ) ;
#378 = CARTESIAN_POINT ( 'NONE',  ( 37.64336544724692146, -3.604726614523235284, 168.5976098342557918 ) ) ;
#379 = CARTESIAN_POINT ( 'NONE',  ( 2.064181346179272847, 52.09768628210144925, -9.465287035748065847 ) ) ;
#380 = CARTESIAN_POINT ( 'NONE',  ( 26.75643035624999655, 7.049594010296217766E-16, -1.265624999385456251 ) ) ;
#381 = VECTOR ( 'NONE', #24853, 1000.000000000000000 ) ;
#382 = CARTESIAN_POINT ( 'NONE',  ( 26.99999999999999645, 241.6375000000000171, 3.464101615137751278 ) ) ;
#383 = CARTESIAN_POINT ( 'NONE',  ( 22.56230152254385501, 3.464101615137912926, -7.837500000000038547 ) ) ;
#384 = FACE_BOUND ( 'NONE', #21248, .T. ) ;
#385 = DIRECTION ( 'NONE',  ( -1.000000000000000000, 0.000000000000000000, 0.000000000000000000 ) ) ;
#386 = CARTESIAN_POINT ( 'NONE',  ( 22.56230152254410370, 0.000000000000000000, -10.00000000000000000 ) ) ;
#387 = CARTESIAN_POINT ( 'NONE',  ( 1.715153634034445762, 45.87731371789854506, -9.534712964251895073 ) ) ;
#388 = CARTESIAN_POINT ( 'NONE',  ( 27.24356964374999279, 199.2218750006145171, -15.72908226750539207 ) ) ;
#389 = ORIENTED_EDGE ( 'NONE', *, *, #10539, .F. ) ;
#390 = CARTESIAN_POINT ( 'NONE',  ( 26.75643035624999655, 248.6593750006145171, -3.323476615752271712 ) ) ;
#391 = CARTESIAN_POINT ( 'NONE',  ( 12.53471296425189330, 48.17731371789854222, 2.311890736173451533 ) ) ;
#392 = CARTESIAN_POINT ( 'NONE',  ( 18.12178482187499640, 4.985214923628404904, -8.428124999385472549 ) ) ;
#393 = CARTESIAN_POINT ( 'NONE',  ( 4.944772684328420986, 12.81481371789855395, 11.48171059495408208 ) ) ;
#394 = CARTESIAN_POINT ( 'NONE',  ( 2.999999999999997335, 244.5000000000000000, 2.500000000000000000 ) ) ;
#395 = ORIENTED_EDGE ( 'NONE', *, *, #6389, .F. ) ;
#396 = CARTESIAN_POINT ( 'NONE',  ( 10.31873187879411269, 3.604726614523240613, -4.284374999385516247 ) ) ;
#397 = ORIENTED_EDGE ( 'NONE', *, *, #22014, .F. ) ;
#398 = CARTESIAN_POINT ( 'NONE',  ( -27.24356964375000345, 198.4531250006145342, 0.000000000000000000 ) ) ;
#399 = CARTESIAN_POINT ( 'NONE',  ( 28.05054758442196672, 5.407089921784862696, 166.4065915139379115 ) ) ;
#400 = CARTESIAN_POINT ( 'NONE',  ( -34.95461230271183695, 208.1428034533959135, -6.469044688360754414 ) ) ;
#401 = CARTESIAN_POINT ( 'NONE',  ( 20.99999999999999289, 245.4437500012290343, -5.999999999999997335 ) ) ;
#402 = DIRECTION ( 'NONE',  ( 0.9961946980917462113, 0.000000000000000000, -0.08715574274765118534 ) ) ;
#403 = CARTESIAN_POINT ( 'NONE',  ( -55.14211230271182984, 205.5309553116392465, 1.321298161741817356 ) ) ;
#404 = CARTESIAN_POINT ( 'NONE',  ( -34.36830436395490551, 209.8844732041982581, 6.500000000000000888 ) ) ;
#405 = CARTESIAN_POINT ( 'NONE',  ( -69.00000000000002842, 214.0000000000000000, -2.499999999999998668 ) ) ;
#406 = AXIS2_PLACEMENT_3D ( 'NONE', #8514, #8149, #2814 ) ;
#407 = VERTEX_POINT ( 'NONE', #11887 ) ;
#408 = CARTESIAN_POINT ( 'NONE',  ( 15.00000000000000000, 248.6500000000000057, 0.000000000000000000 ) ) ;
#409 = CARTESIAN_POINT ( 'NONE',  ( 15.53471296425188797, 29.77731371789854364, 2.908627838312457747 ) ) ;
#410 = CARTESIAN_POINT ( 'NONE',  ( -56.33705436395490551, 203.8621396198270475, -6.307003348497942419 ) ) ;
#411 = CARTESIAN_POINT ( 'NONE',  ( 9.500000000000005329, 127.7101862821014606, 0.1745138560725188748 ) ) ;
#412 = EDGE_CURVE ( 'NONE', #35111, #30074, #26288, .T. ) ;
#413 = CARTESIAN_POINT ( 'NONE',  ( 8.715434833791931624, 27.66018628210144215, 8.962234695871760692 ) ) ;
#414 = EDGE_CURVE ( 'NONE', #36155, #4778, #26130, .T. ) ;
#415 = CARTESIAN_POINT ( 'NONE',  ( 16.56230152254411081, 6.928203230275514990, -3.712500000000020339 ) ) ;
#416 = ORIENTED_EDGE ( 'NONE', *, *, #28626, .T. ) ;
#417 = CARTESIAN_POINT ( 'NONE',  ( -42.68080436395489841, 203.5000000000000000, -0.1155267958017335561 ) ) ;
#418 = CARTESIAN_POINT ( 'NONE',  ( 10.56230152254458865, 3.464101615138028389, -5.324999998771027698 ) ) ;
#419 = CARTESIAN_POINT ( 'NONE',  ( 2.064181346179272847, 15.29768628210142722, -9.465287035748065847 ) ) ;
#420 = CARTESIAN_POINT ( 'NONE',  ( 27.24356964375000700, 195.5468750006145342, 15.72908226750537075 ) ) ;
#421 = CARTESIAN_POINT ( 'NONE',  ( 13.50000000000001421, 195.7625000012290570, 23.38268590217984055 ) ) ;
#422 = CARTESIAN_POINT ( 'NONE',  ( -1.045839947578415010E-13, 196.1750000012290229, 27.00000000000000355 ) ) ;
#423 = CARTESIAN_POINT ( 'NONE',  ( 0.000000000000000000, 143.0000000000000000, 0.000000000000000000 ) ) ;
#424 = CARTESIAN_POINT ( 'NONE',  ( 25.44883753774445978, 3.464101615137752610, 169.6927252169354290 ) ) ;
#425 = EDGE_CURVE ( 'NONE', #21070, #14808, #25046, .T. ) ;
#426 = CARTESIAN_POINT ( 'NONE',  ( 21.00000000000000000, 245.2468750006145228, -6.646953231504538984 ) ) ;
#427 = CARTESIAN_POINT ( 'NONE',  ( 2.064181346179061460, 86.70231371789851949, 9.465287035748106703 ) ) ;
#428 = CARTESIAN_POINT ( 'NONE',  ( 18.12178482187500350, 240.0343750006145171, 4.985214923628407568 ) ) ;
#429 = ORIENTED_EDGE ( 'NONE', *, *, #547, .F. ) ;
#430 = CARTESIAN_POINT ( 'NONE',  ( -58.51413769728823411, 213.1499508600178672, 5.686928522499718142 ) ) ;
#431 = VECTOR ( 'NONE', #33908, 1000.000000000000000 ) ;
#432 = CARTESIAN_POINT ( 'NONE',  ( 21.00000000000000000, 247.2437500012290457, -6.928203230275506996 ) ) ;
#433 = CARTESIAN_POINT ( 'NONE',  ( 7.228626920338837358, 95.32731371789856212, 10.49813415416005036 ) ) ;
#434 = CARTESIAN_POINT ( 'NONE',  ( 10.31873187879410736, 3.604726614523240613, -1.584374999385509630 ) ) ;
#435 = CARTESIAN_POINT ( 'NONE',  ( 30.67183618977810156, -7.209453229046475009, 160.5495935129122245 ) ) ;
#436 = CARTESIAN_POINT ( 'NONE',  ( 26.75643035624999655, 7.049594010296217766E-16, -3.178124999385495641 ) ) ;
#437 = CARTESIAN_POINT ( 'NONE',  ( -4.944772684328424539, 63.41481371789856070, -11.48171059495408031 ) ) ;
#438 = CARTESIAN_POINT ( 'NONE',  ( -27.24356964375000345, 198.0593750006145513, 0.000000000000000000 ) ) ;
#439 = ORIENTED_EDGE ( 'NONE', *, *, #30910, .T. ) ;
#440 = ORIENTED_EDGE ( 'NONE', *, *, #16671, .T. ) ;
#441 = CARTESIAN_POINT ( 'NONE',  ( 26.75643035624999655, -3.323476615752267271, -6.253124999385469174 ) ) ;
#442 = DIRECTION ( 'NONE',  ( 0.1219804832088915436, 0.9925324990730154395, 0.000000000000000000 ) ) ;
#443 = CARTESIAN_POINT ( 'NONE',  ( 26.75643035624999655, 247.6843750006145513, 3.323476615752267715 ) ) ;
#444 = CARTESIAN_POINT ( 'NONE',  ( 4.944772684328679446, 43.18518628210144072, -11.48171059495397373 ) ) ;
#445 = CARTESIAN_POINT ( 'NONE',  ( -46.03794563604517265, 205.3262412349648116, 4.842901733360249317 ) ) ;
#446 = CARTESIAN_POINT ( 'NONE',  ( 20.28004929559795499, 210.7199507044251732, -5.999999999998712141 ) ) ;
#447 = CARTESIAN_POINT ( 'NONE',  ( -64.64211230271182274, 203.5309553116391612, 1.857196546604092280 ) ) ;
#448 = CARTESIAN_POINT ( 'NONE',  ( 24.82458453031440726, 0.000000000000000000, 162.5574806918533000 ) ) ;
#449 = CARTESIAN_POINT ( 'NONE',  ( -11.48171059495408208, 107.1148137178985564, 4.944772684328421875 ) ) ;
#450 = CARTESIAN_POINT ( 'NONE',  ( -63.26413769728823411, 212.1499508600178387, 3.954877714930865817 ) ) ;
#451 = CARTESIAN_POINT ( 'NONE',  ( -32.38913769728823411, 205.8500491399820760, -7.418979330068584233 ) ) ;
#452 = CARTESIAN_POINT ( 'NONE',  ( 23.87821517812499650, 4.985214923628404904, -6.703124999385495997 ) ) ;
#453 = LINE ( 'NONE', #37417, #32490 ) ;
#454 = CARTESIAN_POINT ( 'NONE',  ( -14.38691631536193860, 71.46481371789856496, -5.770363421894132649 ) ) ;
#455 = CARTESIAN_POINT ( 'NONE',  ( -56.72544563604517265, 216.3070033484980854, 6.137860380172893926 ) ) ;
#456 = VERTEX_POINT ( 'NONE', #12456 ) ;
#457 = CARTESIAN_POINT ( 'NONE',  ( 10.56230152254384080, 3.464101615137603396, -9.937499999999992895 ) ) ;
#458 = CARTESIAN_POINT ( 'NONE',  ( 11.48171059495397728, 109.8851862821014436, 4.944772684328674117 ) ) ;
#459 = CARTESIAN_POINT ( 'NONE',  ( -15.53471296425195369, 49.22268628210144215, 2.908627838312118019 ) ) ;
#460 = CARTESIAN_POINT ( 'NONE',  ( 20.99999999999999645, 6.928203230275506996, -5.906249998770958243 ) ) ;
#461 = CARTESIAN_POINT ( 'NONE',  ( 33.74088742350031822, -5.407089921784861808, 159.8105457733328478 ) ) ;
#462 = CIRCLE ( 'NONE', #24693, 2.649999999999992806 ) ;
#463 = CARTESIAN_POINT ( 'NONE',  ( 15.53471296425195369, 63.02268628210144641, -2.908627838312120684 ) ) ;
#464 = DIRECTION ( 'NONE',  ( 0.000000000000000000, 0.000000000000000000, 1.000000000000000000 ) ) ;
#465 = CARTESIAN_POINT ( 'NONE',  ( 10.31873187879411091, -3.604726614523240613, -8.653124999385532590 ) ) ;
#466 = DIRECTION ( 'NONE',  ( 0.000000000000000000, 0.000000000000000000, 1.000000000000000000 ) ) ;
#467 = CARTESIAN_POINT ( 'NONE',  ( -46.83705436395489841, 205.3262412349647263, -4.842901733360204020 ) ) ;
#468 = CARTESIAN_POINT ( 'NONE',  ( -54.50000000000000711, 244.5000000000000000, 5.000000000000000000 ) ) ;
#469 = CARTESIAN_POINT ( 'NONE',  ( 2.660918448318279950, 42.89768628210143930, -12.46528703574805697 ) ) ;
#470 = CARTESIAN_POINT ( 'NONE',  ( 37.03711979530484655, 3.464101615138000856, 164.4628385719782955 ) ) ;
#471 = CARTESIAN_POINT ( 'NONE',  ( -3.474262827703337830, 5.235186282101429001, -8.843639120294326972 ) ) ;
#472 = CARTESIAN_POINT ( 'NONE',  ( 26.75643035624999655, 245.6218750006145513, -3.323476615752271268 ) ) ;
#473 = ORIENTED_EDGE ( 'NONE', *, *, #4147, .F. ) ;
#474 = CARTESIAN_POINT ( 'NONE',  ( 18.00000000000000000, 5.196152422706630247, -8.174999999999988276 ) ) ;
#476 = CYLINDRICAL_SURFACE ( 'NONE', #30001, 5.999999999999994671 ) ;
#475 = PRODUCT_DEFINITION_SHAPE ( 'NONE', 'NONE',  #37510 ) ;
#477 = LINE ( 'NONE', #26256, #35797 ) ;
#478 = CARTESIAN_POINT ( 'NONE',  ( 10.31873187879411091, -3.604726614523240613, -5.053124999385533833 ) ) ;
#479 = CARTESIAN_POINT ( 'NONE',  ( 28.14696362483655889, -5.407089921784859143, 167.5086318987019069 ) ) ;
#480 = CARTESIAN_POINT ( 'NONE',  ( 15.00000000000000000, 241.4124999999999943, -3.464101615137752166 ) ) ;
#481 = CARTESIAN_POINT ( 'NONE',  ( -1.909035429704832693E-15, 199.8875000000000171, -31.17691453623979214 ) ) ;
#482 = CARTESIAN_POINT ( 'NONE',  ( -2.311890736173176641, 42.32268628210145067, -12.53471296425194659 ) ) ;
#483 = VERTEX_POINT ( 'NONE', #17594 ) ;
#484 = AXIS2_PLACEMENT_3D ( 'NONE', #11652, #17544, #9193 ) ;
#485 = ORIENTED_EDGE ( 'NONE', *, *, #35805, .T. ) ;
#486 = DIRECTION ( 'NONE',  ( 0.000000000000000000, 0.000000000000000000, 1.000000000000000000 ) ) ;
#487 = CARTESIAN_POINT ( 'NONE',  ( 26.99999999999999645, 7.347880794884117764E-16, -3.318749998770964549 ) ) ;
#488 = CARTESIAN_POINT ( 'NONE',  ( 23.99999999999999645, 243.1000000000000227, -5.196152422706631135 ) ) ;
#489 = CARTESIAN_POINT ( 'NONE',  ( 23.87821517812500005, -4.985214923628404016, -6.290624999385458160 ) ) ;
#490 = CARTESIAN_POINT ( 'NONE',  ( 4.622313124798573369, 101.8351862821014464, 11.61527771782819940 ) ) ;
#491 = CARTESIAN_POINT ( 'NONE',  ( -8.927990412390371944, 17.12731371789855217, -13.04141134922778988 ) ) ;
#492 = CARTESIAN_POINT ( 'NONE',  ( 36.99463137071579411, 7.347880794884117764E-16, 163.9771936566585566 ) ) ;
#493 = CARTESIAN_POINT ( 'NONE',  ( 26.75643035624999655, 241.4968750006145228, 3.323476615752267715 ) ) ;
#494 = CARTESIAN_POINT ( 'NONE',  ( -33.18080436395489841, 205.4999999999999716, -0.1155267958017894420 ) ) ;
#495 = DIRECTION ( 'NONE',  ( 1.000000000000000000, 0.000000000000000000, 0.000000000000000000 ) ) ;
#496 = CARTESIAN_POINT ( 'NONE',  ( 25.41615413421409642, -3.464101615137757051, 169.3191522051509992 ) ) ;
#497 = CARTESIAN_POINT ( 'NONE',  ( -9.500000000000005329, 15.68981371789854329, 0.1745138560723101806 ) ) ;
#498 = CARTESIAN_POINT ( 'NONE',  ( -65.44122103062157692, 208.3738570449993404, -6.530955311639226935 ) ) ;
#499 = CARTESIAN_POINT ( 'NONE',  ( -35.35044563604517265, 203.6929966515019430, -6.137860380172892150 ) ) ;
#500 = CARTESIAN_POINT ( 'NONE',  ( 0.000000000000000000, 0.000000000000000000, 0.000000000000000000 ) ) ;
#501 = CARTESIAN_POINT ( 'NONE',  ( 22.56230152254543597, 3.464101615136989665, -4.574999998771033916 ) ) ;
#502 = CARTESIAN_POINT ( 'NONE',  ( 27.24356964374999635, 196.0718750006145683, -15.72908226750539029 ) ) ;
#503 = CARTESIAN_POINT ( 'NONE',  ( -0.1745138560722442889, 128.3898137178985621, -15.50000000000000533 ) ) ;
#504 = CARTESIAN_POINT ( 'NONE',  ( -52.37127896937850124, 216.5309553116391612, 1.626142955000506873 ) ) ;
#505 = EDGE_LOOP ( 'NONE', ( #36598, #28782, #25690, #21960 ) ) ;
#506 = CARTESIAN_POINT ( 'NONE',  ( -10.49813415415989581, 50.37268628210145494, -7.228626920339068285 ) ) ;
#507 = CARTESIAN_POINT ( 'NONE',  ( -47.00000000000000711, 244.5000000000000000, 5.000000000000000000 ) ) ;
#508 = CARTESIAN_POINT ( 'NONE',  ( 37.44889919624123564, 3.604726614523243278, 166.3748504141385922 ) ) ;
#509 = CARTESIAN_POINT ( 'NONE',  ( 15.00000000000000000, 3.464101615137752166, -2.231249998770934884 ) ) ;
#510 = CARTESIAN_POINT ( 'NONE',  ( 13.44051670066911441, -5.407089921784859143, -1.865624999385528948 ) ) ;
#511 =( BOUNDED_CURVE ( )  B_SPLINE_CURVE ( 2, ( #32601, #35627, #6825, #12519, #18216, #9301, #29756, #1322, #32976, #12324, #3608, #27109, #24272, #35815, #30140, #26534, #15740, #564, #35248, #20873, #32412, #6454, #18026, #30707, #4726, #36373, #1507, #16302, #27480, #16490, #19157, #25003, #21994, #1694, #2070, #4909, #7769, #10976, #19347, #30522, #36559, #10419, #13082, #13268, #27849, #10231, #24636, #28038, #30328, #8146, #13644, #36187, #22180, #31076, #30886, #25197, #2254, #36750, #10790, #33727, #33359, #4541, #7394, #10600, #21806, #22364, #1882, #33912, #33541, #4352, #22547, #18967, #7954, #19529, #5099, #16678, #34096, #28225, #7581, #15932, #13453, #25379, #13833, #16118, #27669, #36929, #24820, #339, #20454, #34647, #20266, #34468, #5842, #5284, #28584, #37482, #8511, #14381, #6025, #22737, #2998, #20077, #34286, #23291, #19718, #14568, #31805, #8330, #16864, #8692, #37302, #19900, #17420, #11904, #23104, #5463, #28960, #35024, #11533, #34836, #31258, #2811, #31441, #17611, #28401, #17046, #14198, #26120, #25939, #31622, #2622 ),
 .UNSPECIFIED., .F., .F. ) 
 B_SPLINE_CURVE_WITH_KNOTS ( ( 3, 2, 2, 2, 2, 2, 2, 2, 2, 2, 2, 2, 2, 2, 2, 2, 2, 2, 2, 2, 2, 2, 2, 2, 2, 2, 2, 2, 2, 2, 2, 2, 2, 2, 2, 2, 2, 2, 2, 2, 2, 2, 2, 2, 2, 2, 2, 2, 2, 2, 2, 2, 2, 2, 2, 2, 2, 2, 2, 2, 2, 2, 2, 2, 2, 3 ),
 ( 0.000000000000000000, 0.01388888888888888812, 0.02777777777777777624, 0.04166666666666666435, 0.05555555555555555247, 0.06944444444444444753, 0.08333333333333332871, 0.09722222222222222376, 0.1111111111111111049, 0.1250000000000000000, 0.1388888888888888951, 0.1527777777777777901, 0.1666666666666666574, 0.1805555555555555525, 0.1944444444444444475, 0.2083333333333333426, 0.2222222222222222099, 0.2361111111111111049, 0.2500000000000000000, 0.2638888888888888951, 0.2777777777777777901, 0.2916666666666666852, 0.3055555555555555802, 0.3194444444444444198, 0.3333333333333333148, 0.3472222222222222099, 0.3611111111111111049, 0.3750000000000000000, 0.3888888888888888951, 0.4027777777777777901, 0.4166666666666666852, 0.4305555555555555802, 0.4444444444444444198, 0.4583333333333333148, 0.4722222222222222099, 0.4861111111111111049, 0.5000000000000000000, 0.5138888888888888395, 0.5277777777777777901, 0.5416666666666666297, 0.5555555555555555802, 0.5694444444444444198, 0.5833333333333333703, 0.5972222222222222099, 0.6111111111111111605, 0.6250000000000000000, 0.6388888888888888395, 0.6527777777777777901, 0.6666666666666666297, 0.6805555555555555802, 0.6944444444444444198, 0.7083333333333333703, 0.7222222222222222099, 0.7361111111111111605, 0.7500000000000000000, 0.7638888888888888395, 0.7777777777777777901, 0.7916666666666666297, 0.8055555555555555802, 0.8194444444444444198, 0.8333333333333333703, 0.8472222222222222099, 0.8611111111111111605, 0.8750000000000000000, 0.8888888888888888395, 0.8996968925187518451 ),
 .UNSPECIFIED. ) 
 CURVE ( )  GEOMETRIC_REPRESENTATION_ITEM ( )  RATIONAL_B_SPLINE_CURVE ( ( 1.000000000000000000, 0.8660254037844387076, 1.000000000000000000, 0.8660254037844387076, 1.000000000000000000, 0.8660254037844387076, 1.000000000000000000, 0.8660254037844387076, 1.000000000000000000, 0.8660254037844387076, 1.000000000000000000, 0.8660254037844387076, 1.000000000000000000, 0.8660254037844387076, 1.000000000000000000, 0.8660254037844387076, 1.000000000000000000, 0.8660254037844387076, 1.000000000000000000, 0.8660254037844387076, 1.000000000000000000, 0.8660254037844387076, 1.000000000000000000, 0.8660254037844387076, 1.000000000000000000, 0.8660254037844387076, 1.000000000000000000, 0.8660254037844387076, 1.000000000000000000, 0.8660254037844387076, 1.000000000000000000, 0.8660254037844387076, 1.000000000000000000, 0.8660254037844387076, 1.000000000000000000, 0.8660254037844387076, 1.000000000000000000, 0.8660254037844387076, 1.000000000000000000, 0.8660254037844387076, 1.000000000000000000, 0.8660254037844387076, 1.000000000000000000, 0.8660254037844387076, 1.000000000000000000, 0.8660254037844387076, 1.000000000000000000, 0.8660254037844387076, 1.000000000000000000, 0.8660254037844387076, 1.000000000000000000, 0.8660254037844387076, 1.000000000000000000, 0.8660254037844387076, 1.000000000000000000, 0.8660254037844387076, 1.000000000000000000, 0.8660254037844387076, 1.000000000000000000, 0.8660254037844387076, 1.000000000000000000, 0.8660254037844387076, 1.000000000000000000, 0.8660254037844387076, 1.000000000000000000, 0.8660254037844387076, 1.000000000000000000, 0.8660254037844387076, 1.000000000000000000, 0.8660254037844387076, 1.000000000000000000, 0.8660254037844387076, 1.000000000000000000, 0.8660254037844387076, 1.000000000000000000, 0.8660254037844387076, 1.000000000000000000, 0.8660254037844387076, 1.000000000000000000, 0.8660254037844387076, 1.000000000000000000, 0.8660254037844387076, 1.000000000000000000, 0.8660254037844387076, 1.000000000000000000, 0.8660254037844387076, 1.000000000000000000, 0.8660254037844387076, 1.000000000000000000, 0.8660254037844387076, 1.000000000000000000, 0.8660254037844387076, 1.000000000000000000, 0.8660254037844387076, 1.000000000000000000, 0.8660254037844387076, 1.000000000000000000, 0.8660254037844387076, 1.000000000000000000, 0.8660254037844387076, 1.000000000000000000, 0.8660254037844387076, 1.000000000000000000, 0.8660254037844387076, 1.000000000000000000, 0.8660254037844387076, 1.000000000000000000, 0.8660254037844387076, 1.000000000000000000, 0.8660254037844387076, 1.000000000000000000, 0.8660254037844387076, 1.000000000000000000, 0.8660254037844387076, 1.000000000000000000, 0.8660254037844387076, 1.000000000000000000, 0.8660254037844387076, 1.000000000000000000, 0.8660254037844387076, 1.000000000000000000, 0.8660254037844387076, 1.000000000000000000, 0.8660254037844387076, 1.000000000000000000, 0.8660254037844387076, 1.000000000000000000, 0.8660254037844387076, 1.000000000000000000, 0.8957441496010808413, 0.9537471549767810863 ) ) 
 REPRESENTATION_ITEM ( '' )  );
#512 = CARTESIAN_POINT ( 'NONE',  ( 5.233372021372432847, 64.74768628210144072, 8.152565276336710909 ) ) ;
#513 = DIRECTION ( 'NONE',  ( -0.8083506638593008775, -0.5887012860850803220, 0.000000000000000000 ) ) ;
#514 = DIRECTION ( 'NONE',  ( 1.000000000000000000, 0.000000000000000000, -0.000000000000000000 ) ) ;
#515 = CARTESIAN_POINT ( 'NONE',  ( -10.49813415415989581, 87.17268628210143788, -7.228626920339068285 ) ) ;
#516 = CARTESIAN_POINT ( 'NONE',  ( 7.234628195640312676, 199.5299038117966859, -27.00000000000000711 ) ) ;
#517 = CARTESIAN_POINT ( 'NONE',  ( 24.78536444607796341, 0.000000000000000000, 162.1091930777120069 ) ) ;
#518 = ORIENTED_EDGE ( 'NONE', *, *, #17390, .F. ) ;
#519 = CARTESIAN_POINT ( 'NONE',  ( 30.61300606342343755, 7.209453229046475009, 159.8771620917002565 ) ) ;
#520 = CARTESIAN_POINT ( 'NONE',  ( 26.75643035624999655, 7.049594010296217766E-16, -9.815624999385457627 ) ) ;
#521 = CARTESIAN_POINT ( 'NONE',  ( 1.120210788295102201E-13, 195.5000000012290400, -27.00000000000000711 ) ) ;
#522 = CARTESIAN_POINT ( 'NONE',  ( 37.33123894353190764, 3.604726614523243278, 165.0299875717147131 ) ) ;
#523 = CARTESIAN_POINT ( 'NONE',  ( 30.89980292934887629, 6.928203230275514990, 163.1552652694962546 ) ) ;
#524 = FACE_OUTER_BOUND ( 'NONE', #7081, .T. ) ;
#525 = CARTESIAN_POINT ( 'NONE',  ( 23.99999999999999645, 248.0499999999999829, -5.196152422706631135 ) ) ;
#526 = CARTESIAN_POINT ( 'NONE',  ( 27.24356964374999279, 197.3656250006145285, -15.72908226750539207 ) ) ;
#527 = CARTESIAN_POINT ( 'NONE',  ( 8.715434833792128799, 101.9398137178985593, -8.962234695871567070 ) ) ;
#528 = CARTESIAN_POINT ( 'NONE',  ( 7.228626920339069173, 126.2726862821014322, -10.49813415415989404 ) ) ;
#530 = ORIENTED_EDGE ( 'NONE', *, *, #7271, .T. ) ;
#529 = VERTEX_POINT ( 'NONE', #35570 ) ;
#531 = CARTESIAN_POINT ( 'NONE',  ( 13.62178482187501416, 195.0031250006145456, 23.59362340125806767 ) ) ;
#532 = CARTESIAN_POINT ( 'NONE',  ( 26.75643035624999655, 240.1093750006145342, -3.323476615752271712 ) ) ;
#533 = CARTESIAN_POINT ( 'NONE',  ( 15.46528703574811736, 84.40231371789855075, -3.257655550456947768 ) ) ;
#534 = EDGE_CURVE ( 'NONE', #28874, #27232, #3235, .T. ) ;
#535 = CARTESIAN_POINT ( 'NONE',  ( 18.12178482187499640, 4.985214923628404904, -4.828124999385480010 ) ) ;
#536 = CARTESIAN_POINT ( 'NONE',  ( 15.24356964374999990, 247.1218750006145228, -3.323476615752268604 ) ) ;
#537 =( BOUNDED_CURVE ( )  B_SPLINE_CURVE ( 2, ( #9361, #68, #20936, #11634, #17898, #12007, #35307 ),
 .UNSPECIFIED., .F., .F. ) 
 B_SPLINE_CURVE_WITH_KNOTS ( ( 3, 2, 2, 3 ),
 ( 0.5652173913043500031, 0.5724637681159433500, 0.5797101449275368079, 0.5869565217391301548 ),
 .UNSPECIFIED. ) 
 CURVE ( )  GEOMETRIC_REPRESENTATION_ITEM ( )  RATIONAL_B_SPLINE_CURVE ( ( 0.9999999999999589217, 0.8660254037844797859, 1.000000000000000000, 0.8660254037844387076, 1.000000000000000000, 0.8660254037844448138, 0.9999999999999938938 ) ) 
 REPRESENTATION_ITEM ( '' )  );
#538 = CARTESIAN_POINT ( 'NONE',  ( -6.840914352312096547, 94.36018628210146630, 6.594114490232313663 ) ) ;
#539 = CARTESIAN_POINT ( 'NONE',  ( 13.50000000000001421, 197.1125000012290513, 23.38268590217984055 ) ) ;
#540 = CARTESIAN_POINT ( 'NONE',  ( 9.465287035748106703, 75.20231371789854791, -2.064181346179063237 ) ) ;
#541 = CARTESIAN_POINT ( 'NONE',  ( 10.31873187879411269, -3.604726614523240613, -4.603124999385506122 ) ) ;
#542 = CARTESIAN_POINT ( 'NONE',  ( 26.75643035624999655, 241.0093750006145115, -3.323476615752271268 ) ) ;
#543 = CARTESIAN_POINT ( 'NONE',  ( 8.715434833792128799, 46.73981371789854933, -8.962234695871567070 ) ) ;
#544 = CARTESIAN_POINT ( 'NONE',  ( 31.20375858228842603, -6.928203230275506996, 166.6294942803155550 ) ) ;
#545 = CARTESIAN_POINT ( 'NONE',  ( 8.962234695871762469, 108.1601862821014635, -8.715434833791931624 ) ) ;
#546 = CARTESIAN_POINT ( 'NONE',  ( 13.56230152254410548, 5.196152422706630247, -5.812499998771008869 ) ) ;
#547 = EDGE_CURVE ( 'NONE', #14469, #8607, #31068, .T. ) ;
#548 = CARTESIAN_POINT ( 'NONE',  ( -33.57663769728823411, 204.3130714775002730, 3.149950860017883603 ) ) ;
#549 = CYLINDRICAL_SURFACE ( 'NONE', #10694, 27.00000000000000000 ) ;
#550 = CARTESIAN_POINT ( 'NONE',  ( 30.88754665307854097, 7.209453229046475009, 163.0151753906892793 ) ) ;
#551 = CARTESIAN_POINT ( 'NONE',  ( -15.53471296425195369, 76.82268628210144357, 2.908627838312118019 ) ) ;
#552 = CARTESIAN_POINT ( 'NONE',  ( 26.99999999999999645, 248.4250000000000114, -7.347880794884117764E-16 ) ) ;
#553 = DIRECTION ( 'NONE',  ( 1.000000000000000000, 0.000000000000000000, 0.000000000000000000 ) ) ;
#554 = CARTESIAN_POINT ( 'NONE',  ( 15.00000000000000000, 0.000000000000000000, 0.000000000000000000 ) ) ;
#555 = CARTESIAN_POINT ( 'NONE',  ( -1.715153634034234598, 106.7226862821014635, -9.534712964251941258 ) ) ;
#556 = CARTESIAN_POINT ( 'NONE',  ( 19.39230484541326049, 247.7138461906614282, -5.999999999999994671 ) ) ;
#557 = ADVANCED_FACE ( 'NONE', ( #3167 ), #20623, .F. ) ;
#558 = CARTESIAN_POINT ( 'NONE',  ( -15.50000000000000533, 12.71018628210143753, -0.1745138560725808530 ) ) ;
#559 = CARTESIAN_POINT ( 'NONE',  ( -27.24356964374999635, 195.8468750006145171, 15.72908226750539384 ) ) ;
#560 = CARTESIAN_POINT ( 'NONE',  ( 21.00000000000000000, 242.8843750006145399, -6.646953231504538984 ) ) ;
#561 = ORIENTED_EDGE ( 'NONE', *, *, #19014, .T. ) ;
#562 = CARTESIAN_POINT ( 'NONE',  ( 37.52570519453759346, -3.604726614523235284, 167.2527469918319412 ) ) ;
#563 = CARTESIAN_POINT ( 'NONE',  ( 21.00000000000000000, 243.8687500012290172, 5.999999999999998224 ) ) ;
#564 = CARTESIAN_POINT ( 'NONE',  ( 27.24356964374999279, 199.2218750006145171, -15.72908226750539207 ) ) ;
#565 = CARTESIAN_POINT ( 'NONE',  ( 26.99999999999999645, 7.347880794884117764E-16, -4.668749998770954868 ) ) ;
#566 = FACE_OUTER_BOUND ( 'NONE', #21711, .T. ) ;
#567 = DIRECTION ( 'NONE',  ( -0.000000000000000000, 1.000000000000000000, -0.000000000000000000 ) ) ;
#568 = CARTESIAN_POINT ( 'NONE',  ( 22.80587116629411071, 3.604726614523238837, -0.7781249993855585689 ) ) ;
#569 = CARTESIAN_POINT ( 'NONE',  ( -8.152565276336593669, 16.55231371789855643, -5.233372021372610483 ) ) ;
#570 = CARTESIAN_POINT ( 'NONE',  ( -27.24356964375000345, 198.9218750006145626, -15.72908226750537786 ) ) ;
#571 = ORIENTED_EDGE ( 'NONE', *, *, #36630, .T. ) ;
#572 = CARTESIAN_POINT ( 'NONE',  ( 21.00000000000000000, 249.6343750006145399, -6.646953231504538984 ) ) ;
#573 = CARTESIAN_POINT ( 'NONE',  ( 10.49813415416005213, 47.02731371789855075, -7.228626920338837358 ) ) ;
#574 = CARTESIAN_POINT ( 'NONE',  ( 21.00000000000000000, 6.646953231504538984, -1.603124999385459937 ) ) ;
#575 = CARTESIAN_POINT ( 'NONE',  ( -8.962234695871565293, 7.639813717898541690, -8.715434833792128799 ) ) ;
#576 = CARTESIAN_POINT ( 'NONE',  ( 26.99999999999999645, 248.0124999999999602, -3.464101615137755275 ) ) ;
#577 = EDGE_LOOP ( 'NONE', ( #17705, #26737, #27106, #20978 ) ) ;
#578 = CARTESIAN_POINT ( 'NONE',  ( 22.80587116629412492, 3.604726614523243278, -3.984374999385507987 ) ) ;
#579 = EDGE_LOOP ( 'NONE', ( #18982, #34697, #20451, #16198 ) ) ;
#580 = CARTESIAN_POINT ( 'NONE',  ( -1.926257025242585782E-15, 199.2406250006145285, -31.45816453501075927 ) ) ;
#581 = EDGE_CURVE ( 'NONE', #7872, #24534, #12201, .T. ) ;
#582 = CARTESIAN_POINT ( 'NONE',  ( 27.85444716323975101, 5.407089921784862696, 164.1651534432314747 ) ) ;
#583 = CARTESIAN_POINT ( 'NONE',  ( -65.82961230271185116, 212.3930949314663792, 8.469044688360751749 ) ) ;
#584 = CARTESIAN_POINT ( 'NONE',  ( 20.99999999999999645, 248.5093750006144830, 6.646953231504538984 ) ) ;
#585 = CARTESIAN_POINT ( 'NONE',  ( 15.00000000000001954, 11.99999999999999822, 50.26196565745151190 ) ) ;
#586 = EDGE_CURVE ( 'NONE', #12855, #5744, #3208, .T. ) ;
#587 = CARTESIAN_POINT ( 'NONE',  ( -59.69419563604517265, 205.4999999999999716, 0.1155267958017633378 ) ) ;
#588 = CARTESIAN_POINT ( 'NONE',  ( 31.04687824534265417, -6.928203230275506996, 164.8363438237504113 ) ) ;
#589 = CARTESIAN_POINT ( 'NONE',  ( 27.99008328789078703, -5.407089921784859143, 165.7154814421367348 ) ) ;
#590 = VERTEX_POINT ( 'NONE', #13390 ) ;
#591 = CARTESIAN_POINT ( 'NONE',  ( 18.00000000000000355, 248.7249999999999943, 5.196152422706632912 ) ) ;
#592 = CARTESIAN_POINT ( 'NONE',  ( -8.927990412390371944, 7.927313717898536005, -13.04141134922778988 ) ) ;
#593 = CARTESIAN_POINT ( 'NONE',  ( -61.68080436395489841, 201.5000000000000000, -0.1155267958017054536 ) ) ;
#594 = EDGE_CURVE ( 'NONE', #25471, #14391, #18768, .T. ) ;
#595 = CARTESIAN_POINT ( 'NONE',  ( -8.843639120294326972, 131.7351862821014663, 3.474262827703335166 ) ) ;
#596 = LINE ( 'NONE', #9710, #21812 ) ;
#597 = CARTESIAN_POINT ( 'NONE',  ( -12.53471296425194836, 30.82268628210144001, 2.311890736173176641 ) ) ;
#598 = CARTESIAN_POINT ( 'NONE',  ( 13.56230152254411614, -5.196152422706638241, -5.775000000000085620 ) ) ;
#599 = ORIENTED_EDGE ( 'NONE', *, *, #8780, .T. ) ;
#600 = CARTESIAN_POINT ( 'NONE',  ( -35.75372103062156981, 216.5309553116392181, -1.626142955000564383 ) ) ;
#601 = CARTESIAN_POINT ( 'NONE',  ( -8.632099005475501130, 124.5476862821014663, -13.23911966647218996 ) ) ;
#602 = LINE ( 'NONE', #31703, #10891 ) ;
#603 = CARTESIAN_POINT ( 'NONE',  ( 9.500000000000005329, 139.8898137178985621, -0.1745138560723090149 ) ) ;
#604 = CARTESIAN_POINT ( 'NONE',  ( 27.24356964374999635, 195.6218750006145228, -15.72908226750539029 ) ) ;
#605 = CARTESIAN_POINT ( 'NONE',  ( 20.99999999999999645, 185.0294372515228645, 5.999999999999999112 ) ) ;
#606 = CARTESIAN_POINT ( 'NONE',  ( 22.56625951594015689, -0.6522502533381772105, -10.00000000000000000 ) ) ;
#607 = LINE ( 'NONE', #12176, #4334 ) ;
#608 = CARTESIAN_POINT ( 'NONE',  ( 20.99999999999999645, 0.000000000000000000, -8.000000000000000000 ) ) ;
#609 = CARTESIAN_POINT ( 'NONE',  ( 15.24356964374999990, 243.1093750006145342, 0.000000000000000000 ) ) ;
#610 = CARTESIAN_POINT ( 'NONE',  ( -9.465287035748106703, 98.20231371789854791, 2.064181346179061460 ) ) ;
#611 = CARTESIAN_POINT ( 'NONE',  ( 26.99999999999999645, 7.347880794884117764E-16, -4.668749998770954868 ) ) ;
#612 = ORIENTED_EDGE ( 'NONE', *, *, #9923, .T. ) ;
#613 = CARTESIAN_POINT ( 'NONE',  ( -50.59747103062156270, 213.3500491399821328, -5.571401726697985168 ) ) ;
#614 = CARTESIAN_POINT ( 'NONE',  ( 15.00000000000000000, 245.5562500012290457, 0.000000000000000000 ) ) ;
#615 = CARTESIAN_POINT ( 'NONE',  ( -2.311890736173447980, 105.6773137178985706, 12.53471296425189330 ) ) ;
#616 = CARTESIAN_POINT ( 'NONE',  ( 19.68408634441911431, 5.407089921784862696, -0.7968749993855217539 ) ) ;
#617 = CARTESIAN_POINT ( 'NONE',  ( 29.49486714975617474, 6.148716665048038266, 159.5363409456820136 ) ) ;
#618 =( BOUNDED_CURVE ( )  B_SPLINE_CURVE ( 2, ( #14056, #30566, #4584, #23146, #34688, #17273, #8919, #2664, #563 ),
 .UNSPECIFIED., .F., .F. ) 
 B_SPLINE_CURVE_WITH_KNOTS ( ( 3, 2, 2, 2, 3 ),
 ( 0.5326086956521739468, 0.5362318840579710644, 0.5434782608695651884, 0.5507246376811594235, 0.5543478260869565410 ),
 .UNSPECIFIED. ) 
 CURVE ( )  GEOMETRIC_REPRESENTATION_ITEM ( )  RATIONAL_B_SPLINE_CURVE ( ( 0.9330127018922194093, 0.9330127018922194093, 1.000000000000000000, 0.8660254037844387076, 1.000000000000000000, 0.8660254037844387076, 1.000000000000000000, 0.9330127018922194093, 0.9330127018922194093 ) ) 
 REPRESENTATION_ITEM ( '' )  );
#619 = CARTESIAN_POINT ( 'NONE',  ( 26.75643035624999655, -3.323476615752267715, -2.315624999385466509 ) ) ;
#620 = CARTESIAN_POINT ( 'NONE',  ( 4.622313124798831829, 73.76481371789856212, -11.61527771782809282 ) ) ;
#621 = CARTESIAN_POINT ( 'NONE',  ( 13.62178482187501416, 197.7593750006145399, 23.59362340125806767 ) ) ;
#622 = EDGE_LOOP ( 'NONE', ( #9730, #27726, #18131, #5252 ) ) ;
#623 = VECTOR ( 'NONE', #32641, 1000.000000000000000 ) ;
#624 = ORIENTED_EDGE ( 'NONE', *, *, #36236, .T. ) ;
#625 = CARTESIAN_POINT ( 'NONE',  ( 26.75643035624999655, -3.323476615752267271, -4.003124999385458516 ) ) ;
#626 = CARTESIAN_POINT ( 'NONE',  ( 24.65463083184878101, 3.464101615137419543, 160.6149010293500510 ) ) ;
#627 = CARTESIAN_POINT ( 'NONE',  ( 18.12178482187499640, 246.0718750006145115, -4.985214923628404904 ) ) ;
#628 = CARTESIAN_POINT ( 'NONE',  ( -2.660918448318275509, 38.29768628210145920, 12.46528703574805874 ) ) ;
#629 = EDGE_CURVE ( 'NONE', #9403, #23945, #16100, .T. ) ;
#630 = CARTESIAN_POINT ( 'NONE',  ( -52.37127896937850124, 216.5309553116392181, 1.626142955000506429 ) ) ;
#631 = PRESENTATION_STYLE_ASSIGNMENT (( #34575 ) ) ;
#632 = CARTESIAN_POINT ( 'NONE',  ( -65.03794563604516554, 205.3262412349647832, 4.842901733360250205 ) ) ;
#633 = CARTESIAN_POINT ( 'NONE',  ( 36.68087069682425039, 7.347880794884117764E-16, 160.3908927435282692 ) ) ;
#634 = CARTESIAN_POINT ( 'NONE',  ( 7.228626920338837358, 76.92731371789857064, 10.49813415416005036 ) ) ;
#635 = CARTESIAN_POINT ( 'NONE',  ( -66.03497103062157692, 206.1606490808709111, -2.350049139982163027 ) ) ;
#636 = CARTESIAN_POINT ( 'NONE',  ( -32.98288769728823411, 201.5309553116392181, -2.393094931466246855 ) ) ;
#637 =( BOUNDED_CURVE ( )  B_SPLINE_CURVE ( 2, ( #9247, #31797, #17784, #9061, #32362, #11896, #20632, #20820, #23284 ),
 .UNSPECIFIED., .F., .F. ) 
 B_SPLINE_CURVE_WITH_KNOTS ( ( 3, 2, 2, 2, 3 ),
 ( 0.4021739130434782705, 0.4057971014492753881, 0.4130434782608695676, 0.4202898550724637472, 0.4239130434782608647 ),
 .UNSPECIFIED. ) 
 CURVE ( )  GEOMETRIC_REPRESENTATION_ITEM ( )  RATIONAL_B_SPLINE_CURVE ( ( 0.9330127018922194093, 0.9330127018922194093, 1.000000000000000000, 0.8660254037844387076, 1.000000000000000000, 0.8660254037844387076, 1.000000000000000000, 0.9330127018922194093, 0.9330127018922194093 ) ) 
 REPRESENTATION_ITEM ( '' )  );
#638 = CARTESIAN_POINT ( 'NONE',  ( 15.24356964374999990, 0.000000000000000000, -6.553124999385484983 ) ) ;
#639 = CARTESIAN_POINT ( 'NONE',  ( 19.56230152254412147, 5.196152422706637353, -0.6000000000000171863 ) ) ;
#640 = CARTESIAN_POINT ( 'NONE',  ( -13.04141134922778456, 60.82731371789854080, 8.927990412390377273 ) ) ;
#641 = CARTESIAN_POINT ( 'NONE',  ( -53.75669563604516554, 209.8844732041981729, -8.500000000000003553 ) ) ;
#642 = CYLINDRICAL_SURFACE ( 'NONE', #12591, 4.899999999999999467 ) ;
#643 = CARTESIAN_POINT ( 'NONE',  ( -4.622313124798576922, 88.03518628210144925, -11.61527771782819762 ) ) ;
#644 = CARTESIAN_POINT ( 'NONE',  ( -13.04141134922759804, 41.17268628210143078, -8.927990412390657937 ) ) ;
#645 = CARTESIAN_POINT ( 'NONE',  ( 19.95811093400027403, 239.6067736145540152, -5.908846518073574750 ) ) ;
#646 = CARTESIAN_POINT ( 'NONE',  ( 36.81810950810510974, 7.646167579472024665E-16, 159.1648912866995715 ) ) ;
#647 = AXIS2_PLACEMENT_3D ( 'NONE', #18195, #29735, #18006 ) ;
#648 = CARTESIAN_POINT ( 'NONE',  ( -14.25334919248782306, 50.08518628210143930, -6.092822981423979378 ) ) ;
#649 = CARTESIAN_POINT ( 'NONE',  ( 21.00000000000001066, 247.0187500012290513, 5.999999999999998224 ) ) ;
#650 = CARTESIAN_POINT ( 'NONE',  ( 10.31873187879411091, -3.604726614523240613, -9.553124999385522287 ) ) ;
#651 = CARTESIAN_POINT ( 'NONE',  ( -70.80918835584510873, 215.2843023367891249, 3.000000000000000000 ) ) ;
#652 = CARTESIAN_POINT ( 'NONE',  ( -55.74330436395489841, 210.1155267958017134, -6.500000000000000888 ) ) ;
#653 = CARTESIAN_POINT ( 'NONE',  ( 20.99999999999995381, 241.1687500012290570, 5.999999999999998224 ) ) ;
#654 = CARTESIAN_POINT ( 'NONE',  ( 10.69584247140445221, 16.44768628210144001, -6.932735513423970097 ) ) ;
#655 = CARTESIAN_POINT ( 'NONE',  ( 2.064181346179061460, 141.9023137178985507, 9.465287035748106703 ) ) ;
#656 = CARTESIAN_POINT ( 'NONE',  ( 20.99999999999999645, 245.6968750006145399, -6.646953231504538984 ) ) ;
#657 = ORIENTED_EDGE ( 'NONE', *, *, #10356, .T. ) ;
#658 = CARTESIAN_POINT ( 'NONE',  ( 18.00000000000000355, -5.196152422706632912, -8.025000000000003908 ) ) ;
#659 = DIRECTION ( 'NONE',  ( 0.000000000000000000, 0.000000000000000000, -1.000000000000000000 ) ) ;
#660 = DIRECTION ( 'NONE',  ( 0.000000000000000000, 1.000000000000000000, 0.000000000000000000 ) ) ;
#661 = CARTESIAN_POINT ( 'NONE',  ( 13.44051670066911619, -5.407089921784859143, -5.015624999385570604 ) ) ;
#662 = CARTESIAN_POINT ( 'NONE',  ( 37.41458162253433528, 3.604726614523238837, 165.9825987517649253 ) ) ;
#663 = CARTESIAN_POINT ( 'NONE',  ( 21.00000000000000000, 241.1125000000000114, 6.928203230275506996 ) ) ;
#664 = EDGE_CURVE ( 'NONE', #25295, #10376, #15092, .T. ) ;
#665 = CARTESIAN_POINT ( 'NONE',  ( -13.50000000000000533, 199.9250000000000114, -23.38268590217984411 ) ) ;
#666 = CARTESIAN_POINT ( 'NONE',  ( 12.53471296425194659, 44.62268628210144783, -2.311890736173178418 ) ) ;
#667 = ORIENTED_EDGE ( 'NONE', *, *, #34152, .T. ) ;
#668 = EDGE_LOOP ( 'NONE', ( #20169, #31323 ) ) ;
#669 = CARTESIAN_POINT ( 'NONE',  ( 0.000000000000000000, 200.0000000000000000, -25.00000000000000000 ) ) ;
#670 = EDGE_CURVE ( 'NONE', #32512, #7058, #35888, .T. ) ;
#671 = CARTESIAN_POINT ( 'NONE',  ( 15.00000000000063771, -3.464101615138124757, -3.506249998770952558 ) ) ;
#672 = CARTESIAN_POINT ( 'NONE',  ( -13.50000000000000533, 198.2375000012290229, -23.38268590217984411 ) ) ;
#673 = CARTESIAN_POINT ( 'NONE',  ( 21.00000000000000000, 6.646953231504538984, -5.203124999385457805 ) ) ;
#674 = CARTESIAN_POINT ( 'NONE',  ( -7.228626920339069173, 103.2726862821014606, 10.49813415415989581 ) ) ;
#675 = CARTESIAN_POINT ( 'NONE',  ( 13.23911966647199812, 11.95231371789853902, 8.632099005475788900 ) ) ;
#676 = EDGE_CURVE ( 'NONE', #21562, #5473, #30076, .T. ) ;
#677 = CARTESIAN_POINT ( 'NONE',  ( 20.99999999999999289, 249.2125000000000057, 5.999999999999999112 ) ) ;
#678 = CARTESIAN_POINT ( 'NONE',  ( 28.18902776508177510, 5.196152422706636465, 166.5921030979066586 ) ) ;
#679 = VECTOR ( 'NONE', #1496, 1000.000000000000000 ) ;
#680 = CARTESIAN_POINT ( 'NONE',  ( -66.02752896937849414, 212.3500491399821613, 3.839350919129088435 ) ) ;
#681 = FACE_OUTER_BOUND ( 'NONE', #22092, .T. ) ;
#682 = CARTESIAN_POINT ( 'NONE',  ( 28.43415329166666083, 5.196152422706630247, 169.3939006875140194 ) ) ;
#683 = CARTESIAN_POINT ( 'NONE',  ( -8.843639120294245259, 7.064813717898548617, -3.474262827703533230 ) ) ;
#684 = CARTESIAN_POINT ( 'NONE',  ( -58.11830436395490551, 209.8844732041982581, 6.500000000000000888 ) ) ;
#685 = CARTESIAN_POINT ( 'NONE',  ( -66.82663769728823411, 202.5810206699313767, 4.149950860017909804 ) ) ;
#686 = DIRECTION ( 'NONE',  ( 1.000000000000000000, 0.000000000000000000, 0.000000000000000000 ) ) ;
#687 = CARTESIAN_POINT ( 'NONE',  ( 20.99999999999999645, -6.646953231504538984, -0.5906249993854775227 ) ) ;
#688 = CARTESIAN_POINT ( 'NONE',  ( -1.926257025242585782E-15, 198.3406250006145228, -31.45816453501075927 ) ) ;
#689 = CARTESIAN_POINT ( 'NONE',  ( -3.257655550456946880, 128.1023137178985678, -15.46528703574811736 ) ) ;
#690 = CARTESIAN_POINT ( 'NONE',  ( -63.05877896937850835, 211.6261429550004607, -6.530955311639245586 ) ) ;
#691 = ORIENTED_EDGE ( 'NONE', *, *, #2981, .T. ) ;
#692 = CARTESIAN_POINT ( 'NONE',  ( 0.1745138560725515708, 42.61018628210144499, -12.50000000000000355 ) ) ;
#693 = CARTESIAN_POINT ( 'NONE',  ( 18.00000000000000000, 244.5812500012290513, -5.196152422706630247 ) ) ;
#694 = CARTESIAN_POINT ( 'NONE',  ( 37.06326651802246630, 7.347880794884125653E-16, 164.7616969801814548 ) ) ;
#695 = CARTESIAN_POINT ( 'NONE',  ( 28.06362094583411704, -5.407089921784865361, 166.5560207186516664 ) ) ;
#696 = CARTESIAN_POINT ( 'NONE',  ( -15.53471296425195369, 95.22268628210143504, 2.908627838312118019 ) ) ;
#697 = CARTESIAN_POINT ( 'NONE',  ( -64.45163769728823411, 215.6869285224996986, -3.149950860017881382 ) ) ;
#698 = CARTESIAN_POINT ( 'NONE',  ( 19.68408634441910721, -5.407089921784855591, -1.790624999385564964 ) ) ;
#699 = CARTESIAN_POINT ( 'NONE',  ( 9.534712964251941258, 53.82268628210144357, -1.715153634034235708 ) ) ;
#700 = CARTESIAN_POINT ( 'NONE',  ( 20.99999999999999645, 250.0000000000000000, -5.999999999999999112 ) ) ;
#701 = DIRECTION ( 'NONE',  ( 0.5887012860850814322, -0.8083506638592999893, 0.000000000000000000 ) ) ;
#702 = CARTESIAN_POINT ( 'NONE',  ( -4.944772684328673229, 93.78518628210144925, 11.48171059495397728 ) ) ;
#703 = CARTESIAN_POINT ( 'NONE',  ( 36.95867962683190910, 3.464101615138031054, 163.5662633436957663 ) ) ;
#704 = CARTESIAN_POINT ( 'NONE',  ( -29.00000000000002487, 210.0000000000000000, 0.000000000000000000 ) ) ;
#705 = CYLINDRICAL_SURFACE ( 'NONE', #13506, 5.999999999999999112 ) ;
#706 = CARTESIAN_POINT ( 'NONE',  ( 27.54558899987776144, 5.407089921784856479, 160.6348884818688418 ) ) ;
#707 = CIRCLE ( 'NONE', #4958, 2.649999999999991029 ) ;
#708 = CARTESIAN_POINT ( 'NONE',  ( 21.00000000000000000, 6.928203230275506996, -0.5624999999999866773 ) ) ;
#709 = CARTESIAN_POINT ( 'NONE',  ( -49.64999999999999858, 244.5000000000000000, 5.000000000000000000 ) ) ;
#710 = CARTESIAN_POINT ( 'NONE',  ( 30.98069435314010178, -7.209453229046482114, 164.0798584742748290 ) ) ;
#711 = CARTESIAN_POINT ( 'NONE',  ( 31.03707322417642800, -6.928203230275514990, 164.7242719189907518 ) ) ;
#712 = CARTESIAN_POINT ( 'NONE',  ( 25.17756528844239483, 0.000000000000000000, 166.5920692191248804 ) ) ;
#713 = CARTESIAN_POINT ( 'NONE',  ( 26.99999999999999645, 247.9375000000000000, 3.464101615137751278 ) ) ;
#714 = CARTESIAN_POINT ( 'NONE',  ( 13.62178482187499640, 195.6031250006145115, -23.59362340125807123 ) ) ;
#715 = CARTESIAN_POINT ( 'NONE',  ( -8.715434833792127023, 106.5398137178985536, 8.962234695871568846 ) ) ;
#716 = CARTESIAN_POINT ( 'NONE',  ( 4.944772684328679446, 107.5851862821014464, -11.48171059495397373 ) ) ;
#717 = VERTEX_POINT ( 'NONE', #4111 ) ;
#718 = CARTESIAN_POINT ( 'NONE',  ( -27.24356964374999635, 196.6906250006145456, 15.72908226750539384 ) ) ;
#719 = CARTESIAN_POINT ( 'NONE',  ( 19.00081547855239350, 239.7604221912915818, -5.492723509887031952 ) ) ;
#720 = CARTESIAN_POINT ( 'NONE',  ( -15.46528703574811736, 70.60231371789853938, 3.257655550456946436 ) ) ;
#721 = CARTESIAN_POINT ( 'NONE',  ( 26.75643035624999655, 7.049594010296217766E-16, -4.528124999385485516 ) ) ;
#722 = CARTESIAN_POINT ( 'NONE',  ( 23.87821517812499650, 248.8093750006145228, -4.985214923628404904 ) ) ;
#723 = CARTESIAN_POINT ( 'NONE',  ( 7.954856959092191815, 91.77268628210144641, 5.529263428287477744 ) ) ;
#724 = AXIS2_PLACEMENT_3D ( 'NONE', #30085, #15119, #33117 ) ;
#725 = CARTESIAN_POINT ( 'NONE',  ( 13.49999999999999645, 195.0125000012290570, -23.38268590217984766 ) ) ;
#726 = CARTESIAN_POINT ( 'NONE',  ( 3.474262827703532341, 82.96481371789856496, -8.843639120294245259 ) ) ;
#727 = CARTESIAN_POINT ( 'NONE',  ( 22.80587116629410716, 7.646167579472015790E-16, -5.765624999385543958 ) ) ;
#728 = EDGE_CURVE ( 'NONE', #34798, #36105, #17305, .T. ) ;
#729 = CARTESIAN_POINT ( 'NONE',  ( -8.710071997420207879, 107.1148137178985564, 3.796722387233182339 ) ) ;
#730 = CARTESIAN_POINT ( 'NONE',  ( 20.99999999999999645, 241.5343750006145171, -6.646953231504538984 ) ) ;
#731 = CARTESIAN_POINT ( 'NONE',  ( -11.48171059495408208, 51.91481371789855359, 4.944772684328421875 ) ) ;
#732 = LINE ( 'NONE', #35796, #24881 ) ;
#733 =( BOUNDED_CURVE ( )  B_SPLINE_CURVE ( 2, ( #32456, #15221, #12753, #23751, #29425, #29803, #21299 ),
 .UNSPECIFIED., .F., .F. ) 
 B_SPLINE_CURVE_WITH_KNOTS ( ( 3, 2, 2, 3 ),
 ( 0.6956521739130425708, 0.7028985507246365838, 0.7101449275362307079, 0.7173913043478246099 ),
 .UNSPECIFIED. ) 
 CURVE ( )  GEOMETRIC_REPRESENTATION_ITEM ( )  RATIONAL_B_SPLINE_CURVE ( ( 1.000000000000016431, 0.8660254037844222763, 1.000000000000000000, 0.8660254037844387076, 1.000000000000000000, 0.8660254037844653530, 0.9999999999999733546 ) ) 
 REPRESENTATION_ITEM ( '' )  );
#734 = CARTESIAN_POINT ( 'NONE',  ( 8.962234695871762469, 98.96018628210146062, -8.715434833791931624 ) ) ;
#735 = CARTESIAN_POINT ( 'NONE',  ( 16.56230152254410726, -6.928203230275506996, -5.624999998770996434 ) ) ;
#736 = CARTESIAN_POINT ( 'NONE',  ( -68.21205436395490551, 213.2096571498974242, 3.378800118222489601 ) ) ;
#737 = CARTESIAN_POINT ( 'NONE',  ( 7.228626920339068285, 135.4726862821014493, -10.49813415415989581 ) ) ;
#738 = CARTESIAN_POINT ( 'NONE',  ( 30.90715669519676467, -7.209453229046475009, 163.2393191977598974 ) ) ;
#739 = CARTESIAN_POINT ( 'NONE',  ( 8.632099005475504683, 73.94768628210142936, 13.23911966647218996 ) ) ;
#740 = CARTESIAN_POINT ( 'NONE',  ( 19.68408634441911786, -5.407089921784861808, -4.996874999385530813 ) ) ;
#741 = CARTESIAN_POINT ( 'NONE',  ( 26.99999999999999645, 248.4625000000000057, -3.464101615137755275 ) ) ;
#742 = CARTESIAN_POINT ( 'NONE',  ( 22.56230152254410015, 7.347880794884117764E-16, -7.312499998771010645 ) ) ;
#743 = DIRECTION ( 'NONE',  ( -0.000000000000000000, -0.000000000000000000, -1.000000000000000000 ) ) ;
#744 = CARTESIAN_POINT ( 'NONE',  ( 0.1745138560725194299, 116.2101862821014748, -9.500000000000005329 ) ) ;
#745 = CARTESIAN_POINT ( 'NONE',  ( -44.35000000000001563, 244.5000000000000000, 5.000000000000000000 ) ) ;
#746 = EDGE_CURVE ( 'NONE', #7363, #18087, #6969, .T. ) ;
#747 = CARTESIAN_POINT ( 'NONE',  ( -2.908627838312119351, 5.522686282101450850, -15.53471296425195369 ) ) ;
#748 = CARTESIAN_POINT ( 'NONE',  ( 27.24356964375000345, 196.4843750006145626, -3.336375036156643733E-15 ) ) ;
#749 = CARTESIAN_POINT ( 'NONE',  ( 21.00000000000000000, 243.3343750006145285, -6.646953231504538984 ) ) ;
#750 = ORIENTED_EDGE ( 'NONE', *, *, #22577, .F. ) ;
#751 = EDGE_CURVE ( 'NONE', #37490, #27706, #21564, .T. ) ;
#752 = CARTESIAN_POINT ( 'NONE',  ( 28.14696362483655889, -5.407089921784859143, 167.5086318987019069 ) ) ;
#753 = CARTESIAN_POINT ( 'NONE',  ( 21.00000000000000000, -6.646953231504538984, -3.628124999385489158 ) ) ;
#754 = CARTESIAN_POINT ( 'NONE',  ( 16.56230152254411436, -6.928203230275514990, -4.837499999999994138 ) ) ;
#755 = CARTESIAN_POINT ( 'NONE',  ( 15.02283181144952628, 7.347880794884122694E-16, 50.52293445648592751 ) ) ;
#756 = CARTESIAN_POINT ( 'NONE',  ( 22.56230152254500254, 3.464101615137234358, -5.924999998771016685 ) ) ;
#757 = CARTESIAN_POINT ( 'NONE',  ( 20.99999999999999645, -6.928203230275506996, -7.481249998770959309 ) ) ;
#758 = AXIS2_PLACEMENT_3D ( 'NONE', #36466, #33265, #18505 ) ;
#759 = CARTESIAN_POINT ( 'NONE',  ( 0.000000000000000000, 200.0000000000000000, 0.000000000000000000 ) ) ;
#760 = CARTESIAN_POINT ( 'NONE',  ( -8.843639120294245259, 25.46481371789855075, -3.474262827703533230 ) ) ;
#761 = CARTESIAN_POINT ( 'NONE',  ( -13.62178482187498396, 196.7843750006145456, 23.59362340125808188 ) ) ;
#763 = ORIENTED_EDGE ( 'NONE', *, *, #7373, .F. ) ;
#762 = VERTEX_POINT ( 'NONE', #1446 ) ;
#764 = CARTESIAN_POINT ( 'NONE',  ( 21.00000000000000000, 246.4843750006145058, -6.646953231504538984 ) ) ;
#765 = CARTESIAN_POINT ( 'NONE',  ( 10.69584247140429589, 30.35231371789855359, 6.932735513424201024 ) ) ;
#766 = CARTESIAN_POINT ( 'NONE',  ( 23.87821517812500005, -4.985214923628404016, -2.240624999385460114 ) ) ;
#767 = CARTESIAN_POINT ( 'NONE',  ( -13.23911966647199812, 126.9523137178985621, -8.632099005475788900 ) ) ;
#768 = CARTESIAN_POINT ( 'NONE',  ( 15.00000000000000178, -3.464101615137757051, -6.206249998770966059 ) ) ;
#769 = DIRECTION ( 'NONE',  ( 0.000000000000000000, 0.000000000000000000, 1.000000000000000000 ) ) ;
#770 = EDGE_LOOP ( 'NONE', ( #13450, #36497, #28822 ) ) ;
#771 = CARTESIAN_POINT ( 'NONE',  ( 10.31873187879410736, -3.604726614523244610, -3.309374999385498395 ) ) ;
#772 = VECTOR ( 'NONE', #3527, 1000.000000000000000 ) ;
#773 = ORIENTED_EDGE ( 'NONE', *, *, #629, .F. ) ;
#774 = CARTESIAN_POINT ( 'NONE',  ( 5.778771075727756162E-15, 197.6656250006145399, 31.45816453501075927 ) ) ;
#775 = CARTESIAN_POINT ( 'NONE',  ( 24.70858993122118363, 3.604726614523240613, 164.0263046051175024 ) ) ;
#776 = EDGE_CURVE ( 'NONE', #35917, #28635, #13022, .T. ) ;
#777 = CARTESIAN_POINT ( 'NONE',  ( -63.05877896937850835, 212.1620413398627534, -8.530955311639255356 ) ) ;
#778 = CARTESIAN_POINT ( 'NONE',  ( 18.00000000000000355, 245.6312500012290343, 5.196152422706632912 ) ) ;
#779 = CARTESIAN_POINT ( 'NONE',  ( 13.50000000000001421, 196.5500000000000114, 23.38268590217984055 ) ) ;
#780 = CARTESIAN_POINT ( 'NONE',  ( -48.61086230271182984, 212.1499508600178387, -3.954877714930852495 ) ) ;
#781 = CARTESIAN_POINT ( 'NONE',  ( -36.74330436395489841, 210.1155267958017134, -6.500000000000000888 ) ) ;
#782 = CARTESIAN_POINT ( 'NONE',  ( 25.03378979634835488, -3.604726614523240613, 167.7433560723723076 ) ) ;
#783 = ORIENTED_EDGE ( 'NONE', *, *, #9463, .T. ) ;
#784 = CARTESIAN_POINT ( 'NONE',  ( 2.999999999999997335, 252.0000000000000000, -2.500000000000000000 ) ) ;
#785 = CARTESIAN_POINT ( 'NONE',  ( -11.08355503943142573, 140.3601862821014663, 10.83675517735155402 ) ) ;
#786 = CARTESIAN_POINT ( 'NONE',  ( -66.62872103062156270, 201.4690446883607819, 2.162041339862843525 ) ) ;
#787 = CARTESIAN_POINT ( 'NONE',  ( 5.529263428287477744, 126.2726862821014464, -7.954856959092191815 ) ) ;
#788 = LINE ( 'NONE', #10083, #33967 ) ;
#789 = CARTESIAN_POINT ( 'NONE',  ( 10.69584247140445221, 34.84768628210143504, -6.932735513423970097 ) ) ;
#790 = EDGE_CURVE ( 'NONE', #30802, #1071, #21746, .T. ) ;
#791 = CARTESIAN_POINT ( 'NONE',  ( 13.56230152254410726, 5.196152422706636465, -6.375000000000019540 ) ) ;
#792 = ORIENTED_EDGE ( 'NONE', *, *, #29984, .F. ) ;
#793 = CARTESIAN_POINT ( 'NONE',  ( -32.58705436395489841, 205.3262412349647548, -4.842901733360204908 ) ) ;
#794 = CARTESIAN_POINT ( 'NONE',  ( 15.46528703574804986, 118.7976862821014521, 3.257655550457285720 ) ) ;
#795 =( BOUNDED_CURVE ( )  B_SPLINE_CURVE ( 2, ( #34956, #23784, #32113, #6149, #3492, #15063, #12212 ),
 .UNSPECIFIED., .F., .F. ) 
 B_SPLINE_CURVE_WITH_KNOTS ( ( 3, 2, 2, 3 ),
 ( 0.02173913043478289606, 0.02898550724637719705, 0.03623188405797149458, 0.04347826086956579211 ),
 .UNSPECIFIED. ) 
 CURVE ( )  GEOMETRIC_REPRESENTATION_ITEM ( )  RATIONAL_B_SPLINE_CURVE ( ( 0.9999999999999946709, 0.8660254037844440367, 1.000000000000000000, 0.8660254037844387076, 1.000000000000000000, 0.8660254037844280495, 1.000000000000010658 ) ) 
 REPRESENTATION_ITEM ( '' )  );
#796 = LINE ( 'NONE', #12366, #13356 ) ;
#797 = CARTESIAN_POINT ( 'NONE',  ( 8.710071997420211432, 139.3148137178985451, -3.796722387233181895 ) ) ;
#798 = CARTESIAN_POINT ( 'NONE',  ( 13.62178482187501416, 197.7031250006145342, 23.59362340125806767 ) ) ;
#799 = CARTESIAN_POINT ( 'NONE',  ( 1.255007937094097924E-14, 199.4375000000000284, -27.00000000000000355 ) ) ;
#800 = CARTESIAN_POINT ( 'NONE',  ( 10.56230152254594756, 3.464101615138813095, -1.274999998771018772 ) ) ;
#801 = DIRECTION ( 'NONE',  ( 1.000000000000000000, 0.000000000000000000, 0.000000000000000000 ) ) ;
#802 = CARTESIAN_POINT ( 'NONE',  ( 21.00000000000000355, 0.000000000000000000, 50.00000000000001421 ) ) ;
#803 = CARTESIAN_POINT ( 'NONE',  ( 9.500000000000005329, 75.48981371789854222, -0.1745138560723090149 ) ) ;
#804 = CARTESIAN_POINT ( 'NONE',  ( 26.99999999999999289, 0.000000000000000000, 49.73803434254939759 ) ) ;
#805 = VERTEX_POINT ( 'NONE', #21931 ) ;
#806 = CARTESIAN_POINT ( 'NONE',  ( 26.99999999999999645, 244.3937500012290513, 3.464101615137751278 ) ) ;
#807 = CARTESIAN_POINT ( 'NONE',  ( 0.1745138560722779009, 96.18981371789855928, 12.50000000000000355 ) ) ;
#808 = CARTESIAN_POINT ( 'NONE',  ( 22.80587116629411781, -3.604726614523238837, -4.509374999385530103 ) ) ;
#809 = FACE_BOUND ( 'NONE', #24901, .T. ) ;
#810 = CARTESIAN_POINT ( 'NONE',  ( 21.00000000000000000, 6.646953231504538984, -5.765624999385476457 ) ) ;
#811 = CARTESIAN_POINT ( 'NONE',  ( 12.46528703574811558, 56.80231371789856354, -2.660918448318005503 ) ) ;
#812 = CARTESIAN_POINT ( 'NONE',  ( -13.62178482187500528, 197.5343750006145456, -23.59362340125807123 ) ) ;
#813 = EDGE_LOOP ( 'NONE', ( #35823, #32630, #11265, #6472 ) ) ;
#814 = CIRCLE ( 'NONE', #21430, 7.500000000000000000 ) ;
#815 = VERTEX_POINT ( 'NONE', #7521 ) ;
#816 = CARTESIAN_POINT ( 'NONE',  ( 18.12178482187500350, -4.985214923628407568, -5.915624999385471483 ) ) ;
#817 = CARTESIAN_POINT ( 'NONE',  ( -13.49999999999998401, 195.5749999999999886, 23.38268590217985476 ) ) ;
#818 = CARTESIAN_POINT ( 'NONE',  ( 26.75643035624999655, 244.1593750006145171, -3.323476615752271712 ) ) ;
#819 = ADVANCED_FACE ( 'NONE', ( #19094 ), #30646, .F. ) ;
#820 = CARTESIAN_POINT ( 'NONE',  ( -12.46528703574805697, 40.59768628210144215, -2.660918448318280838 ) ) ;
#821 = CARTESIAN_POINT ( 'NONE',  ( -33.17336230271182984, 215.6869285224997270, 3.149950860017831200 ) ) ;
#822 = CARTESIAN_POINT ( 'NONE',  ( 19.68408634441910365, -5.407089921784855591, -0.8906249993855530622 ) ) ;
#823 = CARTESIAN_POINT ( 'NONE',  ( -66.22544563604516554, 214.8429017333602360, 4.673758765035156415 ) ) ;
#824 = FILL_AREA_STYLE_COLOUR ( '', #4427 ) ;
#825 = STYLED_ITEM ( 'NONE', ( #26368 ), #18760 ) ;
#826 = CARTESIAN_POINT ( 'NONE',  ( 30.69389748721465949, -6.928203230275506996, 160.8017552964788592 ) ) ;
#827 = CARTESIAN_POINT ( 'NONE',  ( -4.944772684328424539, 91.01481371789856212, -11.48171059495408031 ) ) ;
#828 = CARTESIAN_POINT ( 'NONE',  ( -48.42038769728824832, 208.6787018382581778, 4.469044688360752637 ) ) ;
#829 = CARTESIAN_POINT ( 'NONE',  ( -37.13913769728823411, 205.8500491399820760, -7.418979330068584233 ) ) ;
#830 = CARTESIAN_POINT ( 'NONE',  ( 26.75643035624999655, 3.323476615752271268, -6.290624999385498128 ) ) ;
#831 = CARTESIAN_POINT ( 'NONE',  ( 16.56230152254411436, 6.928203230275506996, -0.8999999987709939031 ) ) ;
#832 = CARTESIAN_POINT ( 'NONE',  ( 15.46528703574811736, 56.80231371789854933, -3.257655550456947768 ) ) ;
#833 = CARTESIAN_POINT ( 'NONE',  ( -58.11086230271183695, 214.1499508600178387, -7.418979330068641964 ) ) ;
#834 = LINE ( 'NONE', #16009, #19275 ) ;
#835 = CARTESIAN_POINT ( 'NONE',  ( -11.48171059495397373, 86.88518628210145778, -4.944772684328680334 ) ) ;
#836 = CARTESIAN_POINT ( 'NONE',  ( 8.632099005475504683, 27.94768628210144001, 13.23911966647218996 ) ) ;
#837 = CARTESIAN_POINT ( 'NONE',  ( 21.95617849068234761, 3.814046910745170660, -9.967423460872726793 ) ) ;
#838 = CARTESIAN_POINT ( 'NONE',  ( 33.81932759197320593, -5.407089921784861808, 160.7071210016154055 ) ) ;
#839 = CARTESIAN_POINT ( 'NONE',  ( -15.50000000000000533, 49.51018628210145067, -0.1745138560725808530 ) ) ;
#840 = CARTESIAN_POINT ( 'NONE',  ( 27.24356964375000345, 198.6781250006145569, -3.336375036156643733E-15 ) ) ;
#841 =( BOUNDED_CURVE ( )  B_SPLINE_CURVE ( 2, ( #13122, #26953, #12745, #33021, #24313, #35856, #23936 ),
 .UNSPECIFIED., .F., .F. ) 
 B_SPLINE_CURVE_WITH_KNOTS ( ( 3, 2, 2, 3 ),
 ( 0.5434782608695670758, 0.5507246376811614219, 0.5579710144927557680, 0.5652173913043500031 ),
 .UNSPECIFIED. ) 
 CURVE ( )  GEOMETRIC_REPRESENTATION_ITEM ( )  RATIONAL_B_SPLINE_CURVE ( ( 0.9999999999999651390, 0.8660254037844735686, 1.000000000000000000, 0.8660254037844387076, 1.000000000000000000, 0.8660254037843976294, 1.000000000000041078 ) ) 
 REPRESENTATION_ITEM ( '' )  );
#842 = CARTESIAN_POINT ( 'NONE',  ( -37.73288769728821279, 203.5309553116391612, -1.857196546604028775 ) ) ;
#843 = CARTESIAN_POINT ( 'NONE',  ( -27.00000000000000355, 195.4625000000000057, -15.58845726811989429 ) ) ;
#844 = CARTESIAN_POINT ( 'NONE',  ( -6.932735513423968321, 14.14768628210144463, -10.69584247140445221 ) ) ;
#845 = CARTESIAN_POINT ( 'NONE',  ( 25.05990503573306682, 0.000000000000000000, 165.2472063767010013 ) ) ;
#846 = CARTESIAN_POINT ( 'NONE',  ( 9.534712964251900402, 121.7773137178985650, 1.715153634034445540 ) ) ;
#847 = CARTESIAN_POINT ( 'NONE',  ( 26.75643035624999655, 246.0718750006145399, -3.323476615752271268 ) ) ;
#848 = CIRCLE ( 'NONE', #26888, 5.999999999999999112 ) ;
#849 = ORIENTED_EDGE ( 'NONE', *, *, #1576, .T. ) ;
#850 = CARTESIAN_POINT ( 'NONE',  ( 26.99999999999999645, 3.464101615137755275, -7.387499999999980638 ) ) ;
#851 = AXIS2_PLACEMENT_3D ( 'NONE', #4754, #17023, #28563 ) ;
#852 = PLANE ( 'NONE',  #25668 ) ;
#853 = DIRECTION ( 'NONE',  ( 0.000000000000000000, 0.000000000000000000, 1.000000000000000000 ) ) ;
#854 = CARTESIAN_POINT ( 'NONE',  ( 13.44051670066911086, 5.407089921784856479, -6.965624999385521932 ) ) ;
#855 = CARTESIAN_POINT ( 'NONE',  ( 31.16208724273364084, 7.209453229046475009, 166.1531886896782737 ) ) ;
#856 = LINE ( 'NONE', #4264, #19603 ) ;
#857 = CARTESIAN_POINT ( 'NONE',  ( 26.99999999999999645, 199.3625000000000114, -15.58845726811990495 ) ) ;
#858 = AXIS2_PLACEMENT_3D ( 'NONE', #37408, #25218, #21126 ) ;
#859 = CARTESIAN_POINT ( 'NONE',  ( 4.622313124798573369, 55.83518628210144641, 11.61527771782819940 ) ) ;
#860 = ORIENTED_EDGE ( 'NONE', *, *, #32619, .T. ) ;
#861 = ORIENTED_EDGE ( 'NONE', *, *, #9647, .T. ) ;
#862 = CARTESIAN_POINT ( 'NONE',  ( 27.00000000000000355, 196.7375000012290229, -3.306546357697854128E-15 ) ) ;
#863 = DIRECTION ( 'NONE',  ( 0.000000000000000000, 0.000000000000000000, 1.000000000000000000 ) ) ;
#864 = CARTESIAN_POINT ( 'NONE',  ( 27.00000000000001421, 195.2375000000000114, 15.58845726811988897 ) ) ;
#865 = CARTESIAN_POINT ( 'NONE',  ( 15.24356964374999990, 3.323476615752268604, -6.478124999385451055 ) ) ;
#866 = CARTESIAN_POINT ( 'NONE',  ( 10.49813415415989581, 100.9726862821014635, 7.228626920339068285 ) ) ;
#867 = CARTESIAN_POINT ( 'NONE',  ( -5.770363421894122880, 23.16481371789855359, 14.38691631536194393 ) ) ;
#868 = CARTESIAN_POINT ( 'NONE',  ( 10.56230152254410726, 0.000000000000000000, -5.850000000000049383 ) ) ;
#869 = CARTESIAN_POINT ( 'NONE',  ( 11.24016333012528257, 213.6599387512013095, 4.770645753574775050 ) ) ;
#870 =( BOUNDED_CURVE ( )  B_SPLINE_CURVE ( 2, ( #20831, #29529, #6222, #18875, #33264, #1604, #17986 ),
 .UNSPECIFIED., .F., .F. ) 
 B_SPLINE_CURVE_WITH_KNOTS ( ( 3, 2, 2, 3 ),
 ( 0.6304347826086960094, 0.6376811594202902445, 0.6449275362318845906, 0.6521739130434789367 ),
 .UNSPECIFIED. ) 
 CURVE ( )  GEOMETRIC_REPRESENTATION_ITEM ( )  RATIONAL_B_SPLINE_CURVE ( ( 0.9999999999999938938, 0.8660254037844448138, 1.000000000000000000, 0.8660254037844387076, 1.000000000000000000, 0.8660254037844263841, 1.000000000000012212 ) ) 
 REPRESENTATION_ITEM ( '' )  );
#871 = CARTESIAN_POINT ( 'NONE',  ( -65.03794563604515133, 206.7903428501025758, 3.378800118222471838 ) ) ;
#872 = LINE ( 'NONE', #24196, #29464 ) ;
#873 = CARTESIAN_POINT ( 'NONE',  ( 31.36063891923419789, -6.928203230275506996, 168.4226447368806987 ) ) ;
#874 = CARTESIAN_POINT ( 'NONE',  ( 5.233372021372610483, 9.652313717898541867, -8.152565276336593669 ) ) ;
#875 = CARTESIAN_POINT ( 'NONE',  ( -54.15997103062156981, 215.5714017266979852, 3.350049139982118618 ) ) ;
#876 = CARTESIAN_POINT ( 'NONE',  ( -69.59747103062156270, 214.3500491399821044, -7.303452534266878793 ) ) ;
#877 = ITEM_DEFINED_TRANSFORMATION ( 'NONE', 'NONE', #27492,  #17215 ) ;
#878 = CARTESIAN_POINT ( 'NONE',  ( 15.00000000000000000, 241.0000000000000000, 0.000000000000000000 ) ) ;
#879 = CARTESIAN_POINT ( 'NONE',  ( -13.62178482187498396, 199.4281250006145569, 23.59362340125808188 ) ) ;
#880 = CARTESIAN_POINT ( 'NONE',  ( -8.632099005475794229, 115.4523137178985479, 13.23911966647199812 ) ) ;
#881 = CARTESIAN_POINT ( 'NONE',  ( -64.04836230271183695, 204.3130714775002446, -3.149950860017828091 ) ) ;
#882 = ORIENTED_EDGE ( 'NONE', *, *, #5987, .T. ) ;
#883 = CARTESIAN_POINT ( 'NONE',  ( 12.53471296425194836, 35.42268628210144499, -2.311890736173178418 ) ) ;
#884 = CARTESIAN_POINT ( 'NONE',  ( -5.023457906468643763, 224.4868866335225448, -2.499999999999999556 ) ) ;
#885 = CARTESIAN_POINT ( 'NONE',  ( 20.00041244883536606, 239.7473985345926053, -5.668978318349186196 ) ) ;
#886 = CARTESIAN_POINT ( 'NONE',  ( 28.14206111430700474, -5.407089921784865361, 167.4525959469342524 ) ) ;
#887 = CARTESIAN_POINT ( 'NONE',  ( -15.50000000000000533, 104.7101862821014606, -0.1745138560725808530 ) ) ;
#888 = CARTESIAN_POINT ( 'NONE',  ( -62.67038769728823411, 208.1428034533959703, 6.469044688360771289 ) ) ;
#889 = EDGE_CURVE ( 'NONE', #36288, #26422, #2026, .T. ) ;
#890 = CARTESIAN_POINT ( 'NONE',  ( 13.44051670066911264, -5.407089921784859143, -2.765624999385540850 ) ) ;
#891 = CARTESIAN_POINT ( 'NONE',  ( 9.500000000000005329, 63.31018628210144783, 0.1745138560725188748 ) ) ;
#892 = DIRECTION ( 'NONE',  ( 1.000000000000000000, 0.000000000000000000, 0.000000000000000000 ) ) ;
#893 = CARTESIAN_POINT ( 'NONE',  ( -69.39955436395486288, 214.8429017333601792, -4.673758765035196383 ) ) ;
#894 = EDGE_CURVE ( 'NONE', #12557, #11771, #34221, .T. ) ;
#895 = CARTESIAN_POINT ( 'NONE',  ( -2.660918448318275509, 75.09768628210143504, 12.46528703574805874 ) ) ;
#896 = CARTESIAN_POINT ( 'NONE',  ( 3.306546357697854128E-15, 200.0000000000000000, 27.00000000000000355 ) ) ;
#897 = CARTESIAN_POINT ( 'NONE',  ( 21.00000000000000000, 247.4687500012290400, 5.999999999999998224 ) ) ;
#898 = ORIENTED_EDGE ( 'NONE', *, *, #5997, .F. ) ;
#899 = CARTESIAN_POINT ( 'NONE',  ( 33.71964321120555752, 5.407089921784857367, 159.5677233156729642 ) ) ;
#900 = CARTESIAN_POINT ( 'NONE',  ( 26.99999999999999645, 3.464101615137755275, -0.6375000000000126121 ) ) ;
#901 = CARTESIAN_POINT ( 'NONE',  ( 10.56230152254374310, -3.464101615137546109, -6.712500000000007461 ) ) ;
#902 = CARTESIAN_POINT ( 'NONE',  ( 24.90795869275643426, 0.000000000000000000, 166.3050999770023850 ) ) ;
#903 = UNCERTAINTY_MEASURE_WITH_UNIT (LENGTH_MEASURE( 1.000000000000000082E-05 ), #4566, 'distance_accuracy_value', 'NONE');
#904 = CARTESIAN_POINT ( 'NONE',  ( 36.98482634954957859, 7.347880794884125653E-16, 163.8651217518988688 ) ) ;
#905 = DIRECTION ( 'NONE',  ( 1.000000000000000000, 0.000000000000000000, 0.000000000000000000 ) ) ;
#906 = CARTESIAN_POINT ( 'NONE',  ( 24.00000000000000000, 247.4500000000000171, 5.196152422706629359 ) ) ;
#907 = CARTESIAN_POINT ( 'NONE',  ( -13.62178482187498396, 196.7281250006145399, 23.59362340125808188 ) ) ;
#908 = EDGE_CURVE ( 'NONE', #17354, #5563, #28159, .T. ) ;
#909 = CARTESIAN_POINT ( 'NONE',  ( -0.1745138560722763466, 100.7898137178985536, -12.50000000000000355 ) ) ;
#910 = CARTESIAN_POINT ( 'NONE',  ( -10.69584247140444866, 103.8476862821014493, 6.932735513423972762 ) ) ;
#911 = ORIENTED_EDGE ( 'NONE', *, *, #11960, .F. ) ;
#912 = EDGE_LOOP ( 'NONE', ( #20316, #5565, #15559, #5000 ) ) ;
#913 = CARTESIAN_POINT ( 'NONE',  ( -27.24356964374999990, 196.1656250006145399, -15.72908226750537786 ) ) ;
#914 = LINE ( 'NONE', #15712, #11994 ) ;
#915 = CARTESIAN_POINT ( 'NONE',  ( 15.53471296425188797, 84.97731371789856780, 2.908627838312457747 ) ) ;
#916 = AXIS2_PLACEMENT_3D ( 'NONE', #4687, #25159, #10753 ) ;
#917 = CARTESIAN_POINT ( 'NONE',  ( 21.00000000000000000, 6.646953231504538984, -3.515624999385498217 ) ) ;
#918 = TOROIDAL_SURFACE ( 'NONE', #30587, 18.00000000000000355, 10.00000000000000000 ) ;
#919 = CARTESIAN_POINT ( 'NONE',  ( 21.00000000000000000, 248.1718750006145342, 6.646953231504538984 ) ) ;
#920 = CARTESIAN_POINT ( 'NONE',  ( 9.465287035748067623, 100.3976862821014606, 2.064181346179272847 ) ) ;
#921 = CARTESIAN_POINT ( 'NONE',  ( 1.069080835302379631E-14, 197.9750000012290343, 27.00000000000000000 ) ) ;
#922 = CARTESIAN_POINT ( 'NONE',  ( 1.715153634034445762, 55.07731371789854080, -9.534712964251895073 ) ) ;
#923 = CARTESIAN_POINT ( 'NONE',  ( 13.44051670066911086, 5.407089921784856479, -4.715624999385548577 ) ) ;
#924 = CARTESIAN_POINT ( 'NONE',  ( -6.594114490232462877, 115.7398137178985564, 6.840914352311949109 ) ) ;
#925 = CARTESIAN_POINT ( 'NONE',  ( 15.24356964374999990, 240.7093750006144717, -3.323476615752268604 ) ) ;
#926 = CARTESIAN_POINT ( 'NONE',  ( 0.1745138560722779009, 22.58981371789854720, 12.50000000000000355 ) ) ;
#927 = FACE_BOUND ( 'NONE', #31912, .T. ) ;
#928 = CARTESIAN_POINT ( 'NONE',  ( 0.1745138560725515708, 79.41018628210144925, -12.50000000000000355 ) ) ;
#929 = CARTESIAN_POINT ( 'NONE',  ( 16.56230152254411081, -6.928203230275506996, -5.174999998771001586 ) ) ;
#930 = CARTESIAN_POINT ( 'NONE',  ( 37.29692136982500728, 3.604726614523238837, 164.6377359093410746 ) ) ;
#931 = CARTESIAN_POINT ( 'NONE',  ( -5.770363421893818234, 88.03518628210144925, -14.38691631536207005 ) ) ;
#932 = AXIS2_PLACEMENT_3D ( 'NONE', #8550, #25977, #8 ) ;
#933 = CARTESIAN_POINT ( 'NONE',  ( 16.56230152254411436, 7.209453229046482114, -4.809374999385505944 ) ) ;
#934 = PLANE ( 'NONE',  #1221 ) ;
#935 = CARTESIAN_POINT ( 'NONE',  ( 5.438367727407757144E-14, 198.5374999999999943, -27.00000000000000000 ) ) ;
#936 = CARTESIAN_POINT ( 'NONE',  ( 1.715153634034233487, 120.5226862821014322, 9.534712964251941258 ) ) ;
#937 = AXIS2_PLACEMENT_3D ( 'NONE', #24457, #33914, #7396 ) ;
#938 = CARTESIAN_POINT ( 'NONE',  ( -0.1745138560725500443, 139.2101862821014606, 12.50000000000000355 ) ) ;
#939 = CARTESIAN_POINT ( 'NONE',  ( 5.778771075727756162E-15, 195.0218750006145569, 31.45816453501075927 ) ) ;
#940 = CARTESIAN_POINT ( 'NONE',  ( 26.75643035624999655, 240.4843750006145058, 3.323476615752267715 ) ) ;
#941 = VERTEX_POINT ( 'NONE', #5036 ) ;
#942 = CARTESIAN_POINT ( 'NONE',  ( 31.22091736908830839, -7.209453229046475009, 166.8256201108902133 ) ) ;
#943 = CARTESIAN_POINT ( 'NONE',  ( 23.87821517812500005, -4.985214923628404016, -2.690624999385465621 ) ) ;
#944 = CARTESIAN_POINT ( 'NONE',  ( 22.60769515458672885, 242.4825961894323143, 5.999999999999997335 ) ) ;
#945 = CARTESIAN_POINT ( 'NONE',  ( 10.56230152254410726, 0.000000000000000000, -7.650000000000045652 ) ) ;
#946 = CARTESIAN_POINT ( 'NONE',  ( -95.81998461310567450, 11.77610610744882358, 3.000000000000000000 ) ) ;
#947 = DIRECTION ( 'NONE',  ( -0.000000000000000000, 1.000000000000000000, -0.000000000000000000 ) ) ;
#948 = CARTESIAN_POINT ( 'NONE',  ( 7.234628195640322446, 198.3325961894323370, 26.99999999999999645 ) ) ;
#949 = CARTESIAN_POINT ( 'NONE',  ( 5.233372021372610483, 28.05231371789855643, -8.152565276336593669 ) ) ;
#950 = CARTESIAN_POINT ( 'NONE',  ( -1.926257025242585782E-15, 196.5968750006145456, -31.45816453501076637 ) ) ;
#952 = VERTEX_POINT ( 'NONE', #16800 ) ;
#951 = ORIENTED_EDGE ( 'NONE', *, *, #25354, .F. ) ;
#953 = CARTESIAN_POINT ( 'NONE',  ( 26.75643035624999655, 247.7218750006145171, -7.049594010296217766E-16 ) ) ;
#954 = CARTESIAN_POINT ( 'NONE',  ( 7.228626920338837358, 30.92731371789854578, 10.49813415416005036 ) ) ;
#955 = CARTESIAN_POINT ( 'NONE',  ( 26.75643035624999655, 3.323476615752271712, -2.128124999385482052 ) ) ;
#956 = CARTESIAN_POINT ( 'NONE',  ( 13.04141134922778988, 139.0273137178985507, -8.927990412390371944 ) ) ;
#957 = CARTESIAN_POINT ( 'NONE',  ( 26.99999999999999645, 7.347880794884117764E-16, -7.818749998770941012 ) ) ;
#958 = CARTESIAN_POINT ( 'NONE',  ( 3.253724281355069334E-15, 199.5500000012290513, -27.00000000000000000 ) ) ;
#959 = ORIENTED_EDGE ( 'NONE', *, *, #15902, .F. ) ;
#960 = CARTESIAN_POINT ( 'NONE',  ( 22.80587116629411426, 7.646167579472024665E-16, -6.721874999385535787 ) ) ;
#961 = ORIENTED_EDGE ( 'NONE', *, *, #8896, .T. ) ;
#962 = CARTESIAN_POINT ( 'NONE',  ( -27.24356964375000345, 196.2031250006145342, 0.000000000000000000 ) ) ;
#963 = CARTESIAN_POINT ( 'NONE',  ( -8.962234695871760692, 131.1601862821014777, 8.715434833791933400 ) ) ;
#964 = CARTESIAN_POINT ( 'NONE',  ( 24.75434669616370087, -3.604726614523244610, 164.5493068216156871 ) ) ;
#965 = CARTESIAN_POINT ( 'NONE',  ( -60.68377896937850835, 207.8379586601372750, 8.530955311639258909 ) ) ;
#966 = CARTESIAN_POINT ( 'NONE',  ( 20.99999999999999645, 245.5843750006145285, -6.646953231504538984 ) ) ;
#967 =( NAMED_UNIT ( * ) SI_UNIT ( $, .STERADIAN. ) SOLID_ANGLE_UNIT ( ) );
#968 = CARTESIAN_POINT ( 'NONE',  ( 22.56230152254411792, 7.347880794884125653E-16, -5.625000000000018652 ) ) ;
#969 = CARTESIAN_POINT ( 'NONE',  ( -46.23586230271182984, 207.8500491399821613, 3.954877714930852495 ) ) ;
#970 = DIRECTION ( 'NONE',  ( -0.000000000000000000, -0.000000000000000000, 1.000000000000000000 ) ) ;
#971 = CARTESIAN_POINT ( 'NONE',  ( 31.20130732697009535, 7.209453229046475009, 166.6014763038195383 ) ) ;
#972 = VERTEX_POINT ( 'NONE', #11471 ) ;
#973 = CARTESIAN_POINT ( 'NONE',  ( -14.38691631536207183, 131.7351862821014663, 5.770363421893814682 ) ) ;
#974 = CARTESIAN_POINT ( 'NONE',  ( -51.38913769728824121, 205.8500491399820760, -7.418979330068584233 ) ) ;
#975 = AXIS2_PLACEMENT_3D ( 'NONE', #33240, #22432, #7279 ) ;
#976 = CARTESIAN_POINT ( 'NONE',  ( -9.534712964251941258, 122.8226862821014294, 1.715153634034234154 ) ) ;
#977 = DIRECTION ( 'NONE',  ( 0.000000000000000000, 0.000000000000000000, 1.000000000000000000 ) ) ;
#978 = CARTESIAN_POINT ( 'NONE',  ( 12.50000000000000355, 35.71018628210144641, 0.1745138560725507937 ) ) ;
#979 = CARTESIAN_POINT ( 'NONE',  ( 22.56230152254412502, -3.464101615137755275, -7.012500000000041922 ) ) ;
#980 = ORIENTED_EDGE ( 'NONE', *, *, #3451, .T. ) ;
#981 = CARTESIAN_POINT ( 'NONE',  ( 3.253724281355069334E-15, 199.8875000000000455, -27.00000000000000355 ) ) ;
#982 = CARTESIAN_POINT ( 'NONE',  ( 14.38691631536207538, 117.9351862821014407, -5.770363421893813793 ) ) ;
#983 = CARTESIAN_POINT ( 'NONE',  ( 22.56230152254410726, 7.347880794884117764E-16, -9.562499998771039955 ) ) ;
#984 = CARTESIAN_POINT ( 'NONE',  ( -8.152565276336710909, 11.84768628210144747, 5.233372021372435512 ) ) ;
#985 = CARTESIAN_POINT ( 'NONE',  ( 13.62178482187499640, 197.4031250006145228, -23.59362340125807123 ) ) ;
#986 = CARTESIAN_POINT ( 'NONE',  ( 23.99999999999999645, 5.196152422706631135, -1.500000000000001332 ) ) ;
#987 = CARTESIAN_POINT ( 'NONE',  ( 27.00000000000000355, 195.2750000000000057, -3.306546357697854128E-15 ) ) ;
#988 = CARTESIAN_POINT ( 'NONE',  ( 22.39561461052787195, -1.640876061562029031, -9.999999999999998224 ) ) ;
#989 = DIRECTION ( 'NONE',  ( 0.000000000000000000, 0.000000000000000000, -1.000000000000000000 ) ) ;
#990 = DIRECTION ( 'NONE',  ( 1.000000000000000000, 0.000000000000000000, 0.000000000000000000 ) ) ;
#991 = CARTESIAN_POINT ( 'NONE',  ( 1.715153634034445762, 73.47731371789855359, -9.534712964251895073 ) ) ;
#992 = CARTESIAN_POINT ( 'NONE',  ( 25.05663669537974414, 3.464101615137583856, 165.2098490755226123 ) ) ;
#993 = EDGE_LOOP ( 'NONE', ( #26998, #21016, #13480, #17384 ) ) ;
#994 = CARTESIAN_POINT ( 'NONE',  ( 24.00000000000000000, 243.9062500012290400, 5.196152422706629359 ) ) ;
#995 = CARTESIAN_POINT ( 'NONE',  ( 11.61527771782809637, 76.06481371789855928, 4.622313124798827388 ) ) ;
#996 = CARTESIAN_POINT ( 'NONE',  ( 19.68408634441912142, -5.407089921784861808, -2.746874999385529037 ) ) ;
#997 = CARTESIAN_POINT ( 'NONE',  ( 18.00000000000000355, 242.8750000000000000, 5.196152422706632912 ) ) ;
#998 = CARTESIAN_POINT ( 'NONE',  ( 15.24356964375000167, -3.323476615752272600, -4.715624999385497063 ) ) ;
#999 = CARTESIAN_POINT ( 'NONE',  ( -2.660918448318004614, 54.50231371789855217, -12.46528703574811558 ) ) ;
#1000 = ORIENTED_EDGE ( 'NONE', *, *, #22405, .T. ) ;
#1001 = ORIENTED_EDGE ( 'NONE', *, *, #29790, .F. ) ;
#1002 = CARTESIAN_POINT ( 'NONE',  ( 20.99999999999999645, -6.646953231504538984, -6.778124999385457983 ) ) ;
#1003 = CARTESIAN_POINT ( 'NONE',  ( 15.24356964374999990, 244.3468750006145171, 0.000000000000000000 ) ) ;
#1004 = VECTOR ( 'NONE', #14540, 1000.000000000000000 ) ;
#1005 = CARTESIAN_POINT ( 'NONE',  ( 2.660918448318279950, 24.49768628210144783, -12.46528703574805697 ) ) ;
#1006 = EDGE_CURVE ( 'NONE', #5916, #35535, #23839, .T. ) ;
#1007 = CARTESIAN_POINT ( 'NONE',  ( -37.32961230271182274, 211.8571965466040581, 6.469044688360755302 ) ) ;
#1008 = CARTESIAN_POINT ( 'NONE',  ( -63.25669563604516554, 209.8844732041982013, -6.500000000000000888 ) ) ;
#1009 = CARTESIAN_POINT ( 'NONE',  ( 33.60730975337005333, -5.196152422706629359, 159.6810701411317552 ) ) ;
#1010 = CARTESIAN_POINT ( 'NONE',  ( 10.69584247140429589, 85.55231371789857064, 6.932735513424201024 ) ) ;
#1011 = CARTESIAN_POINT ( 'NONE',  ( -44.85788769728823411, 214.4690446883608104, 1.321298161741840893 ) ) ;
#1012 = CARTESIAN_POINT ( 'NONE',  ( -34.56622103062156981, 212.1620413398628671, 8.530955311639223382 ) ) ;
#1013 = EDGE_CURVE ( 'NONE', #2263, #13555, #35585, .T. ) ;
#1014 = CARTESIAN_POINT ( 'NONE',  ( 20.99999999999999645, -6.646953231504538984, -7.340624999385477523 ) ) ;
#1015 = CARTESIAN_POINT ( 'NONE',  ( 26.99999999999999645, 7.347880794884117764E-16, -2.475000000000004974 ) ) ;
#1016 = CARTESIAN_POINT ( 'NONE',  ( -8.632099005475794229, 60.25231371789854506, 13.23911966647199812 ) ) ;
#1017 = CARTESIAN_POINT ( 'NONE',  ( -50.78794563604517975, 203.8621396198271043, 6.307003348498029460 ) ) ;
#1018 = VECTOR ( 'NONE', #12976, 1000.000000000000000 ) ;
#1019 = CARTESIAN_POINT ( 'NONE',  ( 25.48152094116770883, 0.000000000000000000, 170.0662982274954800 ) ) ;
#1020 = CARTESIAN_POINT ( 'NONE',  ( -8.962234695871760692, 85.16018628210144925, 8.715434833791933400 ) ) ;
#1021 = CARTESIAN_POINT ( 'NONE',  ( -13.23911966647218463, 21.04768628210144499, 8.632099005475506459 ) ) ;
#1022 = EDGE_CURVE ( 'NONE', #18726, #12845, #31747, .T. ) ;
#1023 = CARTESIAN_POINT ( 'NONE',  ( 0.000000000000000000, 0.000000000000000000, 0.000000000000000000 ) ) ;
#1024 = CARTESIAN_POINT ( 'NONE',  ( 36.85732959234155004, 7.646167579472024665E-16, 159.6131789008408646 ) ) ;
#1025 = ORIENTED_EDGE ( 'NONE', *, *, #37375, .T. ) ;
#1026 = CARTESIAN_POINT ( 'NONE',  ( -8.927990412390661490, 57.27268628210143220, 13.04141134922759804 ) ) ;
#1027 = CARTESIAN_POINT ( 'NONE',  ( 27.24356964374999279, 198.2656250006145058, -15.72908226750539207 ) ) ;
#1028 = EDGE_CURVE ( 'NONE', #1047, #2118, #24063, .T. ) ;
#1029 = LINE ( 'NONE', #4436, #15658 ) ;
#1030 = DIRECTION ( 'NONE',  ( -0.000000000000000000, 1.000000000000000000, -0.000000000000000000 ) ) ;
#1031 = CARTESIAN_POINT ( 'NONE',  ( -32.98288769728824121, 203.5309553116391612, -1.857196546604028775 ) ) ;
#1032 = CARTESIAN_POINT ( 'NONE',  ( 24.99999999999999289, 0.000000000000000000, -8.000000000000000000 ) ) ;
#1033 = CARTESIAN_POINT ( 'NONE',  ( -11.48171059495397373, 22.48518628210144499, -4.944772684328680334 ) ) ;
#1034 = CARTESIAN_POINT ( 'NONE',  ( 20.99999999999999645, 240.7187500012290400, 5.999999999999998224 ) ) ;
#1035 = CARTESIAN_POINT ( 'NONE',  ( 8.710071997420211432, 130.1148137178985564, -3.796722387233181895 ) ) ;
#1036 = CARTESIAN_POINT ( 'NONE',  ( 20.99999999999999645, 247.2718750006145001, 6.646953231504538984 ) ) ;
#1037 = ORIENTED_EDGE ( 'NONE', *, *, #23070, .T. ) ;
#1038 = CARTESIAN_POINT ( 'NONE',  ( 26.99999999999999645, 7.347880794884117764E-16, -6.074999999999997513 ) ) ;
#1039 = DIRECTION ( 'NONE',  ( 0.000000000000000000, 0.000000000000000000, -1.000000000000000000 ) ) ;
#1040 = CARTESIAN_POINT ( 'NONE',  ( 12.53471296425189330, 140.1773137178985849, 2.311890736173451533 ) ) ;
#1041 = CARTESIAN_POINT ( 'NONE',  ( 22.80587116629411071, 3.604726614523238837, -6.178124999385540050 ) ) ;
#1042 = CARTESIAN_POINT ( 'NONE',  ( 27.82012958953286130, 5.407089921784856479, 163.7729017808578362 ) ) ;
#1043 = CARTESIAN_POINT ( 'NONE',  ( 28.42434827050043467, 5.196152422706636465, 169.2818287827543600 ) ) ;
#1044 = CARTESIAN_POINT ( 'NONE',  ( -81.00000000000002842, 210.0000000000000000, 2.500000000000001332 ) ) ;
#1045 = CARTESIAN_POINT ( 'NONE',  ( -7.228626920339070061, 48.07268628210144357, 10.49813415415989404 ) ) ;
#1046 = ORIENTED_EDGE ( 'NONE', *, *, #23097, .F. ) ;
#1047 = VERTEX_POINT ( 'NONE', #31380 ) ;
#1048 = CARTESIAN_POINT ( 'NONE',  ( 1.120210788295102201E-13, 196.8500000012290343, -27.00000000000000711 ) ) ;
#1049 = CARTESIAN_POINT ( 'NONE',  ( 16.56230152254411436, -6.928203230275514990, -3.937500000000034639 ) ) ;
#1050 = CARTESIAN_POINT ( 'NONE',  ( -13.49999999999998401, 198.3875000012290286, 23.38268590217985476 ) ) ;
#1051 = CARTESIAN_POINT ( 'NONE',  ( 26.75643035624999655, -3.323476615752267715, -7.603124999385488358 ) ) ;
#1052 = CARTESIAN_POINT ( 'NONE',  ( -4.622313124798576922, 78.83518628210146062, -11.61527771782819762 ) ) ;
#1053 = CARTESIAN_POINT ( 'NONE',  ( 13.04141134922778988, 19.42731371789854933, -8.927990412390371944 ) ) ;
#1054 = CARTESIAN_POINT ( 'NONE',  ( 22.60769515458672885, 243.4388461906613657, 5.999999999999997335 ) ) ;
#1055 = CARTESIAN_POINT ( 'NONE',  ( 13.56230152254410370, 5.196152422706630247, -4.912499998770996967 ) ) ;
#1056 = CARTESIAN_POINT ( 'NONE',  ( -34.17038769728823411, 208.6787018382581778, 4.469044688360752637 ) ) ;
#1057 = LINE ( 'NONE', #12631, #35525 ) ;
#1058 = CARTESIAN_POINT ( 'NONE',  ( 31.24297866652486633, -6.928203230275506996, 167.0777818944568480 ) ) ;
#1059 = CARTESIAN_POINT ( 'NONE',  ( -11.48171059495408208, 143.9148137178985678, 4.944772684328421875 ) ) ;
#1060 = EDGE_CURVE ( 'NONE', #37392, #27477, #5776, .T. ) ;
#1061 = CARTESIAN_POINT ( 'NONE',  ( -52.77455436395490551, 205.1570982666397356, 4.673758765035198159 ) ) ;
#1062 = CARTESIAN_POINT ( 'NONE',  ( -67.61830436395490551, 209.8844732041983150, 8.500000000000003553 ) ) ;
#1063 = EDGE_CURVE ( 'NONE', #6180, #9049, #14403, .T. ) ;
#1065 = APPLICATION_CONTEXT ( 'automotive_design' ) ;
#1064 = ITEM_DEFINED_TRANSFORMATION ( 'NONE', 'NONE', #12960,  #17215 ) ;
#1066 = CARTESIAN_POINT ( 'NONE',  ( 26.99999999999999645, 247.0374999999999943, 3.464101615137751278 ) ) ;
#1067 = CARTESIAN_POINT ( 'NONE',  ( 13.62178482187499640, 197.8531250006145399, -23.59362340125807123 ) ) ;
#1068 = CARTESIAN_POINT ( 'NONE',  ( 14.25334919248795451, 120.9148137178985678, -6.092822981423661410 ) ) ;
#1069 = CARTESIAN_POINT ( 'NONE',  ( -55.34002896937850124, 204.4285982733020433, 3.350049139982171020 ) ) ;
#1070 = EDGE_CURVE ( 'NONE', #30479, #30148, #16319, .T. ) ;
#1071 = VERTEX_POINT ( 'NONE', #25874 ) ;
#1072 =( BOUNDED_CURVE ( )  B_SPLINE_CURVE ( 2, ( #10156, #21731, #27592, #6752, #33281, #24192, #32900 ),
 .UNSPECIFIED., .F., .F. ) 
 B_SPLINE_CURVE_WITH_KNOTS ( ( 3, 2, 2, 3 ),
 ( 0.7173913043478248319, 0.7246376811594191780, 0.7318840579710134131, 0.7391304347826076482 ),
 .UNSPECIFIED. ) 
 CURVE ( )  GEOMETRIC_REPRESENTATION_ITEM ( )  RATIONAL_B_SPLINE_CURVE ( ( 1.000000000000022649, 0.8660254037844161701, 1.000000000000000000, 0.8660254037844387076, 1.000000000000000000, 0.8660254037844571373, 0.9999999999999815703 ) ) 
 REPRESENTATION_ITEM ( '' )  );
#1073 = CARTESIAN_POINT ( 'NONE',  ( -8.715434833791929847, 32.26018628210145067, -8.962234695871762469 ) ) ;
#1074 = CARTESIAN_POINT ( 'NONE',  ( 18.00000000000000355, 244.7312500012290570, 5.196152422706632912 ) ) ;
#1075 = CARTESIAN_POINT ( 'NONE',  ( -76.95115755716804529, 229.4913094451872553, -7.500000000000000000 ) ) ;
#1076 = CARTESIAN_POINT ( 'NONE',  ( 37.44236251553515871, -3.604726614523238837, 166.3001358117817006 ) ) ;
#1077 = CARTESIAN_POINT ( 'NONE',  ( -3.257655550457281723, 111.8976862821014606, 15.46528703574804986 ) ) ;
#1078 = CARTESIAN_POINT ( 'NONE',  ( -69.39955436395487709, 214.8429017333601792, -4.673758765035197271 ) ) ;
#1079 = CARTESIAN_POINT ( 'NONE',  ( 22.80587116629410716, 7.646167579472015790E-16, -3.965624999385547689 ) ) ;
#1080 = CARTESIAN_POINT ( 'NONE',  ( 3.474262827703335166, 46.63518628210144357, 8.843639120294326972 ) ) ;
#1081 = CARTESIAN_POINT ( 'NONE',  ( 15.00000000000000000, 240.6062500012290286, 0.000000000000000000 ) ) ;
#1082 = CARTESIAN_POINT ( 'NONE',  ( -39.90997103062156270, 217.3034525342668815, 4.350049139982096413 ) ) ;
#1083 = DIRECTION ( 'NONE',  ( 0.000000000000000000, 0.000000000000000000, 1.000000000000000000 ) ) ;
#1084 = CARTESIAN_POINT ( 'NONE',  ( -7.228626920339069173, 84.87268628210146915, 10.49813415415989581 ) ) ;
#1085 = CARTESIAN_POINT ( 'NONE',  ( 15.00000000000000355, 7.347880794884112834E-16, -8.000000000000000000 ) ) ;
#1086 = CARTESIAN_POINT ( 'NONE',  ( 22.60769515458672885, 247.6736538117966973, -6.000000000000000000 ) ) ;
#1088 = ORIENTED_EDGE ( 'NONE', *, *, #15863, .T. ) ;
#1087 = CARTESIAN_POINT ( 'NONE',  ( 0.1745138560725194299, 51.81018628210144783, -9.500000000000005329 ) ) ;
#1089 = CARTESIAN_POINT ( 'NONE',  ( 24.39973176785919051, 3.604726614523236616, 160.4960396437548695 ) ) ;
#1090 = CARTESIAN_POINT ( 'NONE',  ( 21.00000000000000000, -6.646953231504538984, -9.478124999385466154 ) ) ;
#1091 = CARTESIAN_POINT ( 'NONE',  ( 25.40961745350799461, 3.464101615137737067, 169.2444376027941360 ) ) ;
#1092 = CARTESIAN_POINT ( 'NONE',  ( 24.79356678040014117, -3.604726614523244610, 164.9975944357569517 ) ) ;
#1093 = CARTESIAN_POINT ( 'NONE',  ( 36.86389775648721212, -3.464101615137755275, 162.4829016082965438 ) ) ;
#1094 = CARTESIAN_POINT ( 'NONE',  ( 15.00000000000000000, 246.8500000000000227, 0.000000000000000000 ) ) ;
#1095 = CARTESIAN_POINT ( 'NONE',  ( -13.62178482187500528, 196.5781250006145342, -23.59362340125807123 ) ) ;
#1096 =( BOUNDED_SURFACE ( )  B_SPLINE_SURFACE ( 3, 2, ( 
 ( #17208, #19878, #22527, #2787, #34446, #8486, #20056, #31601, #31421, #7933, #5265, #5624, #19508, #23080, #16843, #31054, #16469, #5076, #14361, #28202, #8124, #311, #26279, #498, #17583, #11877, #23446, #29308, #34999, #21179, #14915, #17398, #12254, #12064, #32344, #23638, #9227, #2973, #24016, #32154, #23824, #35366, #26464, #35561, #31973, #9418, #3160, #3347, #9042, #9605, #3538, #23266, #29499, #20993, #20801, #5816, #15293, #28938, #6003, #32528, #684, #35181, #14543, #6381, #26098, #17956, #11693, #20614, #34810, #26845, #15103, #26653, #129, #18145, #6571, #29687, #3721, #6194, #17766, #8855, #875, #12447, #20429, #29116, #14731, #13200, #6758, #1061, #29877, #18528, #30258, #30453, #27597, #13014, #12634, #9974, #15482, #33101, #21554, #24387, #16236, #1248, #24752, #18332, #24199, #3910, #30066, #4284, #4471, #1628, #24568, #35744, #36301, #27037, #9790, #27787, #30637, #16050, #36490, #10162, #1814, #7144, #10533, #7512, #15673, #13382, #32718, #24935, #21367, #12818, #32906, #10348, #21921, #33470, #35932, #6960, #18901, #4101, #18718, #19086, #27223, #15861, #27406, #1438, #36122, #4654, #21737, #33288, #7327, #2558, #14127, #25683, #8258, #19648, #16421, #10906, #37233, #25124, #31553, #22480, #13572, #17163, #28703, #28335, #13946, #31370, #16608, #5028, #16790, #33846, #28151, #2181, #8072, #13763, #37414, #31190, #33658, #28515, #2372, #11095, #25495, #37047, #19278, #2740, #34027, #11281, #22851, #5213, #14312, #10719, #34400, #19459, #22669 ),
 ( #34213, #25865, #5577, #22109, #22293, #8438, #16973, #19831, #7698, #5393, #30818, #20007, #27968, #25309, #36681, #4842, #1998, #7885, #31008, #36861, #635, #26606, #3297, #266, #23218, #31923, #29067, #34948, #3112, #26796, #20564, #23033, #17907, #17717, #450, #29256, #14869, #8621, #29639, #11829, #29451, #3486, #32106, #3676, #77, #15056, #8809, #8994, #14678, #15245, #9181, #28890, #35130, #12205, #26415, #11464, #20945, #34580, #11642, #23777, #6335, #6140, #20190, #12018, #31739, #23588, #17347, #5954, #2924, #32478, #20750, #32295, #5767, #35315, #9370, #6525, #18099, #23400, #26228, #14493, #26050, #34767, #20381, #17533, #6905, #18851, #12395, #6711, #35510, #24151, #35881, #36071, #33238, #18666, #18283, #7277, #9556, #3862, #33422, #36254, #10115, #4606, #15810, #7460, #27174, #16186, #13148, #21318, #19039, #828, #30591, #21131, #18477, #23967, #30398, #21686, #27549, #30018, #32669, #24522, #26985, #15620, #1577, #12585, #29826, #21869, #15436, #1011, #24702, #33051, #35694, #10297, #4421, #16002, #9746, #32856, #9924, #4048, #1198, #12771, #24341, #21507, #7098, #30207, #4234, #27360, #1390, #12963, #36998, #22247, #10668, #22430, #31142, #24890, #8392, #16557, #8208, #19784, #36814, #19961, #16371, #31321, #25074, #25263, #7835, #31504, #25445, #7650, #13897, #5349, #5161, #5526, #37184, #27735, #27916, #16926, #22617, #10857, #1766, #16740, #13332, #2325, #33611, #33798, #19227, #11227, #28287, #11041, #36440, #2505, #28468, #14078, #19594 ),
 ( #22798, #19408, #25628, #10479, #30771, #22058, #13517, #33978, #34164, #34349, #8019, #4793, #1946, #36628, #30958, #4976, #28103, #2135, #13714, #32060, #12156, #5905, #20893, #29406, #30, #23731, #32436, #35268, #25816, #34713, #9324, #23542, #26370, #6286, #23170, #17112, #3251, #5716, #31875, #17862, #28838, #28652, #587, #37361, #2689, #3438, #11784, #2872, #15007, #35087, #9137, #20702, #14825, #14632, #11415, #17485, #32246, #20140, #26559, #29017, #8572, #14265, #22983, #23352, #8948, #403, #11595, #8759, #34904, #14445, #20333, #3063, #26182, #220, #34533, #20521, #31687, #17297, #6089, #17673, #29210, #26001, #11970, #33197, #18239, #6480, #27511, #26748, #18052, #7238, #1159, #29783, #18812, #24483, #36029, #10073, #30166, #4003, #780, #32813, #21644, #9514, #15957, #6856, #35463, #1534, #13106, #12731, #35841, #15770, #969, #26938, #24298, #3814, #12545, #24110, #29973, #35654, #21831, #15578, #29594, #12920, #9883, #33005, #21464, #7055, #3631, #24661, #18432, #30356, #4380, #27132, #36213, #32627, #10255, #15391, #18625, #9700, #15200, #4193, #23922, #27320, #12348, #1348, #21087, #6664, #21277, #33572, #22574, #28251, #4933, #7425, #22388, #11185, #7980, #1723, #16328, #24848, #5310, #33938, #19553, #37143, #8170, #34120, #11002, #25223, #22206, #10627, #16144, #33755, #7795, #25029, #16888, #1907, #13857, #18994, #13292, #30551, #19184, #30914, #31102, #2280, #13675, #36398, #25405, #4568, #10444, #28424, #31282, #5123, #33385, #10817, #2465 ),
 ( #19745, #27876, #19372, #14039, #25588, #36956, #16703, #27695, #28062, #16515, #7608, #36772, #22019, #30733, #13477, #4756, #36588, #2097, #18152, #14922, #881, #35566, #29885, #35005, #12452, #690, #32726, #22759, #6576, #15109, #35188, #20999, #9233, #3916, #29693, #6763, #17963, #20808, #18337, #24021, #32350, #32536, #9612, #3546, #19925, #15489, #35372, #5485, #3726, #23831, #9048, #26471, #6388, #29505, #26660, #15299, #20620, #12261, #9424, #26852, #27043, #17068, #32160, #3354, #1069, #31463, #21186, #34308, #8352, #28608, #2645, #14221, #25771, #37323, #17772, #23452, #11884, #6199, #29314, #504, #12070, #23645, #4291, #9980, #1635, #16056, #13020, #24576, #36307, #1819, #33106, #1444, #33663, #27792, #4659, #27604, #10538, #7334, #36127, #24392, #24757, #33293, #7151, #12640, #7703, #27230, #1255, #30825, #10169, #18724, #24940, #12824, #21373, #4477, #27412, #32912, #18907, #13207, #21744, #4107, #6966, #30460, #10355, #30265, #4848, #13388, #22115, #16243, #36495, #35939, #21928, #15679, #33475, #7519, #27973, #16427, #19091, #30643, #35750, #21561, #19286, #24205, #15869, #9795, #18534, #30072, #13768, #17168, #16978, #11469, #2004, #22856, #31378, #13952, #37238, #25501, #20195, #34406, #23039, #34219, #37053, #34585, #28709, #11101, #11288, #2744, #19837, #36686, #31745, #14133, #22299, #8444, #2563, #25315, #5220, #22674, #8264, #5398, #20012, #36866, #28521, #25689, #31558, #5773, #33851, #10911, #19653, #8627, #10724, #5582, #17353, #14318, #37419 ),
 ( #25871, #13577, #25130, #7892, #2187, #19466, #31195, #22488, #31013, #5034, #2377, #16614, #28156, #34034, #8078, #28342, #16796, #6530, #20950, #6341, #26801, #23593, #29263, #3117, #3491, #12024, #11834, #28895, #12400, #5960, #17539, #9561, #26421, #23405, #3682, #29073, #83, #20755, #6145, #11647, #35135, #32301, #17722, #20387, #23223, #9187, #17911, #34954, #21137, #18104, #833, #32483, #15250, #14684, #29456, #31928, #12210, #455, #6717, #32674, #3303, #14873, #14498, #15062, #23973, #34772, #8999, #2930, #29644, #26612, #26055, #8813, #641, #26233, #23783, #35321, #271, #32111, #9376, #35516, #20569, #1583, #4053, #4239, #7282, #24708, #36445, #1017, #27179, #35887, #13337, #15441, #15815, #1771, #4426, #16192, #19045, #1395, #27742, #12590, #12776, #18483, #36260, #27365, #10303, #21874, #30023, #36076, #9931, #15626, #18856, #21692, #18672, #30214, #16008, #7466, #1203, #7103, #24896, #33426, #30596, #33242, #10485, #12970, #24527, #24346, #30404, #10120, #21512, #18289, #22065, #32864, #6912, #33616, #27556, #33056, #4611, #13153, #26989, #29832, #3868, #24156, #35699, #9751, #21324, #36634, #1952, #13903, #25451, #2140, #25823, #34355, #17120, #11234, #31510, #7841, #8215, #10673, #28475, #5168, #22990, #37370, #19599, #31149, #30775, #37004, #5533, #13522, #13720, #7655, #22252, #2696, #2514, #36820, #22806, #19968, #14272, #19413, #8400, #22623, #28658, #19232, #14085, #11047, #16746, #5355, #28293, #11423, #25635, #4798, #2332, #34170, #16376 ),
 ( #37191, #19790, #25079, #27921, #33804, #30963, #4981, #16563, #16933, #28109, #31327, #25268, #33982, #10862, #22435, #8025, #3637, #786, #15206, #5723, #14638, #26755, #3444, #6293, #23736, #3070, #12356, #20709, #23176, #11790, #35275, #8766, #34540, #18057, #17304, #8579, #9330, #29216, #20340, #20901, #15013, #26565, #593, #32252, #32068, #28845, #23358, #12163, #37, #6486, #34910, #26008, #29600, #20148, #3258, #26376, #17868, #29026, #17491, #14832, #31882, #26189, #227, #20526, #8954, #31694, #6096, #2879, #32442, #410, #23548, #11975, #35094, #14452, #11602, #17679, #34721, #5912, #9143, #29413, #26945, #10080, #35660, #1165, #6863, #1542, #27326, #29789, #4200, #24490, #7061, #13112, #4386, #24668, #974, #33204, #12926, #12737, #35469, #18632, #36219, #30172, #18245, #9707, #3820, #15964, #15777, #1354, #23928, #27517, #18818, #7244, #36036, #27138, #15584, #15398, #24304, #35847, #4010, #9521, #29980, #30362, #32633, #12551, #6671, #21093, #24117, #21283, #32819, #21650, #18439, #9889, #21472, #33012, #18920, #32738, #6774, #24033, #12837, #10368, #13031, #24771, #27617, #9991, #36321, #21199, #21385, #27056, #33307, #35952, #7347, #30471, #1082, #7162, #18547, #24217, #15881, #30276, #27243, #1266, #24587, #16069, #9807, #15692, #21943, #4492, #1648, #4302, #33488, #21572, #24404, #12652, #1458, #33118, #32925, #26864, #7533, #3928, #15501, #19106, #18735, #6977, #13220, #35762, #35578, #27425, #4119, #9622, #36139, #10180, #21756, #18349, #29897 ),
 ( #30657, #4672, #30086, #893, #12464, #27987, #36698, #33863, #2201, #7905, #31570, #25329, #27805, #22688, #22499, #5235, #34046, #19666, #13402, #34417, #5047, #34232, #8275, #36878, #8455, #4861, #19848, #13594, #13781, #19478, #20024, #13963, #33676, #2389, #31390, #31206, #16255, #25699, #1833, #16441, #5410, #11112, #10924, #24951, #16811, #36509, #28352, #22129, #10738, #7716, #37251, #25512, #37065, #10553, #16992, #19298, #30837, #2016, #25144, #8093, #28532, #2575, #14146, #22311, #11299, #31025, #16629, #22867, #28171, #14886, #9388, #20580, #652, #31939, #20962, #17923, #26068, #12222, #5592, #23793, #14329, #23234, #35332, #12035, #26433, #32312, #11658, #17179, #29275, #31755, #20398, #6354, #17365, #28720, #26622, #25883, #2757, #29468, #281, #28906, #3504, #23603, #35148, #9200, #3314, #3129, #37431, #5971, #20768, #8638, #15072, #17551, #34595, #11481, #23051, #11847, #34967, #467, #96, #34782, #23416, #2942, #8826, #29087, #14696, #26245, #20206, #9010, #5785, #14512, #32124, #6161, #17734, #35900, #29656, #13164, #21337, #12982, #24538, #4068, #24719, #21147, #36088, #29842, #30034, #12603, #36271, #30226, #12413, #18685, #10132, #9943, #10315, #4438, #32494, #32685, #21705, #27376, #15640, #6541, #21523, #18114, #7114, #842, #15452, #23985, #16019, #33070, #4252, #3692, #7294, #33255, #18868, #24358, #32876, #9761, #15260, #6923, #15826, #1406, #35529, #26813, #24167, #9573, #30416, #27567, #1596, #1031, #6729, #18302, #3878, #18494, #27004 ) ),
 .UNSPECIFIED., .T., .F., .F. ) 
 B_SPLINE_SURFACE_WITH_KNOTS ( ( 4, 3, 4 ),
 ( 3, 2, 2, 2, 2, 2, 2, 2, 2, 2, 2, 2, 2, 2, 2, 2, 2, 2, 2, 2, 2, 2, 2, 2, 2, 2, 2, 2, 2, 2, 2, 2, 2, 2, 2, 2, 2, 2, 2, 2, 2, 2, 2, 2, 2, 2, 2, 2, 2, 2, 2, 2, 2, 2, 2, 2, 2, 2, 2, 2, 2, 2, 2, 2, 2, 2, 2, 2, 2, 2, 2, 2, 2, 2, 2, 2, 2, 2, 2, 2, 2, 2, 2, 2, 2, 2, 2, 2, 2, 2, 2, 2, 2, 2, 2, 2, 3 ),
 ( 0.000000000000000000, 0.5000000000000000000, 1.000000000000000000 ),
 ( 0.000000000000000000, 0.01041666666666666609, 0.02083333333333333218, 0.03125000000000000000, 0.04166666666666666435, 0.05208333333333333565, 0.06250000000000000000, 0.07291666666666667129, 0.08333333333333332871, 0.09375000000000000000, 0.1041666666666666713, 0.1145833333333333287, 0.1250000000000000000, 0.1354166666666666574, 0.1458333333333333426, 0.1562500000000000000, 0.1666666666666666574, 0.1770833333333333426, 0.1875000000000000000, 0.1979166666666666574, 0.2083333333333333426, 0.2187500000000000000, 0.2291666666666666574, 0.2395833333333333426, 0.2500000000000000000, 0.2604166666666666852, 0.2708333333333333148, 0.2812500000000000000, 0.2916666666666666852, 0.3020833333333333148, 0.3125000000000000000, 0.3229166666666666852, 0.3333333333333333148, 0.3437500000000000000, 0.3541666666666666852, 0.3645833333333333148, 0.3750000000000000000, 0.3854166666666666852, 0.3958333333333333148, 0.4062500000000000000, 0.4166666666666666852, 0.4270833333333333148, 0.4375000000000000000, 0.4479166666666666852, 0.4583333333333333148, 0.4687500000000000000, 0.4791666666666666852, 0.4895833333333333148, 0.5000000000000000000, 0.5104166666666666297, 0.5208333333333333703, 0.5312500000000000000, 0.5416666666666666297, 0.5520833333333333703, 0.5625000000000000000, 0.5729166666666666297, 0.5833333333333333703, 0.5937500000000000000, 0.6041666666666666297, 0.6145833333333333703, 0.6250000000000000000, 0.6354166666666666297, 0.6458333333333333703, 0.6562500000000000000, 0.6666666666666666297, 0.6770833333333333703, 0.6875000000000000000, 0.6979166666666666297, 0.7083333333333333703, 0.7187500000000000000, 0.7291666666666666297, 0.7395833333333333703, 0.7500000000000000000, 0.7604166666666666297, 0.7708333333333333703, 0.7812500000000000000, 0.7916666666666666297, 0.8020833333333333703, 0.8125000000000000000, 0.8229166666666666297, 0.8333333333333333703, 0.8437500000000000000, 0.8541666666666666297, 0.8645833333333333703, 0.8750000000000000000, 0.8854166666666666297, 0.8958333333333333703, 0.9062500000000000000, 0.9166666666666666297, 0.9270833333333333703, 0.9375000000000000000, 0.9479166666666666297, 0.9583333333333333703, 0.9687500000000000000, 0.9791666666666666297, 0.9895833333333333703, 1.000000000000000000 ),
 .UNSPECIFIED. ) 
 GEOMETRIC_REPRESENTATION_ITEM ( )  RATIONAL_B_SPLINE_SURFACE ( (
 ( 1.000000000000000000, 0.9659258262890683122, 1.000000000000000000, 0.9659258262890683122, 1.000000000000000000, 0.9659258262890683122, 1.000000000000000000, 0.9659258262890683122, 1.000000000000000000, 0.9659258262890683122, 1.000000000000000000, 0.9659258262890683122, 1.000000000000000000, 0.9659258262890683122, 1.000000000000000000, 0.9659258262890683122, 1.000000000000000000, 0.9659258262890683122, 1.000000000000000000, 0.9659258262890683122, 1.000000000000000000, 0.9659258262890683122, 1.000000000000000000, 0.9659258262890683122, 1.000000000000000000, 0.9659258262890683122, 1.000000000000000000, 0.9659258262890683122, 1.000000000000000000, 0.9659258262890683122, 1.000000000000000000, 0.9659258262890683122, 1.000000000000000000, 0.9659258262890683122, 1.000000000000000000, 0.9659258262890683122, 1.000000000000000000, 0.9659258262890683122, 1.000000000000000000, 0.9659258262890683122, 1.000000000000000000, 0.9659258262890683122, 1.000000000000000000, 0.9659258262890683122, 1.000000000000000000, 0.9659258262890683122, 1.000000000000000000, 0.9659258262890683122, 1.000000000000000000, 0.9659258262890683122, 1.000000000000000000, 0.9659258262890683122, 1.000000000000000000, 0.9659258262890683122, 1.000000000000000000, 0.9659258262890683122, 1.000000000000000000, 0.9659258262890683122, 1.000000000000000000, 0.9659258262890683122, 1.000000000000000000, 0.9659258262890683122, 1.000000000000000000, 0.9659258262890683122, 1.000000000000000000, 0.9659258262890683122, 1.000000000000000000, 0.9659258262890683122, 1.000000000000000000, 0.9659258262890683122, 1.000000000000000000, 0.9659258262890683122, 1.000000000000000000, 0.9659258262890683122, 1.000000000000000000, 0.9659258262890683122, 1.000000000000000000, 0.9659258262890683122, 1.000000000000000000, 0.9659258262890683122, 1.000000000000000000, 0.9659258262890683122, 1.000000000000000000, 0.9659258262890683122, 1.000000000000000000, 0.9659258262890683122, 1.000000000000000000, 0.9659258262890683122, 1.000000000000000000, 0.9659258262890683122, 1.000000000000000000, 0.9659258262890683122, 1.000000000000000000, 0.9659258262890683122, 1.000000000000000000, 0.9659258262890683122, 1.000000000000000000, 0.9659258262890683122, 1.000000000000000000, 0.9659258262890683122, 1.000000000000000000, 0.9659258262890683122, 1.000000000000000000, 0.9659258262890683122, 1.000000000000000000, 0.9659258262890683122, 1.000000000000000000, 0.9659258262890683122, 1.000000000000000000, 0.9659258262890683122, 1.000000000000000000, 0.9659258262890683122, 1.000000000000000000, 0.9659258262890683122, 1.000000000000000000, 0.9659258262890683122, 1.000000000000000000, 0.9659258262890683122, 1.000000000000000000, 0.9659258262890683122, 1.000000000000000000, 0.9659258262890683122, 1.000000000000000000, 0.9659258262890683122, 1.000000000000000000, 0.9659258262890683122, 1.000000000000000000, 0.9659258262890683122, 1.000000000000000000, 0.9659258262890683122, 1.000000000000000000, 0.9659258262890683122, 1.000000000000000000, 0.9659258262890683122, 1.000000000000000000, 0.9659258262890683122, 1.000000000000000000, 0.9659258262890683122, 1.000000000000000000, 0.9659258262890683122, 1.000000000000000000, 0.9659258262890683122, 1.000000000000000000, 0.9659258262890683122, 1.000000000000000000, 0.9659258262890683122, 1.000000000000000000, 0.9659258262890683122, 1.000000000000000000, 0.9659258262890683122, 1.000000000000000000, 0.9659258262890683122, 1.000000000000000000, 0.9659258262890683122, 1.000000000000000000, 0.9659258262890683122, 1.000000000000000000, 0.9659258262890683122, 1.000000000000000000, 0.9659258262890683122, 1.000000000000000000, 0.9659258262890683122, 1.000000000000000000, 0.9659258262890683122, 1.000000000000000000, 0.9659258262890683122, 1.000000000000000000, 0.9659258262890683122, 1.000000000000000000, 0.9659258262890683122, 1.000000000000000000, 0.9659258262890683122, 1.000000000000000000, 0.9659258262890683122, 1.000000000000000000, 0.9659258262890683122, 1.000000000000000000, 0.9659258262890683122, 1.000000000000000000, 0.9659258262890683122, 1.000000000000000000, 0.9659258262890683122, 1.000000000000000000, 0.9659258262890683122, 1.000000000000000000, 0.9659258262890683122, 1.000000000000000000, 0.9659258262890683122, 1.000000000000000000, 0.9659258262890683122, 1.000000000000000000, 0.9659258262890683122, 1.000000000000000000),
 ( 0.3333333333333333703, 0.3219752754296894559, 0.3333333333333333703, 0.3219752754296894559, 0.3333333333333333703, 0.3219752754296894559, 0.3333333333333333703, 0.3219752754296894559, 0.3333333333333333703, 0.3219752754296894559, 0.3333333333333333703, 0.3219752754296894559, 0.3333333333333333703, 0.3219752754296894559, 0.3333333333333333703, 0.3219752754296894559, 0.3333333333333333703, 0.3219752754296894559, 0.3333333333333333703, 0.3219752754296894559, 0.3333333333333333703, 0.3219752754296894559, 0.3333333333333333703, 0.3219752754296894559, 0.3333333333333333703, 0.3219752754296894559, 0.3333333333333333703, 0.3219752754296894559, 0.3333333333333333703, 0.3219752754296894559, 0.3333333333333333703, 0.3219752754296894559, 0.3333333333333333703, 0.3219752754296894559, 0.3333333333333333703, 0.3219752754296894559, 0.3333333333333333703, 0.3219752754296894559, 0.3333333333333333703, 0.3219752754296894559, 0.3333333333333333703, 0.3219752754296894559, 0.3333333333333333703, 0.3219752754296894559, 0.3333333333333333703, 0.3219752754296894559, 0.3333333333333333703, 0.3219752754296894559, 0.3333333333333333703, 0.3219752754296894559, 0.3333333333333333703, 0.3219752754296894559, 0.3333333333333333703, 0.3219752754296894559, 0.3333333333333333703, 0.3219752754296894559, 0.3333333333333333703, 0.3219752754296894559, 0.3333333333333333703, 0.3219752754296894559, 0.3333333333333333703, 0.3219752754296894559, 0.3333333333333333703, 0.3219752754296894559, 0.3333333333333333703, 0.3219752754296894559, 0.3333333333333333703, 0.3219752754296894559, 0.3333333333333333703, 0.3219752754296894559, 0.3333333333333333703, 0.3219752754296894559, 0.3333333333333333703, 0.3219752754296894559, 0.3333333333333333703, 0.3219752754296894559, 0.3333333333333333703, 0.3219752754296894559, 0.3333333333333333703, 0.3219752754296894559, 0.3333333333333333703, 0.3219752754296894559, 0.3333333333333333703, 0.3219752754296894559, 0.3333333333333333703, 0.3219752754296894559, 0.3333333333333333703, 0.3219752754296894559, 0.3333333333333333703, 0.3219752754296894559, 0.3333333333333333703, 0.3219752754296894559, 0.3333333333333333703, 0.3219752754296894559, 0.3333333333333333703, 0.3219752754296894559, 0.3333333333333333703, 0.3219752754296894559, 0.3333333333333333703, 0.3219752754296894559, 0.3333333333333333703, 0.3219752754296894559, 0.3333333333333333703, 0.3219752754296894559, 0.3333333333333333703, 0.3219752754296894559, 0.3333333333333333703, 0.3219752754296894559, 0.3333333333333333703, 0.3219752754296894559, 0.3333333333333333703, 0.3219752754296894559, 0.3333333333333333703, 0.3219752754296894559, 0.3333333333333333703, 0.3219752754296894559, 0.3333333333333333703, 0.3219752754296894559, 0.3333333333333333703, 0.3219752754296894559, 0.3333333333333333703, 0.3219752754296894559, 0.3333333333333333703, 0.3219752754296894559, 0.3333333333333333703, 0.3219752754296894559, 0.3333333333333333703, 0.3219752754296894559, 0.3333333333333333703, 0.3219752754296894559, 0.3333333333333333703, 0.3219752754296894559, 0.3333333333333333703, 0.3219752754296894559, 0.3333333333333333703, 0.3219752754296894559, 0.3333333333333333703, 0.3219752754296894559, 0.3333333333333333703, 0.3219752754296894559, 0.3333333333333333703, 0.3219752754296894559, 0.3333333333333333703, 0.3219752754296894559, 0.3333333333333333703, 0.3219752754296894559, 0.3333333333333333703, 0.3219752754296894559, 0.3333333333333333703, 0.3219752754296894559, 0.3333333333333333703, 0.3219752754296894559, 0.3333333333333333703, 0.3219752754296894559, 0.3333333333333333703, 0.3219752754296894559, 0.3333333333333333703, 0.3219752754296894559, 0.3333333333333333703, 0.3219752754296894559, 0.3333333333333333703, 0.3219752754296894559, 0.3333333333333333703, 0.3219752754296894559, 0.3333333333333333703, 0.3219752754296894559, 0.3333333333333333703, 0.3219752754296894559, 0.3333333333333333703, 0.3219752754296894559, 0.3333333333333333703, 0.3219752754296894559, 0.3333333333333333703, 0.3219752754296894559, 0.3333333333333333703, 0.3219752754296894559, 0.3333333333333333703, 0.3219752754296894559, 0.3333333333333333703, 0.3219752754296894559, 0.3333333333333333703, 0.3219752754296894559, 0.3333333333333333703, 0.3219752754296894559, 0.3333333333333333703, 0.3219752754296894559, 0.3333333333333333703, 0.3219752754296894559, 0.3333333333333333703, 0.3219752754296894559, 0.3333333333333333703, 0.3219752754296894559, 0.3333333333333333703),
 ( 0.3333333333333333703, 0.3219752754296894559, 0.3333333333333333703, 0.3219752754296894559, 0.3333333333333333703, 0.3219752754296894559, 0.3333333333333333703, 0.3219752754296894559, 0.3333333333333333703, 0.3219752754296894559, 0.3333333333333333703, 0.3219752754296894559, 0.3333333333333333703, 0.3219752754296894559, 0.3333333333333333703, 0.3219752754296894559, 0.3333333333333333703, 0.3219752754296894559, 0.3333333333333333703, 0.3219752754296894559, 0.3333333333333333703, 0.3219752754296894559, 0.3333333333333333703, 0.3219752754296894559, 0.3333333333333333703, 0.3219752754296894559, 0.3333333333333333703, 0.3219752754296894559, 0.3333333333333333703, 0.3219752754296894559, 0.3333333333333333703, 0.3219752754296894559, 0.3333333333333333703, 0.3219752754296894559, 0.3333333333333333703, 0.3219752754296894559, 0.3333333333333333703, 0.3219752754296894559, 0.3333333333333333703, 0.3219752754296894559, 0.3333333333333333703, 0.3219752754296894559, 0.3333333333333333703, 0.3219752754296894559, 0.3333333333333333703, 0.3219752754296894559, 0.3333333333333333703, 0.3219752754296894559, 0.3333333333333333703, 0.3219752754296894559, 0.3333333333333333703, 0.3219752754296894559, 0.3333333333333333703, 0.3219752754296894559, 0.3333333333333333703, 0.3219752754296894559, 0.3333333333333333703, 0.3219752754296894559, 0.3333333333333333703, 0.3219752754296894559, 0.3333333333333333703, 0.3219752754296894559, 0.3333333333333333703, 0.3219752754296894559, 0.3333333333333333703, 0.3219752754296894559, 0.3333333333333333703, 0.3219752754296894559, 0.3333333333333333703, 0.3219752754296894559, 0.3333333333333333703, 0.3219752754296894559, 0.3333333333333333703, 0.3219752754296894559, 0.3333333333333333703, 0.3219752754296894559, 0.3333333333333333703, 0.3219752754296894559, 0.3333333333333333703, 0.3219752754296894559, 0.3333333333333333703, 0.3219752754296894559, 0.3333333333333333703, 0.3219752754296894559, 0.3333333333333333703, 0.3219752754296894559, 0.3333333333333333703, 0.3219752754296894559, 0.3333333333333333703, 0.3219752754296894559, 0.3333333333333333703, 0.3219752754296894559, 0.3333333333333333703, 0.3219752754296894559, 0.3333333333333333703, 0.3219752754296894559, 0.3333333333333333703, 0.3219752754296894559, 0.3333333333333333703, 0.3219752754296894559, 0.3333333333333333703, 0.3219752754296894559, 0.3333333333333333703, 0.3219752754296894559, 0.3333333333333333703, 0.3219752754296894559, 0.3333333333333333703, 0.3219752754296894559, 0.3333333333333333703, 0.3219752754296894559, 0.3333333333333333703, 0.3219752754296894559, 0.3333333333333333703, 0.3219752754296894559, 0.3333333333333333703, 0.3219752754296894559, 0.3333333333333333703, 0.3219752754296894559, 0.3333333333333333703, 0.3219752754296894559, 0.3333333333333333703, 0.3219752754296894559, 0.3333333333333333703, 0.3219752754296894559, 0.3333333333333333703, 0.3219752754296894559, 0.3333333333333333703, 0.3219752754296894559, 0.3333333333333333703, 0.3219752754296894559, 0.3333333333333333703, 0.3219752754296894559, 0.3333333333333333703, 0.3219752754296894559, 0.3333333333333333703, 0.3219752754296894559, 0.3333333333333333703, 0.3219752754296894559, 0.3333333333333333703, 0.3219752754296894559, 0.3333333333333333703, 0.3219752754296894559, 0.3333333333333333703, 0.3219752754296894559, 0.3333333333333333703, 0.3219752754296894559, 0.3333333333333333703, 0.3219752754296894559, 0.3333333333333333703, 0.3219752754296894559, 0.3333333333333333703, 0.3219752754296894559, 0.3333333333333333703, 0.3219752754296894559, 0.3333333333333333703, 0.3219752754296894559, 0.3333333333333333703, 0.3219752754296894559, 0.3333333333333333703, 0.3219752754296894559, 0.3333333333333333703, 0.3219752754296894559, 0.3333333333333333703, 0.3219752754296894559, 0.3333333333333333703, 0.3219752754296894559, 0.3333333333333333703, 0.3219752754296894559, 0.3333333333333333703, 0.3219752754296894559, 0.3333333333333333703, 0.3219752754296894559, 0.3333333333333333703, 0.3219752754296894559, 0.3333333333333333703, 0.3219752754296894559, 0.3333333333333333703, 0.3219752754296894559, 0.3333333333333333703, 0.3219752754296894559, 0.3333333333333333703, 0.3219752754296894559, 0.3333333333333333703, 0.3219752754296894559, 0.3333333333333333703, 0.3219752754296894559, 0.3333333333333333703, 0.3219752754296894559, 0.3333333333333333703, 0.3219752754296894559, 0.3333333333333333703, 0.3219752754296894559, 0.3333333333333333703),
 ( 1.000000000000000000, 0.9659258262890683122, 1.000000000000000000, 0.9659258262890683122, 1.000000000000000000, 0.9659258262890683122, 1.000000000000000000, 0.9659258262890683122, 1.000000000000000000, 0.9659258262890683122, 1.000000000000000000, 0.9659258262890683122, 1.000000000000000000, 0.9659258262890683122, 1.000000000000000000, 0.9659258262890683122, 1.000000000000000000, 0.9659258262890683122, 1.000000000000000000, 0.9659258262890683122, 1.000000000000000000, 0.9659258262890683122, 1.000000000000000000, 0.9659258262890683122, 1.000000000000000000, 0.9659258262890683122, 1.000000000000000000, 0.9659258262890683122, 1.000000000000000000, 0.9659258262890683122, 1.000000000000000000, 0.9659258262890683122, 1.000000000000000000, 0.9659258262890683122, 1.000000000000000000, 0.9659258262890683122, 1.000000000000000000, 0.9659258262890683122, 1.000000000000000000, 0.9659258262890683122, 1.000000000000000000, 0.9659258262890683122, 1.000000000000000000, 0.9659258262890683122, 1.000000000000000000, 0.9659258262890683122, 1.000000000000000000, 0.9659258262890683122, 1.000000000000000000, 0.9659258262890683122, 1.000000000000000000, 0.9659258262890683122, 1.000000000000000000, 0.9659258262890683122, 1.000000000000000000, 0.9659258262890683122, 1.000000000000000000, 0.9659258262890683122, 1.000000000000000000, 0.9659258262890683122, 1.000000000000000000, 0.9659258262890683122, 1.000000000000000000, 0.9659258262890683122, 1.000000000000000000, 0.9659258262890683122, 1.000000000000000000, 0.9659258262890683122, 1.000000000000000000, 0.9659258262890683122, 1.000000000000000000, 0.9659258262890683122, 1.000000000000000000, 0.9659258262890683122, 1.000000000000000000, 0.9659258262890683122, 1.000000000000000000, 0.9659258262890683122, 1.000000000000000000, 0.9659258262890683122, 1.000000000000000000, 0.9659258262890683122, 1.000000000000000000, 0.9659258262890683122, 1.000000000000000000, 0.9659258262890683122, 1.000000000000000000, 0.9659258262890683122, 1.000000000000000000, 0.9659258262890683122, 1.000000000000000000, 0.9659258262890683122, 1.000000000000000000, 0.9659258262890683122, 1.000000000000000000, 0.9659258262890683122, 1.000000000000000000, 0.9659258262890683122, 1.000000000000000000, 0.9659258262890683122, 1.000000000000000000, 0.9659258262890683122, 1.000000000000000000, 0.9659258262890683122, 1.000000000000000000, 0.9659258262890683122, 1.000000000000000000, 0.9659258262890683122, 1.000000000000000000, 0.9659258262890683122, 1.000000000000000000, 0.9659258262890683122, 1.000000000000000000, 0.9659258262890683122, 1.000000000000000000, 0.9659258262890683122, 1.000000000000000000, 0.9659258262890683122, 1.000000000000000000, 0.9659258262890683122, 1.000000000000000000, 0.9659258262890683122, 1.000000000000000000, 0.9659258262890683122, 1.000000000000000000, 0.9659258262890683122, 1.000000000000000000, 0.9659258262890683122, 1.000000000000000000, 0.9659258262890683122, 1.000000000000000000, 0.9659258262890683122, 1.000000000000000000, 0.9659258262890683122, 1.000000000000000000, 0.9659258262890683122, 1.000000000000000000, 0.9659258262890683122, 1.000000000000000000, 0.9659258262890683122, 1.000000000000000000, 0.9659258262890683122, 1.000000000000000000, 0.9659258262890683122, 1.000000000000000000, 0.9659258262890683122, 1.000000000000000000, 0.9659258262890683122, 1.000000000000000000, 0.9659258262890683122, 1.000000000000000000, 0.9659258262890683122, 1.000000000000000000, 0.9659258262890683122, 1.000000000000000000, 0.9659258262890683122, 1.000000000000000000, 0.9659258262890683122, 1.000000000000000000, 0.9659258262890683122, 1.000000000000000000, 0.9659258262890683122, 1.000000000000000000, 0.9659258262890683122, 1.000000000000000000, 0.9659258262890683122, 1.000000000000000000, 0.9659258262890683122, 1.000000000000000000, 0.9659258262890683122, 1.000000000000000000, 0.9659258262890683122, 1.000000000000000000, 0.9659258262890683122, 1.000000000000000000, 0.9659258262890683122, 1.000000000000000000, 0.9659258262890683122, 1.000000000000000000, 0.9659258262890683122, 1.000000000000000000, 0.9659258262890683122, 1.000000000000000000, 0.9659258262890683122, 1.000000000000000000, 0.9659258262890683122, 1.000000000000000000, 0.9659258262890683122, 1.000000000000000000, 0.9659258262890683122, 1.000000000000000000, 0.9659258262890683122, 1.000000000000000000),
 ( 0.3333333333333333703, 0.3219752754296894559, 0.3333333333333333703, 0.3219752754296894559, 0.3333333333333333703, 0.3219752754296894559, 0.3333333333333333703, 0.3219752754296894559, 0.3333333333333333703, 0.3219752754296894559, 0.3333333333333333703, 0.3219752754296894559, 0.3333333333333333703, 0.3219752754296894559, 0.3333333333333333703, 0.3219752754296894559, 0.3333333333333333703, 0.3219752754296894559, 0.3333333333333333703, 0.3219752754296894559, 0.3333333333333333703, 0.3219752754296894559, 0.3333333333333333703, 0.3219752754296894559, 0.3333333333333333703, 0.3219752754296894559, 0.3333333333333333703, 0.3219752754296894559, 0.3333333333333333703, 0.3219752754296894559, 0.3333333333333333703, 0.3219752754296894559, 0.3333333333333333703, 0.3219752754296894559, 0.3333333333333333703, 0.3219752754296894559, 0.3333333333333333703, 0.3219752754296894559, 0.3333333333333333703, 0.3219752754296894559, 0.3333333333333333703, 0.3219752754296894559, 0.3333333333333333703, 0.3219752754296894559, 0.3333333333333333703, 0.3219752754296894559, 0.3333333333333333703, 0.3219752754296894559, 0.3333333333333333703, 0.3219752754296894559, 0.3333333333333333703, 0.3219752754296894559, 0.3333333333333333703, 0.3219752754296894559, 0.3333333333333333703, 0.3219752754296894559, 0.3333333333333333703, 0.3219752754296894559, 0.3333333333333333703, 0.3219752754296894559, 0.3333333333333333703, 0.3219752754296894559, 0.3333333333333333703, 0.3219752754296894559, 0.3333333333333333703, 0.3219752754296894559, 0.3333333333333333703, 0.3219752754296894559, 0.3333333333333333703, 0.3219752754296894559, 0.3333333333333333703, 0.3219752754296894559, 0.3333333333333333703, 0.3219752754296894559, 0.3333333333333333703, 0.3219752754296894559, 0.3333333333333333703, 0.3219752754296894559, 0.3333333333333333703, 0.3219752754296894559, 0.3333333333333333703, 0.3219752754296894559, 0.3333333333333333703, 0.3219752754296894559, 0.3333333333333333703, 0.3219752754296894559, 0.3333333333333333703, 0.3219752754296894559, 0.3333333333333333703, 0.3219752754296894559, 0.3333333333333333703, 0.3219752754296894559, 0.3333333333333333703, 0.3219752754296894559, 0.3333333333333333703, 0.3219752754296894559, 0.3333333333333333703, 0.3219752754296894559, 0.3333333333333333703, 0.3219752754296894559, 0.3333333333333333703, 0.3219752754296894559, 0.3333333333333333703, 0.3219752754296894559, 0.3333333333333333703, 0.3219752754296894559, 0.3333333333333333703, 0.3219752754296894559, 0.3333333333333333703, 0.3219752754296894559, 0.3333333333333333703, 0.3219752754296894559, 0.3333333333333333703, 0.3219752754296894559, 0.3333333333333333703, 0.3219752754296894559, 0.3333333333333333703, 0.3219752754296894559, 0.3333333333333333703, 0.3219752754296894559, 0.3333333333333333703, 0.3219752754296894559, 0.3333333333333333703, 0.3219752754296894559, 0.3333333333333333703, 0.3219752754296894559, 0.3333333333333333703, 0.3219752754296894559, 0.3333333333333333703, 0.3219752754296894559, 0.3333333333333333703, 0.3219752754296894559, 0.3333333333333333703, 0.3219752754296894559, 0.3333333333333333703, 0.3219752754296894559, 0.3333333333333333703, 0.3219752754296894559, 0.3333333333333333703, 0.3219752754296894559, 0.3333333333333333703, 0.3219752754296894559, 0.3333333333333333703, 0.3219752754296894559, 0.3333333333333333703, 0.3219752754296894559, 0.3333333333333333703, 0.3219752754296894559, 0.3333333333333333703, 0.3219752754296894559, 0.3333333333333333703, 0.3219752754296894559, 0.3333333333333333703, 0.3219752754296894559, 0.3333333333333333703, 0.3219752754296894559, 0.3333333333333333703, 0.3219752754296894559, 0.3333333333333333703, 0.3219752754296894559, 0.3333333333333333703, 0.3219752754296894559, 0.3333333333333333703, 0.3219752754296894559, 0.3333333333333333703, 0.3219752754296894559, 0.3333333333333333703, 0.3219752754296894559, 0.3333333333333333703, 0.3219752754296894559, 0.3333333333333333703, 0.3219752754296894559, 0.3333333333333333703, 0.3219752754296894559, 0.3333333333333333703, 0.3219752754296894559, 0.3333333333333333703, 0.3219752754296894559, 0.3333333333333333703, 0.3219752754296894559, 0.3333333333333333703, 0.3219752754296894559, 0.3333333333333333703, 0.3219752754296894559, 0.3333333333333333703, 0.3219752754296894559, 0.3333333333333333703, 0.3219752754296894559, 0.3333333333333333703, 0.3219752754296894559, 0.3333333333333333703, 0.3219752754296894559, 0.3333333333333333703),
 ( 0.3333333333333333703, 0.3219752754296894559, 0.3333333333333333703, 0.3219752754296894559, 0.3333333333333333703, 0.3219752754296894559, 0.3333333333333333703, 0.3219752754296894559, 0.3333333333333333703, 0.3219752754296894559, 0.3333333333333333703, 0.3219752754296894559, 0.3333333333333333703, 0.3219752754296894559, 0.3333333333333333703, 0.3219752754296894559, 0.3333333333333333703, 0.3219752754296894559, 0.3333333333333333703, 0.3219752754296894559, 0.3333333333333333703, 0.3219752754296894559, 0.3333333333333333703, 0.3219752754296894559, 0.3333333333333333703, 0.3219752754296894559, 0.3333333333333333703, 0.3219752754296894559, 0.3333333333333333703, 0.3219752754296894559, 0.3333333333333333703, 0.3219752754296894559, 0.3333333333333333703, 0.3219752754296894559, 0.3333333333333333703, 0.3219752754296894559, 0.3333333333333333703, 0.3219752754296894559, 0.3333333333333333703, 0.3219752754296894559, 0.3333333333333333703, 0.3219752754296894559, 0.3333333333333333703, 0.3219752754296894559, 0.3333333333333333703, 0.3219752754296894559, 0.3333333333333333703, 0.3219752754296894559, 0.3333333333333333703, 0.3219752754296894559, 0.3333333333333333703, 0.3219752754296894559, 0.3333333333333333703, 0.3219752754296894559, 0.3333333333333333703, 0.3219752754296894559, 0.3333333333333333703, 0.3219752754296894559, 0.3333333333333333703, 0.3219752754296894559, 0.3333333333333333703, 0.3219752754296894559, 0.3333333333333333703, 0.3219752754296894559, 0.3333333333333333703, 0.3219752754296894559, 0.3333333333333333703, 0.3219752754296894559, 0.3333333333333333703, 0.3219752754296894559, 0.3333333333333333703, 0.3219752754296894559, 0.3333333333333333703, 0.3219752754296894559, 0.3333333333333333703, 0.3219752754296894559, 0.3333333333333333703, 0.3219752754296894559, 0.3333333333333333703, 0.3219752754296894559, 0.3333333333333333703, 0.3219752754296894559, 0.3333333333333333703, 0.3219752754296894559, 0.3333333333333333703, 0.3219752754296894559, 0.3333333333333333703, 0.3219752754296894559, 0.3333333333333333703, 0.3219752754296894559, 0.3333333333333333703, 0.3219752754296894559, 0.3333333333333333703, 0.3219752754296894559, 0.3333333333333333703, 0.3219752754296894559, 0.3333333333333333703, 0.3219752754296894559, 0.3333333333333333703, 0.3219752754296894559, 0.3333333333333333703, 0.3219752754296894559, 0.3333333333333333703, 0.3219752754296894559, 0.3333333333333333703, 0.3219752754296894559, 0.3333333333333333703, 0.3219752754296894559, 0.3333333333333333703, 0.3219752754296894559, 0.3333333333333333703, 0.3219752754296894559, 0.3333333333333333703, 0.3219752754296894559, 0.3333333333333333703, 0.3219752754296894559, 0.3333333333333333703, 0.3219752754296894559, 0.3333333333333333703, 0.3219752754296894559, 0.3333333333333333703, 0.3219752754296894559, 0.3333333333333333703, 0.3219752754296894559, 0.3333333333333333703, 0.3219752754296894559, 0.3333333333333333703, 0.3219752754296894559, 0.3333333333333333703, 0.3219752754296894559, 0.3333333333333333703, 0.3219752754296894559, 0.3333333333333333703, 0.3219752754296894559, 0.3333333333333333703, 0.3219752754296894559, 0.3333333333333333703, 0.3219752754296894559, 0.3333333333333333703, 0.3219752754296894559, 0.3333333333333333703, 0.3219752754296894559, 0.3333333333333333703, 0.3219752754296894559, 0.3333333333333333703, 0.3219752754296894559, 0.3333333333333333703, 0.3219752754296894559, 0.3333333333333333703, 0.3219752754296894559, 0.3333333333333333703, 0.3219752754296894559, 0.3333333333333333703, 0.3219752754296894559, 0.3333333333333333703, 0.3219752754296894559, 0.3333333333333333703, 0.3219752754296894559, 0.3333333333333333703, 0.3219752754296894559, 0.3333333333333333703, 0.3219752754296894559, 0.3333333333333333703, 0.3219752754296894559, 0.3333333333333333703, 0.3219752754296894559, 0.3333333333333333703, 0.3219752754296894559, 0.3333333333333333703, 0.3219752754296894559, 0.3333333333333333703, 0.3219752754296894559, 0.3333333333333333703, 0.3219752754296894559, 0.3333333333333333703, 0.3219752754296894559, 0.3333333333333333703, 0.3219752754296894559, 0.3333333333333333703, 0.3219752754296894559, 0.3333333333333333703, 0.3219752754296894559, 0.3333333333333333703, 0.3219752754296894559, 0.3333333333333333703, 0.3219752754296894559, 0.3333333333333333703, 0.3219752754296894559, 0.3333333333333333703, 0.3219752754296894559, 0.3333333333333333703, 0.3219752754296894559, 0.3333333333333333703),
 ( 1.000000000000000000, 0.9659258262890683122, 1.000000000000000000, 0.9659258262890683122, 1.000000000000000000, 0.9659258262890683122, 1.000000000000000000, 0.9659258262890683122, 1.000000000000000000, 0.9659258262890683122, 1.000000000000000000, 0.9659258262890683122, 1.000000000000000000, 0.9659258262890683122, 1.000000000000000000, 0.9659258262890683122, 1.000000000000000000, 0.9659258262890683122, 1.000000000000000000, 0.9659258262890683122, 1.000000000000000000, 0.9659258262890683122, 1.000000000000000000, 0.9659258262890683122, 1.000000000000000000, 0.9659258262890683122, 1.000000000000000000, 0.9659258262890683122, 1.000000000000000000, 0.9659258262890683122, 1.000000000000000000, 0.9659258262890683122, 1.000000000000000000, 0.9659258262890683122, 1.000000000000000000, 0.9659258262890683122, 1.000000000000000000, 0.9659258262890683122, 1.000000000000000000, 0.9659258262890683122, 1.000000000000000000, 0.9659258262890683122, 1.000000000000000000, 0.9659258262890683122, 1.000000000000000000, 0.9659258262890683122, 1.000000000000000000, 0.9659258262890683122, 1.000000000000000000, 0.9659258262890683122, 1.000000000000000000, 0.9659258262890683122, 1.000000000000000000, 0.9659258262890683122, 1.000000000000000000, 0.9659258262890683122, 1.000000000000000000, 0.9659258262890683122, 1.000000000000000000, 0.9659258262890683122, 1.000000000000000000, 0.9659258262890683122, 1.000000000000000000, 0.9659258262890683122, 1.000000000000000000, 0.9659258262890683122, 1.000000000000000000, 0.9659258262890683122, 1.000000000000000000, 0.9659258262890683122, 1.000000000000000000, 0.9659258262890683122, 1.000000000000000000, 0.9659258262890683122, 1.000000000000000000, 0.9659258262890683122, 1.000000000000000000, 0.9659258262890683122, 1.000000000000000000, 0.9659258262890683122, 1.000000000000000000, 0.9659258262890683122, 1.000000000000000000, 0.9659258262890683122, 1.000000000000000000, 0.9659258262890683122, 1.000000000000000000, 0.9659258262890683122, 1.000000000000000000, 0.9659258262890683122, 1.000000000000000000, 0.9659258262890683122, 1.000000000000000000, 0.9659258262890683122, 1.000000000000000000, 0.9659258262890683122, 1.000000000000000000, 0.9659258262890683122, 1.000000000000000000, 0.9659258262890683122, 1.000000000000000000, 0.9659258262890683122, 1.000000000000000000, 0.9659258262890683122, 1.000000000000000000, 0.9659258262890683122, 1.000000000000000000, 0.9659258262890683122, 1.000000000000000000, 0.9659258262890683122, 1.000000000000000000, 0.9659258262890683122, 1.000000000000000000, 0.9659258262890683122, 1.000000000000000000, 0.9659258262890683122, 1.000000000000000000, 0.9659258262890683122, 1.000000000000000000, 0.9659258262890683122, 1.000000000000000000, 0.9659258262890683122, 1.000000000000000000, 0.9659258262890683122, 1.000000000000000000, 0.9659258262890683122, 1.000000000000000000, 0.9659258262890683122, 1.000000000000000000, 0.9659258262890683122, 1.000000000000000000, 0.9659258262890683122, 1.000000000000000000, 0.9659258262890683122, 1.000000000000000000, 0.9659258262890683122, 1.000000000000000000, 0.9659258262890683122, 1.000000000000000000, 0.9659258262890683122, 1.000000000000000000, 0.9659258262890683122, 1.000000000000000000, 0.9659258262890683122, 1.000000000000000000, 0.9659258262890683122, 1.000000000000000000, 0.9659258262890683122, 1.000000000000000000, 0.9659258262890683122, 1.000000000000000000, 0.9659258262890683122, 1.000000000000000000, 0.9659258262890683122, 1.000000000000000000, 0.9659258262890683122, 1.000000000000000000, 0.9659258262890683122, 1.000000000000000000, 0.9659258262890683122, 1.000000000000000000, 0.9659258262890683122, 1.000000000000000000, 0.9659258262890683122, 1.000000000000000000, 0.9659258262890683122, 1.000000000000000000, 0.9659258262890683122, 1.000000000000000000, 0.9659258262890683122, 1.000000000000000000, 0.9659258262890683122, 1.000000000000000000, 0.9659258262890683122, 1.000000000000000000, 0.9659258262890683122, 1.000000000000000000, 0.9659258262890683122, 1.000000000000000000, 0.9659258262890683122, 1.000000000000000000, 0.9659258262890683122, 1.000000000000000000, 0.9659258262890683122, 1.000000000000000000, 0.9659258262890683122, 1.000000000000000000, 0.9659258262890683122, 1.000000000000000000, 0.9659258262890683122, 1.000000000000000000, 0.9659258262890683122, 1.000000000000000000) ) ) 
 REPRESENTATION_ITEM ( '' )  SURFACE ( )  );
#1097 = CARTESIAN_POINT ( 'NONE',  ( -4.622313124798826500, 96.76481371789854791, 11.61527771782809637 ) ) ;
#1098 = CARTESIAN_POINT ( 'NONE',  ( 11.48171059495397728, 100.6851862821014691, 4.944772684328674117 ) ) ;
#1099 = ORIENTED_EDGE ( 'NONE', *, *, #4077, .T. ) ;
#1100 = VECTOR ( 'NONE', #32793, 1000.000000000000000 ) ;
#1101 = VERTEX_POINT ( 'NONE', #20197 ) ;
#1102 = CARTESIAN_POINT ( 'NONE',  ( 5.778771075727756162E-15, 195.4156250006145399, 31.45816453501075927 ) ) ;
#1103 = CARTESIAN_POINT ( 'NONE',  ( 18.12178482187499640, 239.7718750006145001, -4.985214923628404904 ) ) ;
#1104 = CARTESIAN_POINT ( 'NONE',  ( -0.1745138560722442889, 73.18981371789854506, -15.50000000000000533 ) ) ;
#1105 = CARTESIAN_POINT ( 'NONE',  ( 15.24356964374999990, 0.000000000000000000, -6.553124999385484983 ) ) ;
#1106 = CARTESIAN_POINT ( 'NONE',  ( 26.75643035624999655, 245.1718750006145058, -3.323476615752271712 ) ) ;
#1107 = CARTESIAN_POINT ( 'NONE',  ( 0.1745138560725194299, 97.81018628210145494, -9.500000000000005329 ) ) ;
#1108 = PLANE ( 'NONE',  #11917 ) ;
#1109 = EDGE_CURVE ( 'NONE', #28768, #2711, #7134, .T. ) ;
#1110 = CARTESIAN_POINT ( 'NONE',  ( 3.474262827703532341, 64.56481371789854506, -8.843639120294245259 ) ) ;
#1111 = CARTESIAN_POINT ( 'NONE',  ( 19.68408634441910721, -5.407089921784855591, -8.090624999385564564 ) ) ;
#1112 = VECTOR ( 'NONE', #33253, 1000.000000000000000 ) ;
#1113 = CARTESIAN_POINT ( 'NONE',  ( 9.534712964251900402, 121.7773137178985650, 1.715153634034445540 ) ) ;
#1114 = CARTESIAN_POINT ( 'NONE',  ( 27.24356964374999635, 199.6718750006145058, -15.72908226750539029 ) ) ;
#1115 = CARTESIAN_POINT ( 'NONE',  ( -4.944772684328424539, 35.81481371789854506, -11.48171059495408031 ) ) ;
#1116 = LINE ( 'NONE', #12682, #17619 ) ;
#1117 = CARTESIAN_POINT ( 'NONE',  ( 11.61527771782819940, 90.33518628210144641, -4.622313124798573369 ) ) ;
#1118 = CARTESIAN_POINT ( 'NONE',  ( 10.56230152254411614, -3.464101615137757051, -6.149999998770987020 ) ) ;
#1119 = CARTESIAN_POINT ( 'NONE',  ( 10.56230152254410903, 7.347880794884117764E-16, -10.00000000000000000 ) ) ;
#1120 = CARTESIAN_POINT ( 'NONE',  ( 31.08364707426076023, 7.209453229046475009, 165.2566134613956876 ) ) ;
#1121 = CARTESIAN_POINT ( 'NONE',  ( 10.31873187879410736, 0.000000000000000000, -3.346874999385518468 ) ) ;
#1122 = CARTESIAN_POINT ( 'NONE',  ( 4.944772684328679446, 6.385186282101440014, -11.48171059495397373 ) ) ;
#1123 = CARTESIAN_POINT ( 'NONE',  ( 10.49999999999999645, 252.0000000000000000, -2.499999999999999556 ) ) ;
#1124 = CARTESIAN_POINT ( 'NONE',  ( -27.00000000000000355, 199.0625000000000000, -15.58845726811989429 ) ) ;
#1125 = CARTESIAN_POINT ( 'NONE',  ( -8.710071997420127943, 105.2851862821014777, -3.796722387233380402 ) ) ;
#1126 = CARTESIAN_POINT ( 'NONE',  ( 15.00000000000000178, 248.2937500012290286, 3.464101615137757051 ) ) ;
#1127 = CARTESIAN_POINT ( 'NONE',  ( 4.622313124798573369, 129.4351862821014549, 11.61527771782819940 ) ) ;
#1128 = CARTESIAN_POINT ( 'NONE',  ( -13.62178482187500528, 195.2843750006145456, -23.59362340125807123 ) ) ;
#1129 = CARTESIAN_POINT ( 'NONE',  ( 19.00081571707366379, 239.7604221881839521, -5.492723647597353320 ) ) ;
#1130 = ORIENTED_EDGE ( 'NONE', *, *, #27910, .F. ) ;
#1131 = CARTESIAN_POINT ( 'NONE',  ( 34.37331128181295270, -5.407089921784855591, 167.0391835513610488 ) ) ;
#1132 = CARTESIAN_POINT ( 'NONE',  ( 26.75643035624999655, -3.323476615752267715, -3.103124999385467486 ) ) ;
#1133 = CARTESIAN_POINT ( 'NONE',  ( 26.78555467025737258, 0.1019468494213565390, -8.000000000000003553 ) ) ;
#1134 = CARTESIAN_POINT ( 'NONE',  ( 10.56230152254490484, 3.464101615138212242, -5.774999998771026988 ) ) ;
#1135 = CARTESIAN_POINT ( 'NONE',  ( 7.234628195640312676, 199.5299038117966859, -27.00000000000000711 ) ) ;
#1136 = CARTESIAN_POINT ( 'NONE',  ( 7.234628195640322446, 198.7825961894323257, 26.99999999999999645 ) ) ;
#1137 = CARTESIAN_POINT ( 'NONE',  ( 6.840914352311949109, 21.43981371789854506, 6.594114490232462877 ) ) ;
#1138 = CARTESIAN_POINT ( 'NONE',  ( -13.62178482187498396, 196.3343750006145285, 23.59362340125808188 ) ) ;
#1140 = ORIENTED_EDGE ( 'NONE', *, *, #13192, .F. ) ;
#1139 = ORIENTED_EDGE ( 'NONE', *, *, #3630, .F. ) ;
#1141 = CARTESIAN_POINT ( 'NONE',  ( 26.75643035624999655, 245.8843750006145399, 3.323476615752267715 ) ) ;
#1142 = CARTESIAN_POINT ( 'NONE',  ( 6.932735513424201024, 18.85231371789855714, -10.69584247140429412 ) ) ;
#1143 = CARTESIAN_POINT ( 'NONE',  ( 21.00000000000000000, -6.646953231504538984, -2.728124999385465266 ) ) ;
#1144 = CARTESIAN_POINT ( 'NONE',  ( 14.25334919248795451, 130.1148137178985564, -6.092822981423661410 ) ) ;
#1145 = EDGE_CURVE ( 'NONE', #13208, #28137, #27709, .T. ) ;
#1146 = CARTESIAN_POINT ( 'NONE',  ( 15.00000000000000178, -3.464101615137757051, -8.456249998770944742 ) ) ;
#1147 = FACE_BOUND ( 'NONE', #16732, .T. ) ;
#1148 = VERTEX_POINT ( 'NONE', #21138 ) ;
#1149 = CARTESIAN_POINT ( 'NONE',  ( 16.56230152254411792, -7.209453229046482114, -5.484374999385515537 ) ) ;
#1150 = EDGE_LOOP ( 'NONE', ( #1703, #18410, #14, #35728 ) ) ;
#1151 = CARTESIAN_POINT ( 'NONE',  ( -27.24356964375000345, 195.7531250006145456, 0.000000000000000000 ) ) ;
#1152 = CARTESIAN_POINT ( 'NONE',  ( -7.228626920339069173, 140.0726862821014720, 10.49813415415989581 ) ) ;
#1153 = CARTESIAN_POINT ( 'NONE',  ( 24.74781001545762393, 3.604726614523240613, 164.4745922192587670 ) ) ;
#1154 = EDGE_CURVE ( 'NONE', #28711, #31946, #29357, .T. ) ;
#1155 = CARTESIAN_POINT ( 'NONE',  ( -52.76711230271184405, 218.4690446883607535, -2.393094931466363651 ) ) ;
#1156 = CARTESIAN_POINT ( 'NONE',  ( 20.99999999999999645, 245.8093750006144944, 6.646953231504538984 ) ) ;
#1157 = SURFACE_STYLE_USAGE ( .BOTH. , #35084 ) ;
#1158 = DIRECTION ( 'NONE',  ( 0.000000000000000000, 0.000000000000000000, 1.000000000000000000 ) ) ;
#1159 = CARTESIAN_POINT ( 'NONE',  ( -50.19419563604517975, 205.4999999999999716, 0.1155267958017633378 ) ) ;
#1160 = CARTESIAN_POINT ( 'NONE',  ( -11.48171059495397373, 132.8851862821014720, -4.944772684328680334 ) ) ;
#1161 = CARTESIAN_POINT ( 'NONE',  ( 37.41131328218130392, 7.646167579472015790E-16, 165.9452414505865079 ) ) ;
#1162 = ORIENTED_EDGE ( 'NONE', *, *, #2683, .T. ) ;
#1163 = CARTESIAN_POINT ( 'NONE',  ( 31.31161381383153142, -6.928203230275514990, 167.8622852179797462 ) ) ;
#1164 = CARTESIAN_POINT ( 'NONE',  ( 3.257655550457285720, 134.8976862821014606, -15.46528703574804986 ) ) ;
#1165 = CARTESIAN_POINT ( 'NONE',  ( -53.56622103062157692, 212.1620413398628671, 8.530955311639223382 ) ) ;
#1166 = CARTESIAN_POINT ( 'NONE',  ( 5.529263428287477744, 135.4726862821014777, -7.954856959092191815 ) ) ;
#1167 = DIRECTION ( 'NONE',  ( -0.000000000000000000, 1.000000000000000000, -0.000000000000000000 ) ) ;
#1168 = CARTESIAN_POINT ( 'NONE',  ( -12.50000000000000355, 31.11018628210143788, -0.1745138560725492671 ) ) ;
#1169 = CARTESIAN_POINT ( 'NONE',  ( 22.56230152254411792, 7.347880794884125653E-16, -7.425000000000042455 ) ) ;
#1170 = VERTEX_POINT ( 'NONE', #12026 ) ;
#1171 =( LENGTH_UNIT ( ) NAMED_UNIT ( * ) SI_UNIT ( .MILLI., .METRE. ) );
#1172 = CARTESIAN_POINT ( 'NONE',  ( -2.908627838312119351, 115.9226862821014521, -15.53471296425195369 ) ) ;
#1173 = CARTESIAN_POINT ( 'NONE',  ( 5.529263428287300108, 141.3273137178985621, 7.954856959092309943 ) ) ;
#1174 = CARTESIAN_POINT ( 'NONE',  ( -13.62178482187500528, 199.7281250006145399, -23.59362340125807123 ) ) ;
#1175 = CARTESIAN_POINT ( 'NONE',  ( 15.00000000000000000, 0.000000000000000000, -1.349999999999990097 ) ) ;
#1176 = CARTESIAN_POINT ( 'NONE',  ( -27.24356964375000345, 199.4093750006145456, 0.000000000000000000 ) ) ;
#1177 = DIRECTION ( 'NONE',  ( -0.000000000000000000, -1.000000000000000000, -0.000000000000000000 ) ) ;
#1178 = CARTESIAN_POINT ( 'NONE',  ( 15.60291623300155095, 2.331604889245508350, -7.999999999999992895 ) ) ;
#1179 = DIRECTION ( 'NONE',  ( 0.000000000000000000, 0.000000000000000000, 1.000000000000000000 ) ) ;
#1180 = CARTESIAN_POINT ( 'NONE',  ( 6.840914352311949109, 76.63981371789854791, 6.594114490232462877 ) ) ;
#1181 = ORIENTED_EDGE ( 'NONE', *, *, #19610, .T. ) ;
#1182 = CARTESIAN_POINT ( 'NONE',  ( 23.99999999999999645, 244.0562500012290457, -5.196152422706631135 ) ) ;
#1183 = CARTESIAN_POINT ( 'NONE',  ( 4.622313124798831829, 73.76481371789856212, -11.61527771782809282 ) ) ;
#1184 = CARTESIAN_POINT ( 'NONE',  ( 19.68408634441910721, 5.407089921784862696, -3.046874999385523530 ) ) ;
#1185 = CARTESIAN_POINT ( 'NONE',  ( 27.24356964375000700, 199.5406250006145683, 15.72908226750537075 ) ) ;
#1186 = CARTESIAN_POINT ( 'NONE',  ( 15.24356964375000167, -3.323476615752272600, -3.815624999385473615 ) ) ;
#1187 = CARTESIAN_POINT ( 'NONE',  ( -6.932735513424201912, 41.85231371789855359, 10.69584247140429412 ) ) ;
#1188 = ORIENTED_EDGE ( 'NONE', *, *, #28113, .F. ) ;
#1189 = CARTESIAN_POINT ( 'NONE',  ( 36.99136303036318196, -3.464101615137506140, 163.9398363554800540 ) ) ;
#1190 = CARTESIAN_POINT ( 'NONE',  ( 26.75643035624999655, 244.1218750006145228, -7.049594010296217766E-16 ) ) ;
#1191 = CARTESIAN_POINT ( 'NONE',  ( -0.1745138560725500443, 28.81018628210144072, 12.50000000000000355 ) ) ;
#1192 = CARTESIAN_POINT ( 'NONE',  ( -38.31919563604516554, 216.5000000000000000, -0.1155267958017906493 ) ) ;
#1193 = AXIS2_PLACEMENT_3D ( 'NONE', #20299, #5873, #32024 ) ;
#1194 = CARTESIAN_POINT ( 'NONE',  ( -57.71502896937850124, 215.5714017266979567, -3.350049139982168800 ) ) ;
#1195 =( LENGTH_UNIT ( ) NAMED_UNIT ( * ) SI_UNIT ( .MILLI., .METRE. ) );
#1196 = CARTESIAN_POINT ( 'NONE',  ( 27.61053152270135058, 5.196152422706630247, 159.9798607905470362 ) ) ;
#1197 = CARTESIAN_POINT ( 'NONE',  ( -10.69584247140429412, 80.95231371789856212, -6.932735513424201024 ) ) ;
#1198 = CARTESIAN_POINT ( 'NONE',  ( -42.68080436395489841, 205.4999999999999716, -0.1155267958017894420 ) ) ;
#1199 = CARTESIAN_POINT ( 'NONE',  ( -51.78497103062156981, 204.4285982733020148, -3.350049139982115509 ) ) ;
#1200 = CARTESIAN_POINT ( 'NONE',  ( 23.87821517812500005, -4.985214923628404016, -5.953124999385495109 ) ) ;
#1201 = CARTESIAN_POINT ( 'NONE',  ( 22.56230152254410370, 7.347880794884117764E-16, -1.012499998771038134 ) ) ;
#1202 = CARTESIAN_POINT ( 'NONE',  ( 0.1745138560722461762, 50.18981371789855217, 15.50000000000000533 ) ) ;
#1203 = CARTESIAN_POINT ( 'NONE',  ( -45.04836230271183695, 202.5810206699313767, -4.149950860017804111 ) ) ;
#1204 = AXIS2_PLACEMENT_3D ( 'NONE', #34736, #8411, #23189 ) ;
#1205 = DIRECTION ( 'NONE',  ( 1.000000000000000000, 0.000000000000000000, 0.000000000000000000 ) ) ;
#1206 = CARTESIAN_POINT ( 'NONE',  ( 8.715434833791931624, 82.86018628210145209, 8.962234695871760692 ) ) ;
#1207 = CARTESIAN_POINT ( 'NONE',  ( -14.25334919248782306, 22.48518628210144499, -6.092822981423979378 ) ) ;
#1208 = LINE ( 'NONE', #15819, #2920 ) ;
#1209 = CARTESIAN_POINT ( 'NONE',  ( -7.234628195640316228, 197.3200961906614168, -27.00000000000000000 ) ) ;
#1210 = VERTEX_POINT ( 'NONE', #23595 ) ;
#1211 = CARTESIAN_POINT ( 'NONE',  ( -5.770363421893818234, 42.03518628210144925, -14.38691631536207005 ) ) ;
#1212 = CARTESIAN_POINT ( 'NONE',  ( -27.24356964375000345, 197.9656250006145797, -15.72908226750537786 ) ) ;
#1213 = CARTESIAN_POINT ( 'NONE',  ( 22.56230152254411792, 7.347880794884125653E-16, -2.475000000000060485 ) ) ;
#1214 = CARTESIAN_POINT ( 'NONE',  ( 26.97716818855048260, 0.000000000000000000, 49.47706554351410801 ) ) ;
#1215 = ADVANCED_FACE ( 'NONE', ( #29833 ), #3119, .T. ) ;
#1216 = FACE_OUTER_BOUND ( 'NONE', #2406, .T. ) ;
#1217 = CARTESIAN_POINT ( 'NONE',  ( -7.228626920339069173, 29.67268628210144499, 10.49813415415989581 ) ) ;
#1218 = CARTESIAN_POINT ( 'NONE',  ( 21.00000000000000000, 249.2968750006145342, -6.646953231504538984 ) ) ;
#1219 = CARTESIAN_POINT ( 'NONE',  ( -3.796722387233185003, 137.0148137178985621, -8.710071997420207879 ) ) ;
#1220 = CARTESIAN_POINT ( 'NONE',  ( 23.87821517812499650, 244.3093750006145228, -4.985214923628404904 ) ) ;
#1221 = AXIS2_PLACEMENT_3D ( 'NONE', #29172, #18014, #26333 ) ;
#1222 = ORIENTED_EDGE ( 'NONE', *, *, #25857, .T. ) ;
#1223 = CARTESIAN_POINT ( 'NONE',  ( 26.99999999999999289, 0.000000000000000000, -8.000000000000000000 ) ) ;
#1224 = CARTESIAN_POINT ( 'NONE',  ( -2.311890736173447980, 133.2773137178985507, 12.53471296425189330 ) ) ;
#1225 = CARTESIAN_POINT ( 'NONE',  ( 13.44051670066911619, -5.407089921784859143, -6.815624999385539340 ) ) ;
#1226 = CARTESIAN_POINT ( 'NONE',  ( 31.04442699002431993, 7.209453229046475009, 164.8083258472544230 ) ) ;
#1227 = CARTESIAN_POINT ( 'NONE',  ( 0.000000000000000000, 210.0000000000000284, 0.000000000000000000 ) ) ;
#1228 = CARTESIAN_POINT ( 'NONE',  ( 13.50000000000001421, 198.8000000000000114, 23.38268590217984055 ) ) ;
#1229 = VERTEX_POINT ( 'NONE', #1019 ) ;
#1230 = CARTESIAN_POINT ( 'NONE',  ( 10.69584247140445221, 44.04768628210144499, -6.932735513423970097 ) ) ;
#1231 = ORIENTED_EDGE ( 'NONE', *, *, #34414, .F. ) ;
#1232 = ORIENTED_EDGE ( 'NONE', *, *, #16331, .T. ) ;
#1233 = CARTESIAN_POINT ( 'NONE',  ( -13.50000000000000533, 195.8750000000000284, -23.38268590217984411 ) ) ;
#1234 = DIRECTION ( 'NONE',  ( 0.000000000000000000, 0.000000000000000000, 1.000000000000000000 ) ) ;
#1235 = DIRECTION ( 'NONE',  ( 1.000000000000000000, 0.000000000000000000, 0.000000000000000000 ) ) ;
#1236 = CARTESIAN_POINT ( 'NONE',  ( 25.22171936664797798, 0.000000000000000000, 169.8914008901326724 ) ) ;
#1237 = CARTESIAN_POINT ( 'NONE',  ( 21.00000000000000000, 6.646953231504538984, -9.253124999385450522 ) ) ;
#1238 = VECTOR ( 'NONE', #13008, 1000.000000000000000 ) ;
#1239 = CARTESIAN_POINT ( 'NONE',  ( 0.1745138560725515708, 70.21018628210144641, -12.50000000000000355 ) ) ;
#1240 = CARTESIAN_POINT ( 'NONE',  ( 0.1745138560722461762, 13.38981371789854613, 15.50000000000000533 ) ) ;
#1241 = DIRECTION ( 'NONE',  ( 0.000000000000000000, 1.000000000000000000, 0.000000000000000000 ) ) ;
#1242 = ADVANCED_FACE ( 'NONE', ( #35518 ), #20758, .F. ) ;
#1243 = CARTESIAN_POINT ( 'NONE',  ( 15.00000000000000178, 243.7937500012290570, 3.464101615137757051 ) ) ;
#1244 = CARTESIAN_POINT ( 'NONE',  ( -50.78794563604517975, 206.7903428501025758, 3.378800118222471838 ) ) ;
#1245 = FACE_OUTER_BOUND ( 'NONE', #30744, .T. ) ;
#1246 = CARTESIAN_POINT ( 'NONE',  ( 31.30180879287953388, 6.928203230275506996, 167.7502133156687876 ) ) ;
#1247 = CARTESIAN_POINT ( 'NONE',  ( -11.48171059495408208, 134.7148137178985507, 4.944772684328421875 ) ) ;
#1248 = CARTESIAN_POINT ( 'NONE',  ( -50.00372103062157692, 216.5309553116391612, -1.626142955000564383 ) ) ;
#1249 = CARTESIAN_POINT ( 'NONE',  ( -30.99627896937850480, 201.4690446883607251, -2.162041339862721845 ) ) ;
#1250 = ADVANCED_FACE ( 'NONE', ( #23225 ), #9190, .F. ) ;
#1251 = AXIS2_PLACEMENT_3D ( 'NONE', #32704, #15845, #15660 ) ;
#1252 = CARTESIAN_POINT ( 'NONE',  ( 15.24356964374999990, 0.000000000000000000, -0.2531249993854844949 ) ) ;
#1253 = CARTESIAN_POINT ( 'NONE',  ( -27.24356964375000345, 197.5531250006145285, 0.000000000000000000 ) ) ;
#1254 = CARTESIAN_POINT ( 'NONE',  ( -14.25334919248795096, 107.1148137178985564, 6.092822981423662299 ) ) ;
#1255 = CARTESIAN_POINT ( 'NONE',  ( -47.02752896937850124, 213.3500491399821613, 5.571401726697954970 ) ) ;
#1256 = ORIENTED_EDGE ( 'NONE', *, *, #6674, .F. ) ;
#1257 = CARTESIAN_POINT ( 'NONE',  ( 8.715434833791931624, 18.46018628210144286, 8.962234695871760692 ) ) ;
#1258 = CARTESIAN_POINT ( 'NONE',  ( -1.045839947578415010E-13, 196.1750000012290229, 27.00000000000000355 ) ) ;
#1259 = DIRECTION ( 'NONE',  ( -0.000000000000000000, -0.000000000000000000, 1.000000000000000000 ) ) ;
#1260 = CARTESIAN_POINT ( 'NONE',  ( 28.02440086159767674, -5.407089921784865361, 166.1077331045103733 ) ) ;
#1261 = CARTESIAN_POINT ( 'NONE',  ( -0.1745138560725817967, 111.6101862821014521, 15.50000000000000533 ) ) ;
#1262 = CARTESIAN_POINT ( 'NONE',  ( -49.40997103062156981, 215.5714017266979852, 3.350049139982118618 ) ) ;
#1263 = CARTESIAN_POINT ( 'NONE',  ( 22.80587116629410716, 7.646167579472015790E-16, -4.415624999385525662 ) ) ;
#1264 = CARTESIAN_POINT ( 'NONE',  ( -7.954856959092191815, 41.17268628210143078, -5.529263428287477744 ) ) ;
#1265 = CARTESIAN_POINT ( 'NONE',  ( 16.56230152254410726, 0.000000000000000000, 10.00000000000000000 ) ) ;
#1266 = CARTESIAN_POINT ( 'NONE',  ( -38.52455436395490551, 203.6929966515020283, 6.137860380172978303 ) ) ;
#1267 = CARTESIAN_POINT ( 'NONE',  ( 20.99999999999995381, 242.9124999999999943, 5.999999999999998224 ) ) ;
#1268 = CARTESIAN_POINT ( 'NONE',  ( 11.61527771782819940, 71.93518628210145494, -4.622313124798573369 ) ) ;
#1269 = CARTESIAN_POINT ( 'NONE',  ( 18.00000000000000355, -5.196152422706632912, -7.968749998770952025 ) ) ;
#1270 = CARTESIAN_POINT ( 'NONE',  ( 26.99999999999999645, 247.6187500012290741, -3.464101615137755275 ) ) ;
#1272 = CARTESIAN_POINT ( 'NONE',  ( 16.56230152254410726, 0.000000000000000000, 10.00000000000000000 ) ) ;
#1271 = CARTESIAN_POINT ( 'NONE',  ( -8.843639120294326972, 48.93518628210144072, 3.474262827703335166 ) ) ;
#1273 = FACE_OUTER_BOUND ( 'NONE', #14565, .T. ) ;
#1274 = ORIENTED_EDGE ( 'NONE', *, *, #16176, .T. ) ;
#1275 = CARTESIAN_POINT ( 'NONE',  ( 21.00000000000000000, 6.928203230275506996, -0.1124999999999909128 ) ) ;
#1276 = CARTESIAN_POINT ( 'NONE',  ( -13.49999999999998401, 195.6875000012290400, 23.38268590217985476 ) ) ;
#1277 = CARTESIAN_POINT ( 'NONE',  ( 30.88264414254899393, 7.209453229046482114, 162.9591394389215964 ) ) ;
#1278 = CARTESIAN_POINT ( 'NONE',  ( 24.77882776526477571, -3.464101615137761048, 162.0344784741307933 ) ) ;
#1279 = CARTESIAN_POINT ( 'NONE',  ( 23.99999999999999645, 245.3500000000000227, -5.196152422706631135 ) ) ;
#1280 = CARTESIAN_POINT ( 'NONE',  ( 13.62178482187499640, 195.1531250006145513, -23.59362340125807123 ) ) ;
#1281 = CARTESIAN_POINT ( 'NONE',  ( 2.311890736173452865, 110.2773137178985650, -12.53471296425189152 ) ) ;
#1282 = CARTESIAN_POINT ( 'NONE',  ( -12.53471296425194659, 104.4226862821014521, 2.311890736173176641 ) ) ;
#1283 = ORIENTED_EDGE ( 'NONE', *, *, #15614, .T. ) ;
#1284 = AXIS2_PLACEMENT_3D ( 'NONE', #6745, #7064, #30364 ) ;
#1285 = ORIENTED_EDGE ( 'NONE', *, *, #5231, .T. ) ;
#1286 = CARTESIAN_POINT ( 'NONE',  ( 27.00000000000000355, 198.0875000012290457, -3.306546357697854128E-15 ) ) ;
#1287 = CARTESIAN_POINT ( 'NONE',  ( 22.56230152254410726, 7.347880794884117764E-16, -9.112499998771033560 ) ) ;
#1288 = EDGE_CURVE ( 'NONE', #21775, #13344, #22888, .T. ) ;
#1289 = CARTESIAN_POINT ( 'NONE',  ( 13.23911966647199812, 67.15231371789852233, 8.632099005475788900 ) ) ;
#1290 = CARTESIAN_POINT ( 'NONE',  ( 15.24356964374999990, 0.000000000000000000, -5.653124999385472194 ) ) ;
#1291 = CARTESIAN_POINT ( 'NONE',  ( 23.87821517812500005, 244.1593750006145171, 4.985214923628404016 ) ) ;
#1292 = CARTESIAN_POINT ( 'NONE',  ( -0.1745138560725182642, 93.21018628210146062, 9.500000000000005329 ) ) ;
#1293 = ADVANCED_FACE ( 'NONE', ( #273 ), #642, .T. ) ;
#1294 = FACE_OUTER_BOUND ( 'NONE', #9316, .T. ) ;
#1295 = CARTESIAN_POINT ( 'NONE',  ( -5.233372021372612259, 51.05231371789854222, 8.152565276336593669 ) ) ;
#1296 = CARTESIAN_POINT ( 'NONE',  ( 19.68408634441910721, 5.407089921784857367, -8.390624999385531524 ) ) ;
#1297 =( BOUNDED_CURVE ( )  B_SPLINE_CURVE ( 2, ( #36397, #25222, #16702, #28423, #36212, #7793, #8169 ),
 .UNSPECIFIED., .F., .F. ) 
 B_SPLINE_CURVE_WITH_KNOTS ( ( 3, 2, 2, 3 ),
 ( 0.2173913043478289675, 0.2246376811594223422, 0.2318840579710157446, 0.2391304347826091192 ),
 .UNSPECIFIED. ) 
 CURVE ( )  GEOMETRIC_REPRESENTATION_ITEM ( )  RATIONAL_B_SPLINE_CURVE ( ( 0.9999999999999465983, 0.8660254037844921093, 1.000000000000000000, 0.8660254037844387076, 1.000000000000000000, 0.8660254037844310471, 1.000000000000007772 ) ) 
 REPRESENTATION_ITEM ( '' )  );
#1298 = CARTESIAN_POINT ( 'NONE',  ( -6.840914352311947333, 108.8398137178985507, -6.594114490232462877 ) ) ;
#1299 = CARTESIAN_POINT ( 'NONE',  ( 26.75643035624999655, 240.0718750006145399, -7.049594010296217766E-16 ) ) ;
#1300 = CARTESIAN_POINT ( 'NONE',  ( -0.1745138560722763466, 36.38981371789855501, -12.50000000000000355 ) ) ;
#1301 = CIRCLE ( 'NONE', #23716, 5.999999999999998224 ) ;
#1302 = CARTESIAN_POINT ( 'NONE',  ( -8.715434833791929847, 87.46018628210144641, -8.962234695871762469 ) ) ;
#1303 = CARTESIAN_POINT ( 'NONE',  ( 22.56230152254410015, 7.347880794884117764E-16, -7.762499998770988618 ) ) ;
#1304 = EDGE_CURVE ( 'NONE', #17372, #23833, #795, .T. ) ;
#1305 = CYLINDRICAL_SURFACE ( 'NONE', #17735, 27.00000000000000000 ) ;
#1306 = CARTESIAN_POINT ( 'NONE',  ( 37.13677269252619340, 7.646167579472015790E-16, 162.8072281515975135 ) ) ;
#1307 = VECTOR ( 'NONE', #7532, 1000.000000000000000 ) ;
#1308 = CARTESIAN_POINT ( 'NONE',  ( 22.80587116629411781, -3.604726614523238837, -4.509374999385530103 ) ) ;
#1309 = CARTESIAN_POINT ( 'NONE',  ( 14.99999999999945111, -3.464101615137439083, -0.8625000000000012657 ) ) ;
#1310 = CARTESIAN_POINT ( 'NONE',  ( -12.50000000000000355, 6.489813717898557321, 0.1745138560722786503 ) ) ;
#1311 = CARTESIAN_POINT ( 'NONE',  ( 18.00000000000000355, -5.196152422706632912, -5.718749998770950249 ) ) ;
#1312 = CARTESIAN_POINT ( 'NONE',  ( -3.796722387233375073, 102.9851862821014805, 8.710071997420127943 ) ) ;
#1313 = CARTESIAN_POINT ( 'NONE',  ( 18.00000000000000355, -5.196152422706632912, -4.368749998770960374 ) ) ;
#1314 =( BOUNDED_CURVE ( )  B_SPLINE_CURVE ( 3, ( #224, #25821, #19966, #5910 ),
 .UNSPECIFIED., .F., .F. ) 
 B_SPLINE_CURVE_WITH_KNOTS ( ( 4, 4 ),
 ( 4.712388980384690562, 6.283185307179586232 ),
 .UNSPECIFIED. ) 
 CURVE ( )  GEOMETRIC_REPRESENTATION_ITEM ( )  RATIONAL_B_SPLINE_CURVE ( ( 1.000000000000000000, 0.8047378541243652705, 0.8047378541243652705, 1.000000000000000000 ) ) 
 REPRESENTATION_ITEM ( '' )  );
#1315 = CARTESIAN_POINT ( 'NONE',  ( 12.53471296425194836, 136.6226862821014834, -2.311890736173178418 ) ) ;
#1316 = CARTESIAN_POINT ( 'NONE',  ( -6.422845572874366304, 142.9999999999996305, 10.72508787064079172 ) ) ;
#1317 = CARTESIAN_POINT ( 'NONE',  ( 15.24356964374999990, 249.8218750006145399, -3.323476615752268604 ) ) ;
#1318 = VERTEX_POINT ( 'NONE', #35323 ) ;
#1319 = CARTESIAN_POINT ( 'NONE',  ( 28.21233043189729273, 5.407089921784856479, 168.2557779222707097 ) ) ;
#1320 = CARTESIAN_POINT ( 'NONE',  ( 18.12178482187500350, -4.985214923628407568, -3.665624999385469707 ) ) ;
#1321 = EDGE_CURVE ( 'NONE', #18637, #7872, #9377, .T. ) ;
#1322 = CARTESIAN_POINT ( 'NONE',  ( 27.24356964375000700, 199.5968750006145740, 15.72908226750537075 ) ) ;
#1323 = CARTESIAN_POINT ( 'NONE',  ( 2.999999999999997780, 244.5000000000000000, 2.500000000000000000 ) ) ;
#1324 = CARTESIAN_POINT ( 'NONE',  ( 34.27731952563551232, 5.196152422706637353, 167.3393168814877185 ) ) ;
#1325 = CARTESIAN_POINT ( 'NONE',  ( 27.00000000000000355, 199.4375000012290400, -3.306546357697854128E-15 ) ) ;
#1326 = CARTESIAN_POINT ( 'NONE',  ( 26.75643035624999655, 241.9843750006145342, -7.049594010296217766E-16 ) ) ;
#1327 = CARTESIAN_POINT ( 'NONE',  ( 16.56230152254410726, -7.209453229046475009, -3.178124999385525395 ) ) ;
#1328 = CARTESIAN_POINT ( 'NONE',  ( 8.152565276336593669, 21.15231371789855430, 5.233372021372610483 ) ) ;
#1329 = CARTESIAN_POINT ( 'NONE',  ( 27.24356964375000700, 195.9968750006145513, 15.72908226750537075 ) ) ;
#1331 = ORIENTED_EDGE ( 'NONE', *, *, #25346, .T. ) ;
#1330 = ORIENTED_EDGE ( 'NONE', *, *, #23016, .T. ) ;
#1332 = VECTOR ( 'NONE', #31249, 1000.000000000000000 ) ;
#1333 = CARTESIAN_POINT ( 'NONE',  ( 21.00000000000000000, 247.8343750006144717, -6.646953231504538984 ) ) ;
#1334 = CARTESIAN_POINT ( 'NONE',  ( -11.61527771782809282, 25.46481371789855075, -4.622313124798832717 ) ) ;
#1335 = CARTESIAN_POINT ( 'NONE',  ( 18.12178482187499640, 4.985214923628404904, -0.6656249993854668201 ) ) ;
#1336 = CARTESIAN_POINT ( 'NONE',  ( -14.38691631536193860, 126.6648137178985820, -5.770363421894132649 ) ) ;
#1337 = CARTESIAN_POINT ( 'NONE',  ( 26.75643035624999655, 7.049594010296217766E-16, -0.4781249993854874702 ) ) ;
#1338 = VERTEX_POINT ( 'NONE', #20951 ) ;
#1339 = CARTESIAN_POINT ( 'NONE',  ( 16.56230152254411081, 7.209453229046482114, -5.709374999385496530 ) ) ;
#1340 = VERTEX_POINT ( 'NONE', #32484 ) ;
#1341 = CARTESIAN_POINT ( 'NONE',  ( -27.24356964375000345, 196.6531250006145513, 0.000000000000000000 ) ) ;
#1342 = CARTESIAN_POINT ( 'NONE',  ( -4.622313124798576922, 134.0351862821014493, -11.61527771782819762 ) ) ;
#1343 = CARTESIAN_POINT ( 'NONE',  ( 24.86547026816695904, 3.604726614523240613, 165.8194550616826461 ) ) ;
#1344 = CARTESIAN_POINT ( 'NONE',  ( -51.77752896937850124, 214.3500491399821897, 7.303452534266821949 ) ) ;
#1345 = CARTESIAN_POINT ( 'NONE',  ( 26.75643035624999655, 246.7843750006145171, 3.323476615752267271 ) ) ;
#1346 =( NAMED_UNIT ( * ) SI_UNIT ( $, .STERADIAN. ) SOLID_ANGLE_UNIT ( ) );
#1347 = CARTESIAN_POINT ( 'NONE',  ( -26.99999999999999645, 199.2500000012290116, 15.58845726811991561 ) ) ;
#1348 = CARTESIAN_POINT ( 'NONE',  ( -39.70461230271183695, 208.6787018382582346, -4.469044688360757966 ) ) ;
#1349 = CARTESIAN_POINT ( 'NONE',  ( 11.48171059495397728, 137.4851862821014663, 4.944772684328674117 ) ) ;
#1350 = CARTESIAN_POINT ( 'NONE',  ( 25.02725311564228505, 3.604726614523236616, 167.6686414700154444 ) ) ;
#1351 = VERTEX_POINT ( 'NONE', #6531 ) ;
#1352 = FACE_OUTER_BOUND ( 'NONE', #34745, .T. ) ;
#1353 = CARTESIAN_POINT ( 'NONE',  ( 8.632099005475504683, 129.1476862821014322, 13.23911966647218996 ) ) ;
#1354 = CARTESIAN_POINT ( 'NONE',  ( -48.81622103062156981, 212.1620413398628671, 8.530955311639223382 ) ) ;
#1355 =( BOUNDED_CURVE ( )  B_SPLINE_CURVE ( 2, ( #10748, #29951, #25522, #19488, #18598, #33873, #4171 ),
 .UNSPECIFIED., .F., .F. ) 
 B_SPLINE_CURVE_WITH_KNOTS ( ( 3, 2, 2, 3 ),
 ( 0.4782608695652167397, 0.4855072463768107527, 0.4927536231884048767, 0.4999999999999988898 ),
 .UNSPECIFIED. ) 
 CURVE ( )  GEOMETRIC_REPRESENTATION_ITEM ( )  RATIONAL_B_SPLINE_CURVE ( ( 1.000000000000012212, 0.8660254037844263841, 1.000000000000000000, 0.8660254037844387076, 1.000000000000000000, 0.8660254037844592467, 0.9999999999999794609 ) ) 
 REPRESENTATION_ITEM ( '' )  );
#1356 = CARTESIAN_POINT ( 'NONE',  ( 9.465287035748067623, 118.7976862821014521, 2.064181346179272847 ) ) ;
#1357 = EDGE_CURVE ( 'NONE', #13931, #17802, #834, .T. ) ;
#1358 = CARTESIAN_POINT ( 'NONE',  ( 20.99999999999997513, 246.3437500012290684, -5.999999999999999112 ) ) ;
#1359 = ADVANCED_FACE ( 'NONE', ( #15816 ), #4428, .T. ) ;
#1360 = CARTESIAN_POINT ( 'NONE',  ( -10.49813415415989581, 13.57268628210145600, -7.228626920339068285 ) ) ;
#1361 = CARTESIAN_POINT ( 'NONE',  ( 16.56230152254411436, -6.928203230275514990, -7.987500000000027356 ) ) ;
#1362 = UNCERTAINTY_MEASURE_WITH_UNIT (LENGTH_MEASURE( 1.000000000000000082E-05 ), #30394, 'distance_accuracy_value', 'NONE');
#1363 = ORIENTED_EDGE ( 'NONE', *, *, #4409, .T. ) ;
#1364 = CARTESIAN_POINT ( 'NONE',  ( 13.23911966647218996, 117.6476862821014322, -8.632099005475504683 ) ) ;
#1365 = CARTESIAN_POINT ( 'NONE',  ( -89.83814373643217266, 60.44923248139874516, 5.000000000000000000 ) ) ;
#1366 = CARTESIAN_POINT ( 'NONE',  ( 9.500000000000005329, 8.110186282101443211, 0.1745138560725188748 ) ) ;
#1367 = CARTESIAN_POINT ( 'NONE',  ( -27.24356964374999990, 198.8656250006145569, -15.72908226750537786 ) ) ;
#1368 = CARTESIAN_POINT ( 'NONE',  ( 15.00000000000000000, 0.000000000000000000, -2.250000000000001776 ) ) ;
#1369 = CARTESIAN_POINT ( 'NONE',  ( -26.99999999999998934, 196.4375000000000284, 15.58845726811991561 ) ) ;
#1370 = DIRECTION ( 'NONE',  ( 0.9961946980917462113, 0.000000000000000000, -0.08715574274765118534 ) ) ;
#1371 = EDGE_CURVE ( 'NONE', #27477, #5428, #18984, .T. ) ;
#1372 = DIRECTION ( 'NONE',  ( 1.000000000000000000, 0.000000000000000000, 0.000000000000000000 ) ) ;
#1373 = CARTESIAN_POINT ( 'NONE',  ( -5.529263428287297444, 81.52731371789856496, -7.954856959092311719 ) ) ;
#1374 = EDGE_LOOP ( 'NONE', ( #17403, #25108, #14081, #5850 ) ) ;
#1375 = PRODUCT_RELATED_PRODUCT_CATEGORY ( 'part', '', ( #11977 ) ) ;
#1376 = CARTESIAN_POINT ( 'NONE',  ( 26.99999999999999645, 243.9437500012290343, 3.464101615137751278 ) ) ;
#1377 = CARTESIAN_POINT ( 'NONE',  ( 4.944772684328420986, 77.21481371789855075, 11.48171059495408208 ) ) ;
#1378 = CARTESIAN_POINT ( 'NONE',  ( 19.68408634441911431, 5.407089921784862696, -4.846874999385547333 ) ) ;
#1379 = CARTESIAN_POINT ( 'NONE',  ( 26.75643035624999655, 3.323476615752271712, -5.390624999385475569 ) ) ;
#1380 = CARTESIAN_POINT ( 'NONE',  ( -12.50000000000000355, 52.48981371789855643, 0.1745138560722786503 ) ) ;
#1381 = ORIENTED_EDGE ( 'NONE', *, *, #20383, .F. ) ;
#1382 = CARTESIAN_POINT ( 'NONE',  ( 20.99999999999999645, 6.646953231504538984, -7.003124999385472726 ) ) ;
#1383 = CARTESIAN_POINT ( 'NONE',  ( 23.87821517812499650, 245.0968750006145171, -4.985214923628404904 ) ) ;
#1384 = CARTESIAN_POINT ( 'NONE',  ( -11.61527771782819940, 21.33518628210144641, 4.622313124798574258 ) ) ;
#1385 = VECTOR ( 'NONE', #16289, 1000.000000000000000 ) ;
#1386 = CARTESIAN_POINT ( 'NONE',  ( -37.92336230271182984, 215.6869285224997270, 3.149950860017831200 ) ) ;
#1387 = CARTESIAN_POINT ( 'NONE',  ( -49.99627896937850124, 203.4690446883607535, -1.626142955000504209 ) ) ;
#1388 = DIRECTION ( 'NONE',  ( -0.000000000000000000, 1.000000000000000000, -0.000000000000000000 ) ) ;
#1389 = CARTESIAN_POINT ( 'NONE',  ( 0.1745138560722779009, 77.78981371789855359, 12.50000000000000355 ) ) ;
#1390 = CARTESIAN_POINT ( 'NONE',  ( -41.09747103062157692, 212.3500491399821613, -3.839350919129076445 ) ) ;
#1391 = CARTESIAN_POINT ( 'NONE',  ( -62.27455436395490551, 205.1570982666397356, 4.673758765035198159 ) ) ;
#1392 = CARTESIAN_POINT ( 'NONE',  ( 16.56230152254410726, 0.000000000000000000, 0.000000000000000000 ) ) ;
#1393 = CARTESIAN_POINT ( 'NONE',  ( -3.253724281355068545E-15, 196.2874999999999659, -27.00000000000000355 ) ) ;
#1394 = CARTESIAN_POINT ( 'NONE',  ( 0.1745138560722461762, 59.38981371789856212, 15.50000000000000533 ) ) ;
#1395 = CARTESIAN_POINT ( 'NONE',  ( -48.80877896937850124, 212.1620413398627534, -8.530955311639255356 ) ) ;
#1396 = CARTESIAN_POINT ( 'NONE',  ( -27.00000000000000355, 198.1625000000000227, -15.58845726811989429 ) ) ;
#1397 = CARTESIAN_POINT ( 'NONE',  ( -12.46528703574805697, 77.39768628210144641, -2.660918448318280838 ) ) ;
#1398 = CARTESIAN_POINT ( 'NONE',  ( 13.23911966647218996, 34.84768628210143504, -8.632099005475504683 ) ) ;
#1399 = CARTESIAN_POINT ( 'NONE',  ( 13.56230152254410903, 5.196152422706636465, -0.5250000000000532019 ) ) ;
#1400 = CARTESIAN_POINT ( 'NONE',  ( -4.500000000000000888, 210.0000000000000284, 2.500000000000000000 ) ) ;
#1401 = EDGE_LOOP ( 'NONE', ( #763, #24922, #8044, #21636 ) ) ;
#1402 = CARTESIAN_POINT ( 'NONE',  ( -13.23911966647218463, 39.44768628210144357, 8.632099005475506459 ) ) ;
#1403 = CARTESIAN_POINT ( 'NONE',  ( -1.926257025242585782E-15, 198.3406250006145228, -31.45816453501076637 ) ) ;
#1404 = CARTESIAN_POINT ( 'NONE',  ( 16.56230152254411081, 6.928203230275506996, -8.549999998770985599 ) ) ;
#1405 = CARTESIAN_POINT ( 'NONE',  ( 1.069080835302379631E-14, 199.2125000000000057, 27.00000000000000000 ) ) ;
#1406 = CARTESIAN_POINT ( 'NONE',  ( -34.56622103062155560, 211.6261429550005744, 6.530955311639227823 ) ) ;
#1407 = CARTESIAN_POINT ( 'NONE',  ( 34.31653960987195973, 5.196152422706637353, 167.7876044956290116 ) ) ;
#1408 = CARTESIAN_POINT ( 'NONE',  ( 12.53471296425194836, 26.22268628210144925, -2.311890736173178418 ) ) ;
#1409 = CARTESIAN_POINT ( 'NONE',  ( 15.24356964374999990, 248.9593750006145285, 0.000000000000000000 ) ) ;
#1410 = CARTESIAN_POINT ( 'NONE',  ( 7.954856959092311719, 129.8273137178985905, -5.529263428287300108 ) ) ;
#1411 = CARTESIAN_POINT ( 'NONE',  ( 23.87821517812499650, 245.2093750006145569, -4.985214923628404904 ) ) ;
#1412 = ORIENTED_EDGE ( 'NONE', *, *, #35882, .T. ) ;
#1413 = CARTESIAN_POINT ( 'NONE',  ( -29.00000000000002487, 210.0000000000000000, 0.000000000000000000 ) ) ;
#1414 = CARTESIAN_POINT ( 'NONE',  ( 4.944772684328420986, 141.6148137178985849, 11.48171059495408208 ) ) ;
#1415 = CARTESIAN_POINT ( 'NONE',  ( 10.31873187879411091, 0.000000000000000000, -7.340624999385508609 ) ) ;
#1416 = CARTESIAN_POINT ( 'NONE',  ( 37.29365302947196881, 7.646167579472015790E-16, 164.6003786081626572 ) ) ;
#1417 = CARTESIAN_POINT ( 'NONE',  ( 31.40966402442264283, 6.928203230275514990, 168.9830042533329504 ) ) ;
#1418 = CARTESIAN_POINT ( 'NONE',  ( -26.99999999999998934, 196.4375000000000284, 15.58845726811991561 ) ) ;
#1419 = ORIENTED_EDGE ( 'NONE', *, *, #11897, .T. ) ;
#1420 = CARTESIAN_POINT ( 'NONE',  ( -8.962234695871760692, 29.96018628210143930, 8.715434833791933400 ) ) ;
#1421 = ORIENTED_EDGE ( 'NONE', *, *, #25932, .T. ) ;
#1422 = ORIENTED_EDGE ( 'NONE', *, *, #30812, .T. ) ;
#1423 = CARTESIAN_POINT ( 'NONE',  ( 24.58599568454329543, 3.464101615138089674, 159.8303977058270959 ) ) ;
#1424 = CARTESIAN_POINT ( 'NONE',  ( 26.99999999999999289, 0.000000000000000000, -8.000000000000000000 ) ) ;
#1425 = FACE_OUTER_BOUND ( 'NONE', #9140, .T. ) ;
#1427 = CYLINDRICAL_SURFACE ( 'NONE', #12358, 5.999999999999994671 ) ;
#1426 =( GEOMETRIC_REPRESENTATION_CONTEXT ( 3 ) GLOBAL_UNCERTAINTY_ASSIGNED_CONTEXT ( ( #4017 ) ) GLOBAL_UNIT_ASSIGNED_CONTEXT ( ( #8757, #31502, #25813 ) ) REPRESENTATION_CONTEXT ( 'NONE', 'WORKASPACE' ) );
#1428 = CARTESIAN_POINT ( 'NONE',  ( 23.87821517812500005, -4.985214923628404016, -8.540624999385460825 ) ) ;
#1429 = CARTESIAN_POINT ( 'NONE',  ( -12.53471296425194836, 86.02268628210146062, 2.311890736173176641 ) ) ;
#1430 = CARTESIAN_POINT ( 'NONE',  ( -13.04141134922759804, 133.1726862821014663, -8.927990412390657937 ) ) ;
#1431 = AXIS2_PLACEMENT_3D ( 'NONE', #12225, #7297, #26816 ) ;
#1432 = CARTESIAN_POINT ( 'NONE',  ( -4.694659320240884604E-14, 197.4124999999999943, 27.00000000000000000 ) ) ;
#1433 = CARTESIAN_POINT ( 'NONE',  ( 19.39230484541326049, 243.6638461906613600, -5.999999999999997335 ) ) ;
#1434 = CARTESIAN_POINT ( 'NONE',  ( -59.29836230271182984, 206.0451222850691977, -2.149950860017851184 ) ) ;
#1435 = DIRECTION ( 'NONE',  ( -1.000000000000000000, -6.123233995736766036E-17, 0.000000000000000000 ) ) ;
#1436 = CARTESIAN_POINT ( 'NONE',  ( 25.21351703232580022, 3.464101615137752166, 167.0029995320877276 ) ) ;
#1437 = CARTESIAN_POINT ( 'NONE',  ( -8.962234695871565293, 136.4398137178985735, -8.715434833792128799 ) ) ;
#1438 = CARTESIAN_POINT ( 'NONE',  ( -41.69122103062155560, 208.3738570449993404, -6.530955311639226935 ) ) ;
#1439 = CARTESIAN_POINT ( 'NONE',  ( -52.97247103062156270, 205.6499508600178956, 7.303452534266880569 ) ) ;
#1440 = CONTEXT_DEPENDENT_SHAPE_REPRESENTATION ( #22392, #8026 ) ;
#1441 = CARTESIAN_POINT ( 'NONE',  ( 18.00000000000000355, 241.0750000000000171, 5.196152422706632912 ) ) ;
#1442 = CARTESIAN_POINT ( 'NONE',  ( -1.926257025242585782E-15, 198.7906250006145399, -31.45816453501075927 ) ) ;
#1443 = CARTESIAN_POINT ( 'NONE',  ( 6.092822981423662299, 104.8148137178985593, 14.25334919248795096 ) ) ;
#1444 = CARTESIAN_POINT ( 'NONE',  ( -49.99627896937850124, 203.4690446883607535, -1.626142955000504209 ) ) ;
#1445 = ORIENTED_EDGE ( 'NONE', *, *, #16238, .T. ) ;
#1446 = CARTESIAN_POINT ( 'NONE',  ( -6.000000000000000888, -30.00000000000000000, 20.00000000000000711 ) ) ;
#1447 = FACE_OUTER_BOUND ( 'NONE', #12667, .T. ) ;
#1448 = CARTESIAN_POINT ( 'NONE',  ( -13.49999999999998401, 197.8249999999999886, 23.38268590217985476 ) ) ;
#1449 = CARTESIAN_POINT ( 'NONE',  ( 27.82830044041545747, -5.407089921784865361, 163.8662950338039650 ) ) ;
#1450 = AXIS2_PLACEMENT_3D ( 'NONE', #34313, #8358, #5492 ) ;
#1451 = CARTESIAN_POINT ( 'NONE',  ( -5.770363421893818234, 97.23518628210146630, -14.38691631536207005 ) ) ;
#1452 =( GEOMETRIC_REPRESENTATION_CONTEXT ( 3 ) GLOBAL_UNCERTAINTY_ASSIGNED_CONTEXT ( ( #35394 ) ) GLOBAL_UNIT_ASSIGNED_CONTEXT ( ( #31975, #20431, #14733 ) ) REPRESENTATION_CONTEXT ( 'NONE', 'WORKASPACE' ) );
#1453 = CARTESIAN_POINT ( 'NONE',  ( -56.73288769728823411, 203.5309553116391896, -1.857196546604028997 ) ) ;
#1454 = CIRCLE ( 'NONE', #28104, 2.649999999999991029 ) ;
#1455 = CARTESIAN_POINT ( 'NONE',  ( 16.56230152254411081, 7.209453229046475009, -3.403124999385538807 ) ) ;
#1456 = CARTESIAN_POINT ( 'NONE',  ( 2.064181346179272847, 42.89768628210143220, -9.465287035748065847 ) ) ;
#1457 = LINE ( 'NONE', #35951, #26756 ) ;
#1458 = CARTESIAN_POINT ( 'NONE',  ( -35.95163769728824121, 217.4189793300686233, -4.149950860017907139 ) ) ;
#1459=STYLED_ITEM('',(#37556),#33379);
#1460 = CARTESIAN_POINT ( 'NONE',  ( 15.26155779561005232, -6.106572496351636126, -10.00000000000000000 ) ) ;
#1461 = CARTESIAN_POINT ( 'NONE',  ( 2.660918448318279950, 70.49768628210145494, -12.46528703574805697 ) ) ;
#1462 = DIRECTION ( 'NONE',  ( 0.08715574274765150453, 0.000000000000000000, 0.9961946980917461003 ) ) ;
#1464 = VERTEX_POINT ( 'NONE', #21326 ) ;
#1463 = CARTESIAN_POINT ( 'NONE',  ( -7.954856959092191815, 41.17268628210143078, -5.529263428287477744 ) ) ;
#1465 = CARTESIAN_POINT ( 'NONE',  ( 2.999999999999997335, 244.5000000000000000, -2.499999999999999556 ) ) ;
#1466 = ORIENTED_EDGE ( 'NONE', *, *, #32719, .T. ) ;
#1467 = CARTESIAN_POINT ( 'NONE',  ( 21.00000000000000000, -6.928203230275506996, -2.137499999999987743 ) ) ;
#1468 = LINE ( 'NONE', #22824, #18170 ) ;
#1469 = CARTESIAN_POINT ( 'NONE',  ( 33.98928129033111389, 5.407089921784862696, 162.6497006628943041 ) ) ;
#1470 = CARTESIAN_POINT ( 'NONE',  ( 36.82794601260381029, 7.347880794884125653E-16, 162.0719712953337250 ) ) ;
#1471 = CARTESIAN_POINT ( 'NONE',  ( 18.00000000000000355, 245.1250000000000000, 5.196152422706632912 ) ) ;
#1472 = CARTESIAN_POINT ( 'NONE',  ( 2.999999999999997335, 237.0000000000000000, 5.000000000000000000 ) ) ;
#1473 = CARTESIAN_POINT ( 'NONE',  ( 0.1745138560722779009, 77.78981371789855359, 12.50000000000000355 ) ) ;
#1474 = CARTESIAN_POINT ( 'NONE',  ( 12.53471296425194659, 99.82268628210144357, -2.311890736173178418 ) ) ;
#1475 = VERTEX_POINT ( 'NONE', #13339 ) ;
#1476 = ORIENTED_EDGE ( 'NONE', *, *, #2642, .F. ) ;
#1477 = CARTESIAN_POINT ( 'NONE',  ( -13.49999999999998401, 199.2875000012290627, 23.38268590217985476 ) ) ;
#1478 = DIRECTION ( 'NONE',  ( 0.9961946980917462113, 0.000000000000000000, -0.08715574274765118534 ) ) ;
#1479 = CARTESIAN_POINT ( 'NONE',  ( -15.53471296425188442, 61.97731371789853938, -2.908627838312459080 ) ) ;
#1480 = CARTESIAN_POINT ( 'NONE',  ( 23.87821517812499650, 4.985214923628404904, -7.153124999385473970 ) ) ;
#1481 = CARTESIAN_POINT ( 'NONE',  ( 26.75643035624999655, 244.6468750006145285, 3.323476615752267715 ) ) ;
#1482 = CARTESIAN_POINT ( 'NONE',  ( -62.07663769728824121, 206.0451222850691408, 2.149950860017832532 ) ) ;
#1483 = VECTOR ( 'NONE', #7906, 1000.000000000000000 ) ;
#1484 = CARTESIAN_POINT ( 'NONE',  ( -1.909035429704832693E-15, 195.0500000012290229, -31.17691453623979214 ) ) ;
#1485 = CARTESIAN_POINT ( 'NONE',  ( -7.954856959092309943, 60.82731371789854080, 5.529263428287300108 ) ) ;
#1486 = CARTESIAN_POINT ( 'NONE',  ( 10.31873187879411091, 3.604726614523236616, -7.828124999385534188 ) ) ;
#1487 = EDGE_CURVE ( 'NONE', #21289, #23722, #29129, .T. ) ;
#1488 = CARTESIAN_POINT ( 'NONE',  ( -7.954856959092309943, 106.8273137178985479, 5.529263428287300108 ) ) ;
#1489 = CARTESIAN_POINT ( 'NONE',  ( 8.715434833792128799, 37.53981371789855359, -8.962234695871567070 ) ) ;
#1490 = CARTESIAN_POINT ( 'NONE',  ( 10.69584247140445221, 90.04768628210145209, -6.932735513423970097 ) ) ;
#1491 = CARTESIAN_POINT ( 'NONE',  ( 22.56230152254410370, 7.347880794884117764E-16, -8.662499998771028942 ) ) ;
#1492 = CARTESIAN_POINT ( 'NONE',  ( 13.50000000000001421, 196.1000000000000227, 23.38268590217984055 ) ) ;
#1493 = CARTESIAN_POINT ( 'NONE',  ( 30.82871652672388052, -7.209453229046475009, 162.3427439694773398 ) ) ;
#1494 = CARTESIAN_POINT ( 'NONE',  ( 22.80587116629412847, -3.604726614523238837, -5.409374999385520688 ) ) ;
#1495 = DIRECTION ( 'NONE',  ( 1.000000000000000000, 0.000000000000000000, 2.057406622567553763E-16 ) ) ;
#1496 = DIRECTION ( 'NONE',  ( -0.000000000000000000, 1.000000000000000000, -0.000000000000000000 ) ) ;
#1497 = DIRECTION ( 'NONE',  ( -0.000000000000000000, -1.000000000000000000, -0.000000000000000000 ) ) ;
#1498 = CARTESIAN_POINT ( 'NONE',  ( 6.840914352312096547, 98.96018628210144641, -6.594114490232313663 ) ) ;
#1499 = LINE ( 'NONE', #745, #33419 ) ;
#1500 = CARTESIAN_POINT ( 'NONE',  ( -2.660918448318275509, 139.4976862821014549, 12.46528703574805874 ) ) ;
#1501 = CARTESIAN_POINT ( 'NONE',  ( -60.72871937935236986, 215.3268752544371978, 5.000000000000000000 ) ) ;
#1502 = CARTESIAN_POINT ( 'NONE',  ( 15.24356964374999990, 240.7093750006145285, -3.323476615752268604 ) ) ;
#1503 = ORIENTED_EDGE ( 'NONE', *, *, #11731, .F. ) ;
#1504 = CARTESIAN_POINT ( 'NONE',  ( 24.87690945940258302, -3.604726614523240613, 165.9502056158071355 ) ) ;
#1505 = CARTESIAN_POINT ( 'NONE',  ( 18.12178482187500350, -4.985214923628407568, -4.565624999385481608 ) ) ;
#1506 = EDGE_CURVE ( 'NONE', #23173, #20504, #20187, .T. ) ;
#1507 = CARTESIAN_POINT ( 'NONE',  ( -13.62178482187500528, 198.8843750006145399, -23.59362340125807123 ) ) ;
#1508 = AXIS2_PLACEMENT_3D ( 'NONE', #13039, #30663, #33125 ) ;
#1509 = DIRECTION ( 'NONE',  ( 0.000000000000000000, 0.000000000000000000, 1.000000000000000000 ) ) ;
#1510 = CARTESIAN_POINT ( 'NONE',  ( 10.49999999999999467, 237.0000000000000000, -2.500000000000000000 ) ) ;
#1511 = CARTESIAN_POINT ( 'NONE',  ( 15.24356964374999990, 244.0093750006145399, 0.000000000000000000 ) ) ;
#1512 = CARTESIAN_POINT ( 'NONE',  ( 5.233372021372610483, 9.652313717898541867, -8.152565276336593669 ) ) ;
#1513 = CARTESIAN_POINT ( 'NONE',  ( 27.24356964374999279, 196.5218750006145569, -15.72908226750539207 ) ) ;
#1515 = ORIENTED_EDGE ( 'NONE', *, *, #28122, .T. ) ;
#1514 = ORIENTED_EDGE ( 'NONE', *, *, #4696, .F. ) ;
#1516 = CARTESIAN_POINT ( 'NONE',  ( 21.00000000000000000, 247.1593750006145171, 6.646953231504538984 ) ) ;
#1517 = CARTESIAN_POINT ( 'NONE',  ( -2.660918448318005058, 26.90231371789854364, -12.46528703574811558 ) ) ;
#1518 = CARTESIAN_POINT ( 'NONE',  ( 21.00000000000000000, -6.646953231504538984, -3.628124999385489158 ) ) ;
#1519 = CARTESIAN_POINT ( 'NONE',  ( 11.08355503943118769, 122.6398137178985479, 10.83675517735179028 ) ) ;
#1520 =( BOUNDED_CURVE ( )  B_SPLINE_CURVE ( 2, ( #4940, #16154, #15967, #30924, #13483, #25039, #33392, #36780, #7432 ),
 .UNSPECIFIED., .F., .F. ) 
 B_SPLINE_CURVE_WITH_KNOTS ( ( 3, 2, 2, 2, 3 ),
 ( 0.1041666666666666713, 0.1111111111111111049, 0.1250000000000000000, 0.1388888888888888951, 0.1458333333333333426 ),
 .UNSPECIFIED. ) 
 CURVE ( )  GEOMETRIC_REPRESENTATION_ITEM ( )  RATIONAL_B_SPLINE_CURVE ( ( 0.9330127018922194093, 0.9330127018922194093, 1.000000000000000000, 0.8660254037844387076, 1.000000000000000000, 0.8660254037844387076, 1.000000000000000000, 0.9330127018922194093, 0.9330127018922194093 ) ) 
 REPRESENTATION_ITEM ( '' )  );
#1521 = CARTESIAN_POINT ( 'NONE',  ( 26.99999999999999645, 7.347880794884117764E-16, -9.168749998770959309 ) ) ;
#1522 = ORIENTED_EDGE ( 'NONE', *, *, #16803, .T. ) ;
#1523 = CARTESIAN_POINT ( 'NONE',  ( 13.44051670066910908, 5.407089921784862696, -7.021874999385530280 ) ) ;
#1524 = ORIENTED_EDGE ( 'NONE', *, *, #889, .T. ) ;
#1525 = CARTESIAN_POINT ( 'NONE',  ( -27.24356964375000345, 197.1031250006145399, 0.000000000000000000 ) ) ;
#1526 = CARTESIAN_POINT ( 'NONE',  ( -12.53471296425194836, 132.0226862821014606, 2.311890736173176641 ) ) ;
#1527 = CARTESIAN_POINT ( 'NONE',  ( 19.68408634441910721, 5.407089921784857367, -1.190624999385520022 ) ) ;
#1528 = CARTESIAN_POINT ( 'NONE',  ( 36.97172150469783958, -3.604726614523238837, 160.9206844420862694 ) ) ;
#1529 = CARTESIAN_POINT ( 'NONE',  ( -53.75669563604516554, 209.8844732041981729, -8.500000000000003553 ) ) ;
#1530 = CARTESIAN_POINT ( 'NONE',  ( 15.24356964375000167, 247.5343750006144887, 3.323476615752272600 ) ) ;
#1531 = SURFACE_SIDE_STYLE ('',( #14174 ) ) ;
#1532 = CARTESIAN_POINT ( 'NONE',  ( 19.56230152254411081, -5.196152422706629359, -9.637499998771032139 ) ) ;
#1533 = EDGE_CURVE ( 'NONE', #6008, #20414, #27720, .T. ) ;
#1534 = CARTESIAN_POINT ( 'NONE',  ( -47.22544563604517265, 213.3788001182224718, 3.209657149897419348 ) ) ;
#1535 = CARTESIAN_POINT ( 'NONE',  ( -12.53471296425194836, 141.2226862821014493, 2.311890736173176641 ) ) ;
#1536 = CARTESIAN_POINT ( 'NONE',  ( 10.56230152254410903, 0.000000000000000000, -1.237499998771041110 ) ) ;
#1537 = ORIENTED_EDGE ( 'NONE', *, *, #3843, .T. ) ;
#1538 = VECTOR ( 'NONE', #3418, 1000.000000000000000 ) ;
#1539 =( BOUNDED_CURVE ( )  B_SPLINE_CURVE ( 2, ( #31113, #8365, #19564, #1, #19936, #11568, #23141 ),
 .UNSPECIFIED., .F., .F. ) 
 B_SPLINE_CURVE_WITH_KNOTS ( ( 3, 2, 2, 3 ),
 ( 0.3913043478260868069, 0.3985507246376810975, 0.4057971014492754436, 0.4130434782608697342 ),
 .UNSPECIFIED. ) 
 CURVE ( )  GEOMETRIC_REPRESENTATION_ITEM ( )  RATIONAL_B_SPLINE_CURVE ( ( 1.000000000000003109, 0.8660254037844357100, 1.000000000000000000, 0.8660254037844387076, 1.000000000000000000, 0.8660254037844355990, 1.000000000000003109 ) ) 
 REPRESENTATION_ITEM ( '' )  );
#1540 = DIRECTION ( 'NONE',  ( 0.000000000000000000, -1.000000000000000000, 0.000000000000000000 ) ) ;
#1541 = CARTESIAN_POINT ( 'NONE',  ( -2.908627838312119351, 115.9226862821014521, -15.53471296425195369 ) ) ;
#1542 = CARTESIAN_POINT ( 'NONE',  ( -53.17038769728823411, 207.6069050685337913, 8.469044688360781947 ) ) ;
#1543 = CARTESIAN_POINT ( 'NONE',  ( -5.529263428287477744, 112.4726862821014635, 7.954856959092191815 ) ) ;
#1544 = CARTESIAN_POINT ( 'NONE',  ( 27.00000000000003908, -3.464101615137728185, -2.456249998770948295 ) ) ;
#1545 = CARTESIAN_POINT ( 'NONE',  ( -7.228626920339069173, 20.47268628210144570, 10.49813415415989581 ) ) ;
#1546 = CARTESIAN_POINT ( 'NONE',  ( 13.56230152254411792, -5.196152422706638241, -9.375000000000078160 ) ) ;
#1547 = ORIENTED_EDGE ( 'NONE', *, *, #13873, .F. ) ;
#1548 = LINE ( 'NONE', #19197, #28798 ) ;
#1549 = CARTESIAN_POINT ( 'NONE',  ( -6.594114490232312775, 78.26018628210144357, -6.840914352312096547 ) ) ;
#1550 = DIRECTION ( 'NONE',  ( -0.9925324990730152175, 0.1219804832088933616, 0.000000000000000000 ) ) ;
#1551 = CARTESIAN_POINT ( 'NONE',  ( -5.529263428287297444, 127.5273137178985792, -7.954856959092311719 ) ) ;
#1552 = CARTESIAN_POINT ( 'NONE',  ( -1.926257025242585782E-15, 199.6906250006145456, -31.45816453501075927 ) ) ;
#1553 = CARTESIAN_POINT ( 'NONE',  ( 10.49999999999999467, 215.7563705986615901, -5.555555555555558911 ) ) ;
#1554 = CARTESIAN_POINT ( 'NONE',  ( 27.24356964375000700, 196.8968750006145285, 15.72908226750537075 ) ) ;
#1555 = LINE ( 'NONE', #16722, #15004 ) ;
#1556 = FACE_OUTER_BOUND ( 'NONE', #35166, .T. ) ;
#1557 = CARTESIAN_POINT ( 'NONE',  ( -6.840914352311947333, 62.83981371789855785, -6.594114490232462877 ) ) ;
#1558 = ORIENTED_EDGE ( 'NONE', *, *, #594, .T. ) ;
#1559 = CARTESIAN_POINT ( 'NONE',  ( 26.99999999999999645, 243.4937500012290741, 3.464101615137751278 ) ) ;
#1560 = CARTESIAN_POINT ( 'NONE',  ( 12.46528703574811558, 84.40231371789853654, -2.660918448318005947 ) ) ;
#1561 = CARTESIAN_POINT ( 'NONE',  ( 10.31873187879410736, 0.000000000000000000, -5.596874999385520688 ) ) ;
#1562 = CARTESIAN_POINT ( 'NONE',  ( 20.99999999999999645, 242.9687500012290684, 5.999999999999998224 ) ) ;
#1563 = CARTESIAN_POINT ( 'NONE',  ( 18.12178482187499640, 4.985214923628404904, -5.278124999385486404 ) ) ;
#1564 = CARTESIAN_POINT ( 'NONE',  ( -4.622313124798826500, 50.76481371789855501, 11.61527771782809637 ) ) ;
#1565 = AXIS2_PLACEMENT_3D ( 'NONE', #36851, #23023, #17153 ) ;
#1566 = EDGE_CURVE ( 'NONE', #3429, #35216, #33057, .T. ) ;
#1567 = APPLICATION_CONTEXT ( 'automotive_design' ) ;
#1568 = ORIENTED_EDGE ( 'NONE', *, *, #4516, .F. ) ;
#1569 = CARTESIAN_POINT ( 'NONE',  ( 23.87821517812499650, 4.985214923628404904, -7.040624999385459049 ) ) ;
#1570 = CARTESIAN_POINT ( 'NONE',  ( -8.715434833791929847, 23.06018628210145138, -8.962234695871762469 ) ) ;
#1571 = CARTESIAN_POINT ( 'NONE',  ( -34.55877896937849414, 211.6261429550004891, -6.530955311639245586 ) ) ;
#1572 = CARTESIAN_POINT ( 'NONE',  ( -57.91294563604515133, 214.6737587650350747, -4.842901733360249317 ) ) ;
#1573 =( BOUNDED_CURVE ( )  B_SPLINE_CURVE ( 2, ( #20156, #25464, #8226, #17130, #28666, #34364, #31705 ),
 .UNSPECIFIED., .F., .F. ) 
 B_SPLINE_CURVE_WITH_KNOTS ( ( 3, 2, 2, 3 ),
 ( 0.6086956521739121939, 0.6159420289855062070, 0.6231884057971003310, 0.6304347826086944551 ),
 .UNSPECIFIED. ) 
 CURVE ( )  GEOMETRIC_REPRESENTATION_ITEM ( )  RATIONAL_B_SPLINE_CURVE ( ( 1.000000000000016431, 0.8660254037844222763, 1.000000000000000000, 0.8660254037844387076, 1.000000000000000000, 0.8660254037844612451, 0.9999999999999774625 ) ) 
 REPRESENTATION_ITEM ( '' )  );
#1574 = AXIS2_PLACEMENT_3D ( 'NONE', #26100, #8857, #131 ) ;
#1575 = CARTESIAN_POINT ( 'NONE',  ( 10.69584247140429589, 67.15231371789855075, 6.932735513424201024 ) ) ;
#1576 = EDGE_CURVE ( 'NONE', #14024, #22269, #24528, .T. ) ;
#1577 = CARTESIAN_POINT ( 'NONE',  ( -45.84747103062156981, 212.3500491399821613, -3.839350919129076445 ) ) ;
#1579 = ADVANCED_FACE ( 'NONE', ( #30215 ), #27924, .F. ) ;
#1578 = CARTESIAN_POINT ( 'NONE',  ( -57.72247103062156270, 206.6499508600178672, 5.571401726697986057 ) ) ;
#1580 = CARTESIAN_POINT ( 'NONE',  ( 13.50000000000001421, 195.7625000012290570, 23.38268590217984055 ) ) ;
#1581 = CARTESIAN_POINT ( 'NONE',  ( 27.81970530529572372, -5.196152422706632912, 162.3707280659671994 ) ) ;
#1582 = CARTESIAN_POINT ( 'NONE',  ( 3.257655550456945548, 31.50231371789854862, 15.46528703574811736 ) ) ;
#1583 = CARTESIAN_POINT ( 'NONE',  ( -51.97544563604517265, 216.3070033484980854, 6.137860380172893926 ) ) ;
#1584 = CARTESIAN_POINT ( 'NONE',  ( 24.00000000000000000, -5.196152422706629359, -7.950000000000012612 ) ) ;
#1585 = CARTESIAN_POINT ( 'NONE',  ( -11.61527771782819940, 67.33518628210144641, 4.622313124798574258 ) ) ;
#1586 = CARTESIAN_POINT ( 'NONE',  ( 13.23911966647218996, 25.64768628210144286, -8.632099005475504683 ) ) ;
#1587 = AXIS2_PLACEMENT_3D ( 'NONE', #16076, #33314, #36516 ) ;
#1589 = EDGE_CURVE ( 'NONE', #25013, #11771, #16193, .T. ) ;
#1588 = CARTESIAN_POINT ( 'NONE',  ( 16.56230152254411436, 6.928203230275514990, -3.262500000000057021 ) ) ;
#1590 = CARTESIAN_POINT ( 'NONE',  ( -28.86277965861013328, 202.5120511701786654, -2.828156894100585461 ) ) ;
#1591 = ORIENTED_EDGE ( 'NONE', *, *, #30400, .T. ) ;
#1592 = CARTESIAN_POINT ( 'NONE',  ( -10.83675517735155047, 32.26018628210145067, -11.08355503943142750 ) ) ;
#1593 = CARTESIAN_POINT ( 'NONE',  ( -1.926257025242585782E-15, 196.5406250006145399, -31.45816453501076637 ) ) ;
#1594 = DIRECTION ( 'NONE',  ( -1.558072081575740353E-16, -1.134704379232807653E-16, -1.000000000000000000 ) ) ;
#1595 = DIRECTION ( 'NONE',  ( 0.000000000000000000, 0.000000000000000000, -1.000000000000000000 ) ) ;
#1596 = CARTESIAN_POINT ( 'NONE',  ( -33.18080436395490551, 203.5000000000000000, -0.1155267958017335561 ) ) ;
#1597 = CARTESIAN_POINT ( 'NONE',  ( -27.00000000000000355, 195.5000000000000000, 0.000000000000000000 ) ) ;
#1598 = CARTESIAN_POINT ( 'NONE',  ( 27.00000000000001421, 196.2500000012290116, 15.58845726811988897 ) ) ;
#1599 = CARTESIAN_POINT ( 'NONE',  ( 21.00000000000000000, 247.4968750006145513, -6.646953231504538984 ) ) ;
#1600 = CARTESIAN_POINT ( 'NONE',  ( -9.500000000000005329, 126.0898137178985650, 0.1745138560723101806 ) ) ;
#1601 = CARTESIAN_POINT ( 'NONE',  ( 23.87821517812500005, 243.7093750006145285, 4.985214923628404016 ) ) ;
#1602 = EDGE_LOOP ( 'NONE', ( #5890, #19433, #27846, #21433 ) ) ;
#1603 = DIRECTION ( 'NONE',  ( 0.000000000000000000, 0.000000000000000000, 1.000000000000000000 ) ) ;
#1604 = CARTESIAN_POINT ( 'NONE',  ( 14.99999999999968203, -3.464101615137573198, -7.106249998770961973 ) ) ;
#1605 = CARTESIAN_POINT ( 'NONE',  ( -4.944772684328424539, 137.0148137178985621, -11.48171059495408031 ) ) ;
#1606 = CARTESIAN_POINT ( 'NONE',  ( 10.31873187879410736, 0.000000000000000000, -6.890624999385530636 ) ) ;
#1607 = CARTESIAN_POINT ( 'NONE',  ( 24.75598086634022010, 0.000000000000000000, 164.5679854722048958 ) ) ;
#1608 = CARTESIAN_POINT ( 'NONE',  ( 13.56230152254411259, -5.196152422706632912, -2.512499998771011711 ) ) ;
#1609 = CARTESIAN_POINT ( 'NONE',  ( 26.99999999999999645, 198.4625000000000341, -15.58845726811990495 ) ) ;
#1610 = VERTEX_POINT ( 'NONE', #12971 ) ;
#1611 = CARTESIAN_POINT ( 'NONE',  ( 2.311890736173175753, 37.72268628210144215, 12.53471296425194659 ) ) ;
#1612 = ORIENTED_EDGE ( 'NONE', *, *, #18908, .T. ) ;
#1613 = ORIENTED_EDGE ( 'NONE', *, *, #16584, .F. ) ;
#1614 = CARTESIAN_POINT ( 'NONE',  ( 21.00000000000000000, -6.928203230275506996, -5.231249998770948650 ) ) ;
#1615 = CARTESIAN_POINT ( 'NONE',  ( 15.24356964374999990, 0.000000000000000000, -1.040624999385481031 ) ) ;
#1616 = DIRECTION ( 'NONE',  ( -0.000000000000000000, -0.000000000000000000, -1.000000000000000000 ) ) ;
#1617 = CARTESIAN_POINT ( 'NONE',  ( -27.00000000000000355, 196.3625000000000114, -15.58845726811989429 ) ) ;
#1618 = CARTESIAN_POINT ( 'NONE',  ( 26.75643035624999655, 3.323476615752271712, -9.328124999385446259 ) ) ;
#1619 = CARTESIAN_POINT ( 'NONE',  ( -4.944772684328673229, 75.38518628210144357, 11.48171059495397728 ) ) ;
#1620 = CARTESIAN_POINT ( 'NONE',  ( -14.38691631536193860, 7.064813717898548617, -5.770363421894132649 ) ) ;
#1621 = ADVANCED_FACE ( 'NONE', ( #36077 ), #7283, .F. ) ;
#1622 = CARTESIAN_POINT ( 'NONE',  ( -13.49999999999998401, 197.3750000000000284, 23.38268590217985476 ) ) ;
#1623 = CARTESIAN_POINT ( 'NONE',  ( 16.22935424640221669, 222.7217220096020469, 3.659938751166898374 ) ) ;
#1624 = CARTESIAN_POINT ( 'NONE',  ( -54.35044563604515844, 206.6211998817775566, -3.209657149897419348 ) ) ;
#1625 = DIRECTION ( 'NONE',  ( 0.000000000000000000, 0.000000000000000000, 1.000000000000000000 ) ) ;
#1626 = CARTESIAN_POINT ( 'NONE',  ( 25.18083362879543685, -3.464101615137757051, 166.6294265203033262 ) ) ;
#1627 = CARTESIAN_POINT ( 'NONE',  ( 12.53471296425189330, 121.7773137178985792, 2.311890736173451977 ) ) ;
#1628 = CARTESIAN_POINT ( 'NONE',  ( -48.42038769728821990, 208.1428034533959703, 6.469044688360770401 ) ) ;
#1630 = EDGE_CURVE ( 'NONE', #12051, #26056, #3822, .T. ) ;
#1629 = CARTESIAN_POINT ( 'NONE',  ( -51.58705436395489841, 203.8621396198270475, -6.307003348497942419 ) ) ;
#1631 = SHAPE_DEFINITION_REPRESENTATION ( #19546, #8404 ) ;
#1632 = CARTESIAN_POINT ( 'NONE',  ( 20.99999999999999645, 6.646953231504538984, -1.715624999385482852 ) ) ;
#1633 = CARTESIAN_POINT ( 'NONE',  ( -27.24356964374999990, 196.1656250006145399, -15.72908226750537786 ) ) ;
#1634 = CARTESIAN_POINT ( 'NONE',  ( 0.1745138560722461762, 105.3898137178985479, 15.50000000000000533 ) ) ;
#1635 = CARTESIAN_POINT ( 'NONE',  ( -51.38169563604516554, 210.1155267958017703, 6.500000000000000888 ) ) ;
#1636 = AXIS2_PLACEMENT_3D ( 'NONE', #17636, #21747, #29554 ) ;
#1637 = ORIENTED_EDGE ( 'NONE', *, *, #15360, .F. ) ;
#1638 = CARTESIAN_POINT ( 'NONE',  ( 28.25112623189659544, -5.196152422706632912, 167.3018918215213660 ) ) ;
#1639 = CARTESIAN_POINT ( 'NONE',  ( -12.46528703574805697, 123.3976862821014606, -2.660918448318280838 ) ) ;
#1640 = CARTESIAN_POINT ( 'NONE',  ( 8.927990412390657937, 80.27268628210143220, -13.04141134922759804 ) ) ;
#1641 = DIRECTION ( 'NONE',  ( -0.000000000000000000, -1.000000000000000000, -0.000000000000000000 ) ) ;
#1642 = CARTESIAN_POINT ( 'NONE',  ( 37.32470226282583781, -3.604726614523238837, 164.9552729693578215 ) ) ;
#1643 = CARTESIAN_POINT ( 'NONE',  ( -3.257655550457281723, 84.29768628210146630, 15.46528703574804986 ) ) ;
#1644 = CARTESIAN_POINT ( 'NONE',  ( -52.57663769728823411, 204.3130714775002730, 3.149950860017883603 ) ) ;
#1645 = CARTESIAN_POINT ( 'NONE',  ( 13.44051670066911086, 5.407089921784856479, -4.715624999385548577 ) ) ;
#1646 = CARTESIAN_POINT ( 'NONE',  ( 9.500000000000005329, 44.91018628210144215, 0.1745138560725188748 ) ) ;
#1647 = CARTESIAN_POINT ( 'NONE',  ( 15.00000000000034461, -3.464101615137956003, -3.562499999999996447 ) ) ;
#1648 = CARTESIAN_POINT ( 'NONE',  ( -37.13913769728823411, 205.8500491399820760, -7.418979330068584233 ) ) ;
#1649 = CARTESIAN_POINT ( 'NONE',  ( 19.68408634441911786, -5.407089921784861808, -9.496874999385534366 ) ) ;
#1650 = CARTESIAN_POINT ( 'NONE',  ( -12.53471296425194836, 67.62268628210145494, 2.311890736173176641 ) ) ;
#1651 = CARTESIAN_POINT ( 'NONE',  ( 16.07192114941521766, -3.422577806627481234, -8.000000000000001776 ) ) ;
#1652 = FACE_OUTER_BOUND ( 'NONE', #9339, .T. ) ;
#1654 = CARTESIAN_POINT ( 'NONE',  ( 10.31873187879410381, 3.604726614523240613, -0.2343749993854903346 ) ) ;
#1653 = CARTESIAN_POINT ( 'NONE',  ( -9.465287035748065847, 49.79768628210144499, -2.064181346179273735 ) ) ;
#1655 = CARTESIAN_POINT ( 'NONE',  ( 6.123233995736766282E-16, 0.000000000000000000, 5.000000000000000000 ) ) ;
#1656 = ORIENTED_EDGE ( 'NONE', *, *, #14505, .T. ) ;
#1657 = CARTESIAN_POINT ( 'NONE',  ( 18.00000000000000000, 5.196152422706630247, -3.225000000000005862 ) ) ;
#1658 = CARTESIAN_POINT ( 'NONE',  ( 24.71512661192725702, -3.604726614523244610, 164.1010192074743941 ) ) ;
#1659 = CARTESIAN_POINT ( 'NONE',  ( 33.68901826208886519, 5.196152422706637353, 160.6150026693684367 ) ) ;
#1660 = CARTESIAN_POINT ( 'NONE',  ( 26.99999999999999645, 245.6875000000000000, 3.464101615137751278 ) ) ;
#1661 = DIRECTION ( 'NONE',  ( 1.000000000000000000, 0.000000000000000000, 0.000000000000000000 ) ) ;
#1662 = CARTESIAN_POINT ( 'NONE',  ( -12.53471296425189152, 89.57731371789856212, -2.311890736173453753 ) ) ;
#1663 = CARTESIAN_POINT ( 'NONE',  ( -11.48171059495397373, 77.68518628210145494, -4.944772684328680334 ) ) ;
#1664 = ORIENTED_EDGE ( 'NONE', *, *, #36317, .F. ) ;
#1665 = EDGE_LOOP ( 'NONE', ( #22970, #4177, #13653, #15801, #24714, #31155, #33788, #28685 ) ) ;
#1666 = CARTESIAN_POINT ( 'NONE',  ( 13.49999999999999645, 199.0625000012290400, -23.38268590217984766 ) ) ;
#1667 = CARTESIAN_POINT ( 'NONE',  ( -26.99999999999999645, 196.8875000000000171, 15.58845726811991561 ) ) ;
#1668 = AXIS2_PLACEMENT_3D ( 'NONE', #15479, #33098, #18715 ) ;
#1669 = CARTESIAN_POINT ( 'NONE',  ( 13.23911966647199812, 57.95231371789854791, 8.632099005475788900 ) ) ;
#1670 = CARTESIAN_POINT ( 'NONE',  ( 21.00000000000000000, 6.646953231504538984, -7.565624999385492266 ) ) ;
#1671 = CARTESIAN_POINT ( 'NONE',  ( 15.24356964374999990, 244.4218750006145058, -3.323476615752268604 ) ) ;
#1672 = CARTESIAN_POINT ( 'NONE',  ( -50.39955436395490551, 213.3788001182225003, -3.209657149897400252 ) ) ;
#1673 = CARTESIAN_POINT ( 'NONE',  ( 31.44888410865908668, 6.928203230275514990, 169.4312918674742434 ) ) ;
#1674 = CARTESIAN_POINT ( 'NONE',  ( -3.474262827703527901, 59.96481371789855075, 8.843639120294245259 ) ) ;
#1675 = CARTESIAN_POINT ( 'NONE',  ( 19.68408634441910721, -5.407089921784855591, -8.990624999385548932 ) ) ;
#1676 = CARTESIAN_POINT ( 'NONE',  ( -6.594114490232462877, 88.13981371789856212, 6.840914352311949109 ) ) ;
#1677 = CARTESIAN_POINT ( 'NONE',  ( 20.99999999999999645, 240.1843750006145513, -6.646953231504538984 ) ) ;
#1678 = CARTESIAN_POINT ( 'NONE',  ( -7.228626920338836470, 26.32731371789854791, -10.49813415416005213 ) ) ;
#1679 = CARTESIAN_POINT ( 'NONE',  ( -7.228626920339069173, 84.87268628210146915, 10.49813415415989581 ) ) ;
#1680 = CARTESIAN_POINT ( 'NONE',  ( 22.56230152254409660, 3.464101615137755275, -9.074999998770975296 ) ) ;
#1681 = DIRECTION ( 'NONE',  ( -0.000000000000000000, -0.000000000000000000, -1.000000000000000000 ) ) ;
#1682 = CARTESIAN_POINT ( 'NONE',  ( 33.83730346391489263, 5.407089921784857367, 160.9125861580968149 ) ) ;
#1683 = CARTESIAN_POINT ( 'NONE',  ( 13.44051670066911264, -5.407089921784865361, -5.521874999385528504 ) ) ;
#1684 = CARTESIAN_POINT ( 'NONE',  ( -13.49999999999998401, 195.6875000012290400, 23.38268590217985476 ) ) ;
#1685 = CARTESIAN_POINT ( 'NONE',  ( 9.534712964251941258, 90.62268628210145494, -1.715153634034235708 ) ) ;
#1686 = DIRECTION ( 'NONE',  ( -0.000000000000000000, -1.000000000000000000, -0.000000000000000000 ) ) ;
#1687 = CARTESIAN_POINT ( 'NONE',  ( 4.944772684328679446, 125.9851862821014521, -11.48171059495397373 ) ) ;
#1688 = LINE ( 'NONE', #24815, #8796 ) ;
#1689 = CARTESIAN_POINT ( 'NONE',  ( 26.75643035624999655, 240.9718750006145171, -7.049594010296217766E-16 ) ) ;
#1690 = ORIENTED_EDGE ( 'NONE', *, *, #33509, .F. ) ;
#1691 = CARTESIAN_POINT ( 'NONE',  ( 34.15106413780644345, 5.407089921784857367, 164.4988870712271023 ) ) ;
#1692 = VECTOR ( 'NONE', #23370, 1000.000000000000000 ) ;
#1693 = CARTESIAN_POINT ( 'NONE',  ( 15.24356964374999990, 0.000000000000000000, -4.640624999385472904 ) ) ;
#1694 = CARTESIAN_POINT ( 'NONE',  ( 5.778771075727756162E-15, 198.6218750006145513, 31.45816453501076637 ) ) ;
#1695 = CARTESIAN_POINT ( 'NONE',  ( 20.99999999999999645, 185.0294372515228645, 0.000000000000000000 ) ) ;
#1696 = CARTESIAN_POINT ( 'NONE',  ( 22.56230152254410726, 7.347880794884117764E-16, -9.112499998771033560 ) ) ;
#1697 = CARTESIAN_POINT ( 'NONE',  ( 15.24356964374999990, 243.0718750006145115, -3.323476615752268604 ) ) ;
#1698 = CARTESIAN_POINT ( 'NONE',  ( 15.00000000000000355, 7.347880794884112834E-16, -8.000000000000000000 ) ) ;
#1699 = EDGE_CURVE ( 'NONE', #7705, #7058, #22066, .T. ) ;
#1700 = CARTESIAN_POINT ( 'NONE',  ( 4.944772684328420986, 132.4148137178985678, 11.48171059495408208 ) ) ;
#1701 = CARTESIAN_POINT ( 'NONE',  ( 5.778771075727756162E-15, 195.9218750006145342, 31.45816453501076637 ) ) ;
#1703 = ORIENTED_EDGE ( 'NONE', *, *, #14020, .T. ) ;
#1702 = ORIENTED_EDGE ( 'NONE', *, *, #27762, .F. ) ;
#1704 = CARTESIAN_POINT ( 'NONE',  ( 23.87821517812499650, 244.1968750006145115, -4.985214923628404904 ) ) ;
#1705 = CARTESIAN_POINT ( 'NONE',  ( -12.50000000000000355, 15.68981371789854329, 0.1745138560722786503 ) ) ;
#1706 = CARTESIAN_POINT ( 'NONE',  ( 21.00000000000000000, 6.646953231504538984, -4.753124999385462068 ) ) ;
#1707 = CARTESIAN_POINT ( 'NONE',  ( 15.46528703574811736, 112.0023137178985451, -3.257655550456947768 ) ) ;
#1708 = CARTESIAN_POINT ( 'NONE',  ( 22.56230152254403265, -3.464101615137814338, -0.2625000000000441980 ) ) ;
#1709 = CARTESIAN_POINT ( 'NONE',  ( 21.00000000000000000, 6.928203230275506996, -9.506249998770956111 ) ) ;
#1710 = CLOSED_SHELL ( 'NONE', ( #11763, #6880, #29831, #34272, #5221, #24168, #34342, #28757, #8109, #22910 ) ) ;
#1711 = CIRCLE ( 'NONE', #36816, 4.000000000000003553 ) ;
#1712 = CARTESIAN_POINT ( 'NONE',  ( 13.44051670066911086, 5.407089921784862696, -5.671874999385540406 ) ) ;
#1713 = ORIENTED_EDGE ( 'NONE', *, *, #10791, .T. ) ;
#1714 = CARTESIAN_POINT ( 'NONE',  ( -27.24356964375001056, 194.8294844423495533, -9.915847621322177119 ) ) ;
#1715 = CARTESIAN_POINT ( 'NONE',  ( -8.715434833791929847, 124.2601862821014578, -8.962234695871762469 ) ) ;
#1716 = CARTESIAN_POINT ( 'NONE',  ( -79.65000000000000568, 210.0000000000000000, 5.000000000000000888 ) ) ;
#1717 = CARTESIAN_POINT ( 'NONE',  ( 30.82381401619432637, -7.209453229046482114, 162.2867080177096852 ) ) ;
#1718 = ADVANCED_FACE ( 'NONE', ( #28616 ), #14601, .T. ) ;
#1719 = CARTESIAN_POINT ( 'NONE',  ( -49.60044563604517265, 203.6929966515019430, -6.137860380172892150 ) ) ;
#1720 = CARTESIAN_POINT ( 'NONE',  ( 26.75643035624999655, 247.2718750006145001, -7.049594010296217766E-16 ) ) ;
#1721 =( NAMED_UNIT ( * ) PLANE_ANGLE_UNIT ( ) SI_UNIT ( $, .RADIAN. ) );
#1722 = CARTESIAN_POINT ( 'NONE',  ( 22.56230152254410015, 7.347880794884117764E-16, -2.812499998771006204 ) ) ;
#1723 = CARTESIAN_POINT ( 'NONE',  ( -37.32961230271184405, 211.3212981617417938, 4.469044688360757966 ) ) ;
#1724 = CARTESIAN_POINT ( 'NONE',  ( -10.49813415415989581, 133.1726862821014663, -7.228626920339068285 ) ) ;
#1725 = CARTESIAN_POINT ( 'NONE',  ( 22.56230152254410015, 3.464101615137755275, -0.5249999987710241012 ) ) ;
#1727 = EDGE_LOOP ( 'NONE', ( #26472, #2358, #397, #19028 ) ) ;
#1726 = EDGE_CURVE ( 'NONE', #9537, #27444, #10675, .T. ) ;
#1728 = DIRECTION ( 'NONE',  ( 0.08715574274765150453, 0.000000000000000000, 0.9961946980917461003 ) ) ;
#1729 = CARTESIAN_POINT ( 'NONE',  ( 10.56230152254411081, 0.000000000000000000, -4.837499998771033205 ) ) ;
#1730 = CARTESIAN_POINT ( 'NONE',  ( -3.257655550457281723, 121.0976862821014635, 15.46528703574804986 ) ) ;
#1731 = CARTESIAN_POINT ( 'NONE',  ( 13.49999999999999645, 198.0500000000000114, -23.38268590217984766 ) ) ;
#1732 = CARTESIAN_POINT ( 'NONE',  ( -2.660918448318275509, 19.89768628210143575, 12.46528703574805874 ) ) ;
#1733 = CARTESIAN_POINT ( 'NONE',  ( 19.56230152254412147, -5.196152422706635576, -9.300000000000057554 ) ) ;
#1734 = VECTOR ( 'NONE', #11519, 1000.000000000000000 ) ;
#1735 = ORIENTED_EDGE ( 'NONE', *, *, #15718, .F. ) ;
#1736 = CARTESIAN_POINT ( 'NONE',  ( 15.02283181144952628, 7.347880794884122694E-16, 50.52293445648592751 ) ) ;
#1737 = CARTESIAN_POINT ( 'NONE',  ( -8.710071997420127943, 86.88518628210145778, -3.796722387233380402 ) ) ;
#1738 = SURFACE_STYLE_FILL_AREA ( #16160 ) ;
#1739 = CARTESIAN_POINT ( 'NONE',  ( 5.529263428287300108, 122.9273137178985422, 7.954856959092309943 ) ) ;
#1740 = CARTESIAN_POINT ( 'NONE',  ( -13.62178482187500528, 197.0281250006145228, -23.59362340125807123 ) ) ;
#1742 = CARTESIAN_POINT ( 'NONE',  ( -49.64999999999999147, 244.5000000000000000, 5.000000000000000888 ) ) ;
#1741 =( BOUNDED_CURVE ( )  B_SPLINE_CURVE ( 2, ( #21748, #9984, #1448, #6767, #30269, #15304, #18727, #13212, #12645 ),
 .UNSPECIFIED., .F., .F. ) 
 B_SPLINE_CURVE_WITH_KNOTS ( ( 3, 2, 2, 2, 3 ),
 ( 0.3958333333333333703, 0.4027777777777777901, 0.4166666666666666852, 0.4305555555555555802, 0.4375000000000000000 ),
 .UNSPECIFIED. ) 
 CURVE ( )  GEOMETRIC_REPRESENTATION_ITEM ( )  RATIONAL_B_SPLINE_CURVE ( ( 0.9330127018922194093, 0.9330127018922196314, 1.000000000000000000, 0.8660254037844387076, 1.000000000000000000, 0.8660254037844387076, 1.000000000000000000, 0.9330127018922194093, 0.9330127018922194093 ) ) 
 REPRESENTATION_ITEM ( '' )  );
#1743 = CARTESIAN_POINT ( 'NONE',  ( -27.24356964374999635, 198.5468750006145626, 15.72908226750539384 ) ) ;
#1744 = DIRECTION ( 'NONE',  ( 0.000000000000000000, 0.000000000000000000, -1.000000000000000000 ) ) ;
#1745 = CARTESIAN_POINT ( 'NONE',  ( 24.00000000000000000, 243.8500000000000227, 5.196152422706629359 ) ) ;
#1746 = CARTESIAN_POINT ( 'NONE',  ( 9.500000000000005329, 57.08981371789855075, -0.1745138560723090149 ) ) ;
#1747 = CARTESIAN_POINT ( 'NONE',  ( 15.00000000000000178, -3.464101615137757051, -6.712500000000003020 ) ) ;
#1748 = ORIENTED_EDGE ( 'NONE', *, *, #10047, .T. ) ;
#1749 = CARTESIAN_POINT ( 'NONE',  ( 23.99999999999999645, 241.3562500012290286, -5.196152422706631135 ) ) ;
#1750 = CARTESIAN_POINT ( 'NONE',  ( 11.48171059495408208, 74.91481371789855359, -4.944772684328420986 ) ) ;
#1751 = EDGE_CURVE ( 'NONE', #24079, #15328, #5891, .T. ) ;
#1752 = CARTESIAN_POINT ( 'NONE',  ( 13.44051670066910908, 5.407089921784862696, -7.021874999385530280 ) ) ;
#1753 = CARTESIAN_POINT ( 'NONE',  ( 5.778771075727756162E-15, 199.4656250006145797, 31.45816453501075927 ) ) ;
#1754 = CARTESIAN_POINT ( 'NONE',  ( 21.00000000000000000, 6.646953231504538984, -7.565624999385492266 ) ) ;
#1755 = CARTESIAN_POINT ( 'NONE',  ( 2.311890736173452865, 27.47731371789855004, -12.53471296425189152 ) ) ;
#1756 = EDGE_LOOP ( 'NONE', ( #2378, #1797, #29965, #24577 ) ) ;
#1757 = CARTESIAN_POINT ( 'NONE',  ( 23.87821517812499650, 4.985214923628404904, -7.490624999385464555 ) ) ;
#1758 = CARTESIAN_POINT ( 'NONE',  ( 7.228626920339068285, 25.07268628210144712, -10.49813415415989581 ) ) ;
#1759 = EDGE_CURVE ( 'NONE', #19165, #27793, #2654, .T. ) ;
#1760 = CARTESIAN_POINT ( 'NONE',  ( 37.64499961742345135, 3.604726614523243278, 168.6162884848450005 ) ) ;
#1761 =( BOUNDED_CURVE ( )  B_SPLINE_CURVE ( 2, ( #33202, #15774, #36034, #10078, #28067, #7429, #33389, #27880, #10632 ),
 .UNSPECIFIED., .F., .F. ) 
 B_SPLINE_CURVE_WITH_KNOTS ( ( 3, 2, 2, 2, 3 ),
 ( 0.7708333333333333703, 0.7777777777777777901, 0.7916666666666666297, 0.8055555555555555802, 0.8125000000000000000 ),
 .UNSPECIFIED. ) 
 CURVE ( )  GEOMETRIC_REPRESENTATION_ITEM ( )  RATIONAL_B_SPLINE_CURVE ( ( 0.9330127018922192983, 0.9330127018922198534, 1.000000000000000000, 0.8660254037844387076, 1.000000000000000000, 0.8660254037844387076, 1.000000000000000000, 0.9330127018922194093, 0.9330127018922194093 ) ) 
 REPRESENTATION_ITEM ( '' )  );
#1762 = CARTESIAN_POINT ( 'NONE',  ( -49.60044563604517265, 205.1570982666397072, -4.673758765035155527 ) ) ;
#1763 = ADVANCED_FACE ( 'NONE', ( #26334 ), #19416, .T. ) ;
#1764 = CARTESIAN_POINT ( 'NONE',  ( 27.00000000000052580, -3.464101615137444412, -7.462499999999999467 ) ) ;
#1765 = CARTESIAN_POINT ( 'NONE',  ( 12.46528703574811558, 75.20231371789856212, -2.660918448318005503 ) ) ;
#1766 = CARTESIAN_POINT ( 'NONE',  ( -34.76413769728823411, 212.1499508600178387, 3.954877714930865817 ) ) ;
#1767 = CARTESIAN_POINT ( 'NONE',  ( -58.51413769728823411, 213.1499508600178672, 5.686928522499718142 ) ) ;
#1768 = CYLINDRICAL_SURFACE ( 'NONE', #5822, 5.999999999999994671 ) ;
#1769 = CARTESIAN_POINT ( 'NONE',  ( -12.83399793243727238, 216.5739059620414082, -4.792798303949182603 ) ) ;
#1770 = CARTESIAN_POINT ( 'NONE',  ( 13.23911966647199812, 48.75231371789854506, 8.632099005475788900 ) ) ;
#1771 = CARTESIAN_POINT ( 'NONE',  ( -49.60044563604517265, 203.6929966515019430, -6.137860380172892150 ) ) ;
#1772 = DIRECTION ( 'NONE',  ( 0.000000000000000000, -0.000000000000000000, 1.000000000000000000 ) ) ;
#1773 = CARTESIAN_POINT ( 'NONE',  ( 10.69584247140445221, 62.44768628210145778, -6.932735513423970097 ) ) ;
#1774 = CARTESIAN_POINT ( 'NONE',  ( 15.50000000000000533, 8.110186282101443211, 0.1745138560725827404 ) ) ;
#1776 = EDGE_CURVE ( 'NONE', #14300, #10569, #1955, .T. ) ;
#1775 = CARTESIAN_POINT ( 'NONE',  ( 10.56230152254411614, -3.464101615137761048, -1.312500000000054401 ) ) ;
#1777 = CYLINDRICAL_SURFACE ( 'NONE', #7695, 5.999999999999994671 ) ;
#1778 = ORIENTED_EDGE ( 'NONE', *, *, #29074, .T. ) ;
#1779 = CARTESIAN_POINT ( 'NONE',  ( 0.1745138560725837118, 33.41018628210144925, -15.50000000000000533 ) ) ;
#1780 = CARTESIAN_POINT ( 'NONE',  ( -13.62178482187498396, 195.3781250006145171, 23.59362340125808188 ) ) ;
#1781 = CARTESIAN_POINT ( 'NONE',  ( -27.24356964375000345, 197.1593750006145456, 0.000000000000000000 ) ) ;
#1782 = DIRECTION ( 'NONE',  ( 1.000000000000000000, 0.000000000000000000, 0.000000000000000000 ) ) ;
#1783 = DIRECTION ( 'NONE',  ( 0.000000000000000000, 0.000000000000000000, 1.000000000000000000 ) ) ;
#1784 = CARTESIAN_POINT ( 'NONE',  ( -2.311890736173176641, 5.522686282101451738, -12.53471296425194836 ) ) ;
#1785 = CARTESIAN_POINT ( 'NONE',  ( 21.00000000000000000, 247.0468750006145058, -6.646953231504538984 ) ) ;
#1786 = CARTESIAN_POINT ( 'NONE',  ( -6.840914352311947333, 118.0398137178985536, -6.594114490232462877 ) ) ;
#1787 = CARTESIAN_POINT ( 'NONE',  ( 26.75643035624999655, 243.2968750006145342, 3.323476615752267271 ) ) ;
#1788 = ORIENTED_EDGE ( 'NONE', *, *, #3607, .F. ) ;
#1789 = SURFACE_STYLE_USAGE ( .BOTH. , #34002 ) ;
#1790 = CARTESIAN_POINT ( 'NONE',  ( 15.00000000000000000, 248.7062500012290229, 0.000000000000000000 ) ) ;
#1791 = ADVANCED_FACE ( 'NONE', ( #17077 ), #6254, .F. ) ;
#1792 = CARTESIAN_POINT ( 'NONE',  ( -6.422845572874366304, 142.9999999999996305, 10.72508787064079172 ) ) ;
#1793 = CARTESIAN_POINT ( 'NONE',  ( 19.68408634441910721, 5.407089921784857367, -8.390624999385531524 ) ) ;
#1794 = CARTESIAN_POINT ( 'NONE',  ( 34.05955060792140188, -5.407089921784855591, 163.4528826382307614 ) ) ;
#1795 = DIRECTION ( 'NONE',  ( 0.000000000000000000, 0.000000000000000000, 1.000000000000000000 ) ) ;
#1796 = CARTESIAN_POINT ( 'NONE',  ( 13.50000000000001421, 198.3499999999999943, 23.38268590217984055 ) ) ;
#1797 = ORIENTED_EDGE ( 'NONE', *, *, #17252, .T. ) ;
#1798 = CARTESIAN_POINT ( 'NONE',  ( 10.69584247140445221, 34.84768628210144215, -6.932735513423970097 ) ) ;
#1799 = ORIENTED_EDGE ( 'NONE', *, *, #664, .T. ) ;
#1800 = ORIENTED_EDGE ( 'NONE', *, *, #8770, .F. ) ;
#1801 = CARTESIAN_POINT ( 'NONE',  ( 26.99999999999999645, 7.347880794884117764E-16, -6.018749998770944742 ) ) ;
#1802 = CARTESIAN_POINT ( 'NONE',  ( -81.00000000000002842, 206.0000000000000000, -2.499999999999998668 ) ) ;
#1803 = CARTESIAN_POINT ( 'NONE',  ( 19.39230484541326760, 242.0486538117967257, 5.999999999999999112 ) ) ;
#1804 = DIRECTION ( 'NONE',  ( 0.9961946980917462113, 0.000000000000000000, -0.08715574274765118534 ) ) ;
#1805 = CARTESIAN_POINT ( 'NONE',  ( 15.24356964375000167, -3.323476615752272600, -9.103124999385496352 ) ) ;
#1806 = CARTESIAN_POINT ( 'NONE',  ( -8.715434833791929847, 78.26018628210144357, -8.962234695871762469 ) ) ;
#1807 = CARTESIAN_POINT ( 'NONE',  ( 10.83675517735155225, 138.0601862821014549, 11.08355503943142573 ) ) ;
#1808 = CARTESIAN_POINT ( 'NONE',  ( 15.61591388112558398, 224.3575629836673500, -2.655215585728295302 ) ) ;
#1809 = CARTESIAN_POINT ( 'NONE',  ( -56.72544563604517265, 213.3788001182224718, 3.209657149897419348 ) ) ;
#1810 = DIRECTION ( 'NONE',  ( -0.000000000000000000, 1.000000000000000000, -0.000000000000000000 ) ) ;
#1811 = AXIS2_PLACEMENT_3D ( 'NONE', #26939, #970, #24112 ) ;
#1812 = CARTESIAN_POINT ( 'NONE',  ( 25.25600545691528254, 0.000000000000000000, 167.4886444474074381 ) ) ;
#1813 = CARTESIAN_POINT ( 'NONE',  ( 12.46528703574811558, 121.2023137178985621, -2.660918448318005503 ) ) ;
#1814 = CARTESIAN_POINT ( 'NONE',  ( -46.24330436395489841, 210.1155267958017134, -6.500000000000000888 ) ) ;
#1815 = CARTESIAN_POINT ( 'NONE',  ( -61.28497103062156981, 202.6965474657331185, -4.350049139982091084 ) ) ;
#1816 = CARTESIAN_POINT ( 'NONE',  ( 26.75643035624999655, -3.323476615752267271, -0.9656249993854794100 ) ) ;
#1817 = CARTESIAN_POINT ( 'NONE',  ( -27.24356964374999635, 196.2406250006145285, 15.72908226750539384 ) ) ;
#1818 = CARTESIAN_POINT ( 'NONE',  ( -14.25334919248795096, 97.91481371789856780, 6.092822981423662299 ) ) ;
#1819 = CARTESIAN_POINT ( 'NONE',  ( -50.39211230271182274, 203.5309553116391612, 1.857196546604092280 ) ) ;
#1820 = EDGE_LOOP ( 'NONE', ( #14528, #16312, #11727, #22043 ) ) ;
#1821 = DIRECTION ( 'NONE',  ( 0.000000000000000000, 0.000000000000000000, -1.000000000000000000 ) ) ;
#1822 = CARTESIAN_POINT ( 'NONE',  ( -8.715434833791929847, 124.2601862821014578, -8.962234695871762469 ) ) ;
#1823 = CARTESIAN_POINT ( 'NONE',  ( 13.23911966647218996, 62.44768628210144357, -8.632099005475504683 ) ) ;
#1824 = CARTESIAN_POINT ( 'NONE',  ( 34.09102412561951212, 5.196152422706631135, 165.2099507155409412 ) ) ;
#1825 = CARTESIAN_POINT ( 'NONE',  ( 34.06772145880400160, 5.407089921784862696, 163.5462758911768617 ) ) ;
#1826 = VECTOR ( 'NONE', #29654, 1000.000000000000114 ) ;
#1827 = CARTESIAN_POINT ( 'NONE',  ( -15.46528703574804986, 86.59768628210143504, -3.257655550457287497 ) ) ;
#1828 = CARTESIAN_POINT ( 'NONE',  ( -51.38913769728823411, 206.8500491399821044, -5.686928522499717253 ) ) ;
#1829 = CARTESIAN_POINT ( 'NONE',  ( 10.31873187879411091, -3.604726614523240613, -5.053124999385533833 ) ) ;
#1830 = CARTESIAN_POINT ( 'NONE',  ( 6.594114490232313663, 46.06018628210144072, 6.840914352312096547 ) ) ;
#1831 = EDGE_CURVE ( 'NONE', #37491, #32439, #17831, .T. ) ;
#1832 = CARTESIAN_POINT ( 'NONE',  ( 37.07307153918868181, 7.347880794884117764E-16, 164.8737688849411143 ) ) ;
#1833 = CARTESIAN_POINT ( 'NONE',  ( -62.47247103062156981, 206.6499508600178672, 5.571401726697986057 ) ) ;
#1834 = CARTESIAN_POINT ( 'NONE',  ( 30.72331255028488428, -6.928203230275514990, 161.1379710058604644 ) ) ;
#1835 = CARTESIAN_POINT ( 'NONE',  ( -12.53471296425194836, 49.22268628210144215, 2.311890736173176641 ) ) ;
#1836 = CARTESIAN_POINT ( 'NONE',  ( 27.00000000000052580, -3.464101615137444412, -7.856249998770953979 ) ) ;
#1837 = CARTESIAN_POINT ( 'NONE',  ( 27.00000000000000355, 197.6375000012290286, -3.306546357697854128E-15 ) ) ;
#1839 = CARTESIAN_POINT ( 'NONE',  ( 13.44051670066910908, 5.407089921784862696, -2.071874999385547866 ) ) ;
#1838 = CARTESIAN_POINT ( 'NONE',  ( -7.954856959092191815, 31.97268628210143149, -5.529263428287477744 ) ) ;
#1840 = CARTESIAN_POINT ( 'NONE',  ( 19.39230484541326760, 241.9924038105676800, 5.999999999999999112 ) ) ;
#1841 = ORIENTED_EDGE ( 'NONE', *, *, #12878, .F. ) ;
#1842 = CARTESIAN_POINT ( 'NONE',  ( 18.00000000000000355, -5.196152422706632912, -2.175000000000010481 ) ) ;
#1843 = CARTESIAN_POINT ( 'NONE',  ( 27.74986027194257332, -5.407089921784865361, 162.9697198055213789 ) ) ;
#1844 = CARTESIAN_POINT ( 'NONE',  ( 30.84097280299421229, -6.928203230275514990, 162.4828338482843151 ) ) ;
#1845 = CARTESIAN_POINT ( 'NONE',  ( 26.99999999999999645, 246.2125000000000057, -3.464101615137755275 ) ) ;
#1846 = DIRECTION ( 'NONE',  ( -0.5887012860850813212, 0.8083506638592999893, 0.000000000000000000 ) ) ;
#1847 = EDGE_CURVE ( 'NONE', #16024, #17042, #30597, .T. ) ;
#1848 = CARTESIAN_POINT ( 'NONE',  ( -10.69584247140429412, 90.15231371789856496, -6.932735513424201024 ) ) ;
#1849 = CARTESIAN_POINT ( 'NONE',  ( 8.715434833791931624, 92.06018628210145494, 8.962234695871760692 ) ) ;
#1850 = EDGE_LOOP ( 'NONE', ( #28320, #13238, #13654, #30388 ) ) ;
#1851 = VERTEX_POINT ( 'NONE', #11381 ) ;
#1852 = CARTESIAN_POINT ( 'NONE',  ( 13.49999999999999645, 197.2625000012290286, -23.38268590217984766 ) ) ;
#1853 = CARTESIAN_POINT ( 'NONE',  ( -13.50000000000000533, 196.7750000000000057, -23.38268590217984411 ) ) ;
#1854 = CARTESIAN_POINT ( 'NONE',  ( 11.08355503943118769, 58.23981371789854222, 10.83675517735179028 ) ) ;
#1855 = CARTESIAN_POINT ( 'NONE',  ( 23.87821517812500005, -4.985214923628404016, -9.553124999385486760 ) ) ;
#1856 = CARTESIAN_POINT ( 'NONE',  ( 23.87821517812499650, 244.7593750006145399, -4.985214923628404904 ) ) ;
#1857 = CARTESIAN_POINT ( 'NONE',  ( -55.94122103062156981, 208.9097554298617752, -4.530955311639240257 ) ) ;
#1858 = DIRECTION ( 'NONE',  ( 0.08715574274765150453, 0.000000000000000000, 0.9961946980917461003 ) ) ;
#1859 = CARTESIAN_POINT ( 'NONE',  ( 8.710071997420211432, 38.11481371789853512, -3.796722387233181895 ) ) ;
#1860 = CARTESIAN_POINT ( 'NONE',  ( 13.44051670066911264, 5.407089921784856479, -8.315624999385541116 ) ) ;
#1861 = CARTESIAN_POINT ( 'NONE',  ( -2.064181346179062349, 100.5023137178985451, -9.465287035748106703 ) ) ;
#1862 = CARTESIAN_POINT ( 'NONE',  ( 13.62178482187499640, 197.9093750006145456, -23.59362340125807123 ) ) ;
#1863 = CARTESIAN_POINT ( 'NONE',  ( 6.932735513424201024, 9.652313717898541867, -10.69584247140429412 ) ) ;
#1864 = CARTESIAN_POINT ( 'NONE',  ( -6.932735513423968321, 60.14768628210144641, -10.69584247140445221 ) ) ;
#1865 = CARTESIAN_POINT ( 'NONE',  ( 22.56230152254410015, 7.347880794884117764E-16, -8.212499998771022547 ) ) ;
#1866 =( BOUNDED_CURVE ( )  B_SPLINE_CURVE ( 2, ( #29614, #800, #33026, #3650, #4213, #18453, #15219 ),
 .UNSPECIFIED., .F., .F. ) 
 B_SPLINE_CURVE_WITH_KNOTS ( ( 3, 2, 2, 3 ),
 ( 0.08695652173913427652, 0.09420289855072766505, 0.1014492753623210397, 0.1086956521739144144 ),
 .UNSPECIFIED. ) 
 CURVE ( )  GEOMETRIC_REPRESENTATION_ITEM ( )  RATIONAL_B_SPLINE_CURVE ( ( 0.9999999999999289457, 0.8660254037845097619, 1.000000000000000000, 0.8660254037844387076, 1.000000000000000000, 0.8660254037844132835, 1.000000000000025313 ) ) 
 REPRESENTATION_ITEM ( '' )  );
#1867 = CARTESIAN_POINT ( 'NONE',  ( 18.00000000000000355, 247.3750000000000000, 5.196152422706632912 ) ) ;
#1868 = CARTESIAN_POINT ( 'NONE',  ( 33.87652354815133293, 5.407089921784857367, 161.3608737722381079 ) ) ;
#1869 = CARTESIAN_POINT ( 'NONE',  ( 37.15151170766156952, 7.347880794884117764E-16, 165.7703441132237003 ) ) ;
#1870 = CARTESIAN_POINT ( 'NONE',  ( 13.44051670066911264, -5.407089921784865361, -5.971874999385562433 ) ) ;
#1871 = CARTESIAN_POINT ( 'NONE',  ( 36.59262550718515428, 7.347880794884125653E-16, 159.3822456104860237 ) ) ;
#1872 = CARTESIAN_POINT ( 'NONE',  ( -74.35000000000002274, 210.0000000000000000, 3.000000000000000000 ) ) ;
#1873 = CARTESIAN_POINT ( 'NONE',  ( 3.474262827703335166, 92.63518628210147199, 8.843639120294326972 ) ) ;
#1874 = CYLINDRICAL_SURFACE ( 'NONE', #4361, 1.500000000000001332 ) ;
#1875 = CARTESIAN_POINT ( 'NONE',  ( -2.660918448318275509, 121.0976862821014635, 12.46528703574805874 ) ) ;
#1876 = CYLINDRICAL_SURFACE ( 'NONE', #25136, 5.999999999999994671 ) ;
#1877 = DIRECTION ( 'NONE',  ( 0.000000000000000000, 0.000000000000000000, 1.000000000000000000 ) ) ;
#1879 = ORIENTED_EDGE ( 'NONE', *, *, #30260, .F. ) ;
#1878 = AXIS2_PLACEMENT_3D ( 'NONE', #9654, #26702, #23684 ) ;
#1880 = CARTESIAN_POINT ( 'NONE',  ( 37.17272443640960233, -3.604726614523235284, 163.2181584645603323 ) ) ;
#1881 = CARTESIAN_POINT ( 'NONE',  ( 23.87821517812499650, 4.985214923628404904, -5.240624999385462779 ) ) ;
#1882 = CARTESIAN_POINT ( 'NONE',  ( 27.24356964375000345, 197.3843750006145399, -3.336375036156643733E-15 ) ) ;
#1883 = LINE ( 'NONE', #4026, #2516 ) ;
#1884 = CARTESIAN_POINT ( 'NONE',  ( 37.33453876732453125, -3.464101615137755275, 167.8623529779920034 ) ) ;
#1885 = DIRECTION ( 'NONE',  ( -0.000000000000000000, -0.000000000000000000, 1.000000000000000000 ) ) ;
#1886 = CARTESIAN_POINT ( 'NONE',  ( 21.00000000000000000, 243.4468750006145683, -6.646953231504538984 ) ) ;
#1887 = CARTESIAN_POINT ( 'NONE',  ( 29.49323130461320730, 6.148716367659644355, 159.5176625013623095 ) ) ;
#1888 = CARTESIAN_POINT ( 'NONE',  ( -4.622313124798826500, 142.7648137178985621, 11.61527771782809637 ) ) ;
#1889 = CARTESIAN_POINT ( 'NONE',  ( 8.715434833791931624, 138.0601862821014549, 8.962234695871760692 ) ) ;
#1891 = ORIENTED_EDGE ( 'NONE', *, *, #7343, .F. ) ;
#1890 = ORIENTED_EDGE ( 'NONE', *, *, #32981, .F. ) ;
#1892 = CARTESIAN_POINT ( 'NONE',  ( 26.75643035624999655, 245.4718750006145171, -7.049594010296217766E-16 ) ) ;
#1893 = DIRECTION ( 'NONE',  ( 1.000000000000000000, 0.000000000000000000, 0.000000000000000000 ) ) ;
#1894 = CARTESIAN_POINT ( 'NONE',  ( 15.24356964374999990, 3.323476615752268604, -2.878124999385485161 ) ) ;
#1895 = CARTESIAN_POINT ( 'NONE',  ( 15.46528703574811736, 121.2023137178985479, -3.257655550456947768 ) ) ;
#1896 = CARTESIAN_POINT ( 'NONE',  ( 26.99999999999999645, 244.3750000000000000, -7.347880794884117764E-16 ) ) ;
#1897 = CARTESIAN_POINT ( 'NONE',  ( 24.00000000000000000, -5.196152422706629359, -10.14374999877096251 ) ) ;
#1898 = EDGE_CURVE ( 'NONE', #29577, #4196, #33243, .T. ) ;
#1899 = CARTESIAN_POINT ( 'NONE',  ( 22.80587116629412492, -3.604726614523238837, -7.659374999385499372 ) ) ;
#1900 = ORIENTED_EDGE ( 'NONE', *, *, #29749, .F. ) ;
#1901 = CARTESIAN_POINT ( 'NONE',  ( -13.49999999999998401, 198.3875000012290286, 23.38268590217985476 ) ) ;
#1902 = CARTESIAN_POINT ( 'NONE',  ( 12.50000000000000355, 118.5101862821014578, 0.1745138560725507937 ) ) ;
#1903 = DIRECTION ( 'NONE',  ( -0.9933043639548644332, 0.1155267958017622554, 0.000000000000000000 ) ) ;
#1904 = CARTESIAN_POINT ( 'NONE',  ( -40.29836230271183695, 202.5810206699313767, -4.149950860017804111 ) ) ;
#1905 = CARTESIAN_POINT ( 'NONE',  ( 23.87821517812499650, 243.7468750006145228, -4.985214923628404904 ) ) ;
#1906 = DIRECTION ( 'NONE',  ( 1.000000000000000000, 0.000000000000000000, 0.000000000000000000 ) ) ;
#1907 = CARTESIAN_POINT ( 'NONE',  ( -33.76711230271183695, 214.4690446883608104, -1.321298161741814914 ) ) ;
#1909 = EDGE_CURVE ( 'NONE', #28735, #6593, #13629, .T. ) ;
#1908 = CARTESIAN_POINT ( 'NONE',  ( 2.660918448318279950, 134.8976862821014890, -12.46528703574805697 ) ) ;
#1910 = CARTESIAN_POINT ( 'NONE',  ( 16.56230152254411436, 6.928203230275506996, -0.4499999987709982219 ) ) ;
#1911 = ORIENTED_EDGE ( 'NONE', *, *, #28122, .F. ) ;
#1912 = CARTESIAN_POINT ( 'NONE',  ( 20.99999999999999289, 245.4437500012290343, -5.999999999999997335 ) ) ;
#1913 = CARTESIAN_POINT ( 'NONE',  ( 10.83675517735155225, 119.6601862821014635, 11.08355503943142573 ) ) ;
#1914 = UNCERTAINTY_MEASURE_WITH_UNIT (LENGTH_MEASURE( 1.000000000000000082E-05 ), #7486, 'distance_accuracy_value', 'NONE');
#1915 = DIRECTION ( 'NONE',  ( 0.000000000000000000, 1.000000000000000000, 0.000000000000000000 ) ) ;
#1916 = CARTESIAN_POINT ( 'NONE',  ( -8.715434833791929847, 4.660186282101435928, -8.962234695871762469 ) ) ;
#1917 = CARTESIAN_POINT ( 'NONE',  ( 22.56230152254412147, -3.464101615137755275, -9.712500000000016342 ) ) ;
#1918 = ORIENTED_EDGE ( 'NONE', *, *, #4718, .F. ) ;
#1919 = DIRECTION ( 'NONE',  ( -0.000000000000000000, -0.000000000000000000, -1.000000000000000000 ) ) ;
#1920 = CARTESIAN_POINT ( 'NONE',  ( 1.715153634034233487, 74.52268628210144641, 9.534712964251941258 ) ) ;
#1921 =( NAMED_UNIT ( * ) SI_UNIT ( $, .STERADIAN. ) SOLID_ANGLE_UNIT ( ) );
#1922 = CARTESIAN_POINT ( 'NONE',  ( -5.233372021372612259, 124.6523137178985650, 8.152565276336593669 ) ) ;
#1923 = CARTESIAN_POINT ( 'NONE',  ( 27.24356964375000700, 195.4906250006145001, 15.72908226750537075 ) ) ;
#1924 = CYLINDRICAL_SURFACE ( 'NONE', #15961, 5.999999999999998224 ) ;
#1925 = CARTESIAN_POINT ( 'NONE',  ( 27.24356964375000345, 199.1843750006145228, -3.336375036156643733E-15 ) ) ;
#1926 = CARTESIAN_POINT ( 'NONE',  ( -29.00000000000002487, 210.0000000000000000, 0.000000000000000000 ) ) ;
#1927 = CARTESIAN_POINT ( 'NONE',  ( 26.99999999999999645, 242.0875000000000057, 3.464101615137751278 ) ) ;
#1928 = CARTESIAN_POINT ( 'NONE',  ( -6.594114490232462877, 60.53981371789856070, 6.840914352311949109 ) ) ;
#1929 = CARTESIAN_POINT ( 'NONE',  ( 34.14658591151403755, -5.196152422706635576, 165.8450248343500562 ) ) ;
#1930 = ORIENTED_EDGE ( 'NONE', *, *, #21548, .F. ) ;
#1931 = VECTOR ( 'NONE', #2756, 1000.000000000000000 ) ;
#1932 = CARTESIAN_POINT ( 'NONE',  ( 18.00000000000000355, 242.4812500012290570, 5.196152422706632912 ) ) ;
#1933 = CARTESIAN_POINT ( 'NONE',  ( -8.715434833792127023, 60.53981371789856070, 8.962234695871568846 ) ) ;
#1934 = CARTESIAN_POINT ( 'NONE',  ( 19.68408634441911431, -5.407089921784861808, -6.346874999385549110 ) ) ;
#1935 = CARTESIAN_POINT ( 'NONE',  ( 27.24356964374999635, 198.2656250006145058, -15.72908226750539029 ) ) ;
#1936 = CARTESIAN_POINT ( 'NONE',  ( 26.75643035624999655, -3.323476615752267715, -7.715624999385478411 ) ) ;
#1937 = CARTESIAN_POINT ( 'NONE',  ( -0.1745138560722763466, 36.38981371789855501, -12.50000000000000355 ) ) ;
#1938 = ORIENTED_EDGE ( 'NONE', *, *, #7640, .T. ) ;
#1939 = CARTESIAN_POINT ( 'NONE',  ( 19.68408634441911431, -5.407089921784861808, -0.4968749993855270386 ) ) ;
#1940 = CARTESIAN_POINT ( 'NONE',  ( -11.48171059495397373, 4.085186282101443744, -4.944772684328680334 ) ) ;
#1941 = CARTESIAN_POINT ( 'NONE',  ( 34.52528910822917396, -5.407089921784861808, 168.7762980561585380 ) ) ;
#1942 = CARTESIAN_POINT ( 'NONE',  ( -55.34002896937850124, 204.4285982733020433, 3.350049139982171020 ) ) ;
#1943 = PRODUCT_CONTEXT ( 'NONE', #19027, 'mechanical' ) ;
#1944 = CARTESIAN_POINT ( 'NONE',  ( -3.253724281355068545E-15, 197.3000000012290229, -27.00000000000000355 ) ) ;
#1945 = CARTESIAN_POINT ( 'NONE',  ( -11.61527771782809282, 62.26481371789854791, -4.622313124798832717 ) ) ;
#1946 = CARTESIAN_POINT ( 'NONE',  ( -65.63169563604516554, 210.1155267958017703, 4.499999999999996447 ) ) ;
#1948 = EDGE_CURVE ( 'NONE', #16763, #28735, #10973, .T. ) ;
#1947 = CARTESIAN_POINT ( 'NONE',  ( -53.96205436395489130, 214.6737587650352168, 4.842901733360204908 ) ) ;
#1949 = CARTESIAN_POINT ( 'NONE',  ( 20.99999999999999645, 6.928203230275506996, -6.862499999999990941 ) ) ;
#1950 = CARTESIAN_POINT ( 'NONE',  ( 15.00000000000000000, 0.000000000000000000, -3.093749998770961795 ) ) ;
#1951 = CARTESIAN_POINT ( 'NONE',  ( 15.46528703574811736, 47.60231371789853938, -3.257655550456947768 ) ) ;
#1952 = CARTESIAN_POINT ( 'NONE',  ( -39.11086230271183695, 214.1499508600178387, -7.418979330068641964 ) ) ;
#1953 = CARTESIAN_POINT ( 'NONE',  ( 8.962234695871762469, 25.36018628210144499, -8.715434833791931624 ) ) ;
#1954 =( BOUNDED_CURVE ( )  B_SPLINE_CURVE ( 2, ( #28163, #8083, #30649, #25506, #1824, #24944, #13393 ),
 .UNSPECIFIED., .F., .F. ) 
 B_SPLINE_CURVE_WITH_KNOTS ( ( 3, 2, 2, 3 ),
 ( 0.3478260869565212854, 0.3550724637681154094, 0.3623188405797094780, 0.3695652173913035465 ),
 .UNSPECIFIED. ) 
 CURVE ( )  GEOMETRIC_REPRESENTATION_ITEM ( )  RATIONAL_B_SPLINE_CURVE ( ( 1.000000000000008216, 0.8660254037844304920, 1.000000000000000000, 0.8660254037844387076, 1.000000000000000000, 0.8660254037844530295, 0.9999999999999856781 ) ) 
 REPRESENTATION_ITEM ( '' )  );
#1955 = LINE ( 'NONE', #28988, #36989 ) ;
#1956 = CARTESIAN_POINT ( 'NONE',  ( -10.49813415415989581, 59.57268628210145778, -7.228626920339068285 ) ) ;
#1957 = CARTESIAN_POINT ( 'NONE',  ( 15.46528703574804986, 17.59768628210143504, 3.257655550457285720 ) ) ;
#1958 = CARTESIAN_POINT ( 'NONE',  ( 13.56230152254410726, 5.196152422706636465, -1.875000000000043299 ) ) ;
#1959 = CARTESIAN_POINT ( 'NONE',  ( 20.99999999999997868, 246.9625000000000057, 5.999999999999999112 ) ) ;
#1960 = ORIENTED_EDGE ( 'NONE', *, *, #2267, .F. ) ;
#1961 = CARTESIAN_POINT ( 'NONE',  ( -8.927990412390661490, 29.67268628210143788, 13.04141134922759804 ) ) ;
#1962 = CARTESIAN_POINT ( 'NONE',  ( -13.50000000000000533, 195.9875000012290229, -23.38268590217984411 ) ) ;
#1963 = CARTESIAN_POINT ( 'NONE',  ( 27.24356964374999635, 197.8718750006145513, -15.72908226750539029 ) ) ;
#1964 = CARTESIAN_POINT ( 'NONE',  ( -29.50000000000000711, 237.0000000000000000, -2.499999999999994671 ) ) ;
#1965 = CYLINDRICAL_SURFACE ( 'NONE', #29291, 2.649999999999992806 ) ;
#1966 = CARTESIAN_POINT ( 'NONE',  ( -44.35000000000001563, 244.5000000000000000, -2.499999999999998224 ) ) ;
#1967 = CARTESIAN_POINT ( 'NONE',  ( 37.07307153918868181, 7.347880794884117764E-16, 164.8737688849411143 ) ) ;
#1968 = CARTESIAN_POINT ( 'NONE',  ( 23.87821517812499650, 246.5593750006145228, -4.985214923628404904 ) ) ;
#1969 = CARTESIAN_POINT ( 'NONE',  ( 9.500000000000005329, 103.0898137178985792, -0.1745138560723090149 ) ) ;
#1970 = CARTESIAN_POINT ( 'NONE',  ( 15.24356964375000167, 243.5968750006144887, 3.323476615752272600 ) ) ;
#1971 = ORIENTED_EDGE ( 'NONE', *, *, #25981, .F. ) ;
#1972 = CARTESIAN_POINT ( 'NONE',  ( 22.56230152254492438, -3.464101615137295642, -7.012500000000033040 ) ) ;
#1973 = EDGE_CURVE ( 'NONE', #30190, #35202, #32023, .T. ) ;
#1974 = CARTESIAN_POINT ( 'NONE',  ( 18.00000000000000355, 248.7812500012290400, 5.196152422706632912 ) ) ;
#1975 = CARTESIAN_POINT ( 'NONE',  ( -2.311890736173447980, 114.8773137178985735, 12.53471296425189330 ) ) ;
#1976 = CARTESIAN_POINT ( 'NONE',  ( 13.44051670066911619, -5.407089921784859143, -9.515624999385547511 ) ) ;
#1977 = CARTESIAN_POINT ( 'NONE',  ( 37.01584409946383403, -3.604726614523235284, 161.4250080079952170 ) ) ;
#1978 = CARTESIAN_POINT ( 'NONE',  ( 24.93570810221097034, -3.464101615138005741, 163.8276289306958233 ) ) ;
#1979 = CARTESIAN_POINT ( 'NONE',  ( 13.49999999999999645, 197.5999999999999943, -23.38268590217984766 ) ) ;
#1980 = AXIS2_PLACEMENT_3D ( 'NONE', #7089, #18659, #4225 ) ;
#1981 = ORIENTED_EDGE ( 'NONE', *, *, #16185, .F. ) ;
#1982 = CARTESIAN_POINT ( 'NONE',  ( 12.46528703574805874, 26.79768628210144144, 2.660918448318279950 ) ) ;
#1983 = ORIENTED_EDGE ( 'NONE', *, *, #32619, .F. ) ;
#1984 = VERTEX_POINT ( 'NONE', #17641 ) ;
#1985 = CARTESIAN_POINT ( 'NONE',  ( 23.99999999999999645, 5.196152422706631135, -4.143749998770957177 ) ) ;
#1986 = DIRECTION ( 'NONE',  ( 0.000000000000000000, 0.000000000000000000, 1.000000000000000000 ) ) ;
#1987 = CYLINDRICAL_SURFACE ( 'NONE', #10033, 27.00000000000000000 ) ;
#1988 = CYLINDRICAL_SURFACE ( 'NONE', #26802, 6.000000000000001776 ) ;
#1989 = CARTESIAN_POINT ( 'NONE',  ( 15.24356964374999990, 248.8468750006145171, 0.000000000000000000 ) ) ;
#1990 = CARTESIAN_POINT ( 'NONE',  ( 11.48171059495397728, 63.88518628210145067, 4.944772684328674117 ) ) ;
#1991 = CARTESIAN_POINT ( 'NONE',  ( 6.092822981423978490, 135.1851862821014549, -14.25334919248782306 ) ) ;
#1992 = CARTESIAN_POINT ( 'NONE',  ( -57.51711230271182984, 216.4690446883607535, -1.857196546604089393 ) ) ;
#1993 = CARTESIAN_POINT ( 'NONE',  ( 15.20136072254650372, 225.4630380732105550, -1.553813268098525935 ) ) ;
#1994 = CARTESIAN_POINT ( 'NONE',  ( -55.53794563604517975, 206.7903428501025758, 3.378800118222471838 ) ) ;
#1995 = CARTESIAN_POINT ( 'NONE',  ( 20.99999999999999645, 185.0294372515228645, 5.999999999999999112 ) ) ;
#1996 = CARTESIAN_POINT ( 'NONE',  ( 24.93897644267070035, 3.464101615137752166, 163.8649862330987048 ) ) ;
#1997 = CARTESIAN_POINT ( 'NONE',  ( 2.311890736173452865, 128.6773137178985564, -12.53471296425189152 ) ) ;
#1998 = CARTESIAN_POINT ( 'NONE',  ( -66.82663769728823411, 206.0451222850691408, 2.149950860017832532 ) ) ;
#1999 = CLOSED_SHELL ( 'NONE', ( #16368, #12231, #10763, #12020, #10658, #28577 ) ) ;
#2000 = CARTESIAN_POINT ( 'NONE',  ( -58.51413769728822700, 214.1499508600179240, 7.418979330068584233 ) ) ;
#2001 = CARTESIAN_POINT ( 'NONE',  ( 20.99999999999999645, -6.646953231504538984, -2.840624999385488181 ) ) ;
#2002 = CARTESIAN_POINT ( 'NONE',  ( -1.926257025242585782E-15, 196.9906250006145569, -31.45816453501075927 ) ) ;
#2003 = CARTESIAN_POINT ( 'NONE',  ( -13.04141134922778456, 88.42731371789855643, 8.927990412390377273 ) ) ;
#2004 = CARTESIAN_POINT ( 'NONE',  ( -38.31919563604516554, 216.5000000000000000, -0.1155267958017906493 ) ) ;
#2005 = EDGE_LOOP ( 'NONE', ( #16646, #26117 ) ) ;
#2006 = DIRECTION ( 'NONE',  ( -1.000000000000000000, -6.123233995736766036E-17, 0.000000000000000000 ) ) ;
#2007 = CARTESIAN_POINT ( 'NONE',  ( 2.660918448318279950, 116.4976862821014549, -12.46528703574805697 ) ) ;
#2008 = CARTESIAN_POINT ( 'NONE',  ( 10.83675517735155225, 73.66018628210144925, 11.08355503943142573 ) ) ;
#2009 = DIRECTION ( 'NONE',  ( 0.000000000000000000, 0.000000000000000000, 1.000000000000000000 ) ) ;
#2010 = CARTESIAN_POINT ( 'NONE',  ( 24.86547026816695904, 3.604726614523240613, 165.8194550616826461 ) ) ;
#2011 = CARTESIAN_POINT ( 'NONE',  ( -15.50000000000000533, 86.31018628210145494, -0.1745138560725808530 ) ) ;
#2012 = AXIS2_PLACEMENT_3D ( 'NONE', #21693, #33244, #1205 ) ;
#2013 = CARTESIAN_POINT ( 'NONE',  ( -54.75372103062155560, 216.5309553116392181, -1.626142955000564383 ) ) ;
#2014 = CARTESIAN_POINT ( 'NONE',  ( 22.80587116629410360, 7.646167579472015790E-16, -7.115624999385533833 ) ) ;
#2015 = CARTESIAN_POINT ( 'NONE',  ( 3.796722387233379514, 24.78518628210144215, -8.710071997420127943 ) ) ;
#2016 = CARTESIAN_POINT ( 'NONE',  ( -58.71205436395488420, 214.6737587650352168, 4.842901733360204908 ) ) ;
#2017 = CARTESIAN_POINT ( 'NONE',  ( -44.35000000000001563, 244.5000000000000000, 2.500000000000002220 ) ) ;
#2018 = CARTESIAN_POINT ( 'NONE',  ( 11.48171059495397728, 63.88518628210145067, 4.944772684328674117 ) ) ;
#2019 = CARTESIAN_POINT ( 'NONE',  ( 13.50000000000001421, 198.3499999999999943, 23.38268590217984055 ) ) ;
#2020 = CARTESIAN_POINT ( 'NONE',  ( 10.56230152254410548, 0.000000000000000000, -6.750000000000061284 ) ) ;
#2022 = CARTESIAN_POINT ( 'NONE',  ( 22.80587116629411426, 7.646167579472024665E-16, -1.771874999385525395 ) ) ;
#2021 = CARTESIAN_POINT ( 'NONE',  ( 0.1745138560725194299, 24.21018628210144996, -9.500000000000005329 ) ) ;
#2023 = CARTESIAN_POINT ( 'NONE',  ( 27.00000000000001421, 198.5000000012290684, 15.58845726811988897 ) ) ;
#2024 = ORIENTED_EDGE ( 'NONE', *, *, #23373, .F. ) ;
#2025 = CARTESIAN_POINT ( 'NONE',  ( 15.00000000000000000, 3.464101615137752166, -2.287500000000007638 ) ) ;
#2026 =( BOUNDED_CURVE ( )  B_SPLINE_CURVE ( 2, ( #36868, #8629, #22677, #14501, #31560, #34036, #13771, #7894, #14135 ),
 .UNSPECIFIED., .F., .F. ) 
 B_SPLINE_CURVE_WITH_KNOTS ( ( 3, 2, 2, 2, 3 ),
 ( 0.05434782608695652717, 0.05797101449275362389, 0.06521739130434782428, 0.07246376811594203160, 0.07608695652173913526 ),
 .UNSPECIFIED. ) 
 CURVE ( )  GEOMETRIC_REPRESENTATION_ITEM ( )  RATIONAL_B_SPLINE_CURVE ( ( 0.9330127018922194093, 0.9330127018922194093, 1.000000000000000000, 0.8660254037844387076, 1.000000000000000000, 0.8660254037844387076, 1.000000000000000000, 0.9330127018922191873, 0.9330127018922192983 ) ) 
 REPRESENTATION_ITEM ( '' )  );
#2027 = CARTESIAN_POINT ( 'NONE',  ( -74.35000000000002274, 210.0000000000000000, 5.000000000000000000 ) ) ;
#2028 = CARTESIAN_POINT ( 'NONE',  ( 33.87162103762178589, 5.407089921784862696, 161.3048378204704534 ) ) ;
#2029 = CARTESIAN_POINT ( 'NONE',  ( 19.68408634441910365, -5.407089921784855591, -0.8906249993855530622 ) ) ;
#2030 = CARTESIAN_POINT ( 'NONE',  ( 33.83282523762249383, -5.196152422706635576, 162.2587239212197971 ) ) ;
#2031 = CARTESIAN_POINT ( 'NONE',  ( 24.00000000000000000, 242.5000000000000000, 5.196152422706629359 ) ) ;
#2032 = DIRECTION ( 'NONE',  ( 0.000000000000000000, 0.000000000000000000, -1.000000000000000000 ) ) ;
#2033 = CARTESIAN_POINT ( 'NONE',  ( -2.660918448318004614, 82.10231371789855359, -12.46528703574811558 ) ) ;
#2034 = CARTESIAN_POINT ( 'NONE',  ( 6.932735513423970097, 83.14768628210144641, 10.69584247140445044 ) ) ;
#2035 = ORIENTED_EDGE ( 'NONE', *, *, #13992, .T. ) ;
#2036 = ORIENTED_EDGE ( 'NONE', *, *, #21240, .F. ) ;
#2037 = CARTESIAN_POINT ( 'NONE',  ( 27.00000000000000355, 197.1875000012290400, -3.306546357697854128E-15 ) ) ;
#2038 = CARTESIAN_POINT ( 'NONE',  ( 26.99999999999999645, 7.347880794884117764E-16, -1.124999999999987121 ) ) ;
#2039 = CARTESIAN_POINT ( 'NONE',  ( 14.38691631536194393, 57.66481371789855359, 5.770363421894124656 ) ) ;
#2040 = CARTESIAN_POINT ( 'NONE',  ( 21.00000000000000000, 6.646953231504538984, -9.815624999385470062 ) ) ;
#2041 = CARTESIAN_POINT ( 'NONE',  ( 15.24356964374999990, 243.1093750006145342, 0.000000000000000000 ) ) ;
#2042 = AXIS2_PLACEMENT_3D ( 'NONE', #31159, #28304, #16756 ) ;
#2043 = CARTESIAN_POINT ( 'NONE',  ( -55.54538769728824832, 211.3212981617418222, -4.469044688360751749 ) ) ;
#2044 = CARTESIAN_POINT ( 'NONE',  ( 1.255007937094097924E-14, 199.4375000000000284, -27.00000000000000000 ) ) ;
#2045 = CARTESIAN_POINT ( 'NONE',  ( 6.840914352311949109, 39.83981371789855075, 6.594114490232462877 ) ) ;
#2046 = CARTESIAN_POINT ( 'NONE',  ( 16.56230152254411436, -7.209453229046475009, -9.928124999385525840 ) ) ;
#2047 = CARTESIAN_POINT ( 'NONE',  ( 8.843639120294245259, 94.46481371789855075, 3.474262827703527901 ) ) ;
#2048 = CARTESIAN_POINT ( 'NONE',  ( -1.926257025242585782E-15, 198.3968750006145285, -31.45816453501075927 ) ) ;
#2049 = CARTESIAN_POINT ( 'NONE',  ( -10.49813415416004858, 14.82731371789855501, 7.228626920338839135 ) ) ;
#2050 =( GEOMETRIC_REPRESENTATION_CONTEXT ( 3 ) GLOBAL_UNCERTAINTY_ASSIGNED_CONTEXT ( ( #9714 ) ) GLOBAL_UNIT_ASSIGNED_CONTEXT ( ( #28, #2687, #34711 ) ) REPRESENTATION_CONTEXT ( 'NONE', 'WORKASPACE' ) );
#2051 = ADVANCED_FACE ( 'NONE', ( #370, #18586 ), #32779, .F. ) ;
#2052 = CARTESIAN_POINT ( 'NONE',  ( -12.53471296425194836, 58.42268628210145209, 2.311890736173176641 ) ) ;
#2053 = CARTESIAN_POINT ( 'NONE',  ( 22.56230152254409660, 3.464101615137755275, -9.524999998771003007 ) ) ;
#2054 = EDGE_CURVE ( 'NONE', #32985, #22802, #12313, .T. ) ;
#2055 = CARTESIAN_POINT ( 'NONE',  ( 2.999999999999997335, 244.5000000000000000, -10.00000000000000000 ) ) ;
#2056 = CARTESIAN_POINT ( 'NONE',  ( 24.55988044515800439, 0.000000000000000000, 162.3265474014984591 ) ) ;
#2057 = CARTESIAN_POINT ( 'NONE',  ( 10.31873187879411091, 3.604726614523240613, -9.684374999385527261 ) ) ;
#2058 = CARTESIAN_POINT ( 'NONE',  ( 22.80587116629411781, -3.604726614523238837, -7.209374999385536498 ) ) ;
#2059 = CARTESIAN_POINT ( 'NONE',  ( 36.86389775648778055, -3.464101615137418211, 162.4829016082964870 ) ) ;
#2060 = CARTESIAN_POINT ( 'NONE',  ( 27.72819177541068214, 5.196152422706630247, 161.3247236329709153 ) ) ;
#2061 = CARTESIAN_POINT ( 'NONE',  ( -9.465287035748065847, 86.59768628210143504, -2.064181346179273735 ) ) ;
#2062 = DIRECTION ( 'NONE',  ( 0.9961946980917462113, 0.000000000000000000, -0.08715574274765118534 ) ) ;
#2063 = ADVANCED_FACE ( 'NONE', ( #24072 ), #6442, .T. ) ;
#2064 = CARTESIAN_POINT ( 'NONE',  ( -11.48171059495397373, 114.4851862821014521, -4.944772684328680334 ) ) ;
#2065 = CARTESIAN_POINT ( 'NONE',  ( -26.99999999999999645, 197.3375000000000057, 15.58845726811991561 ) ) ;
#2066 = CARTESIAN_POINT ( 'NONE',  ( 22.60769515458673240, 248.3888461906613543, 6.000000000000000000 ) ) ;
#2067 = ORIENTED_EDGE ( 'NONE', *, *, #6952, .T. ) ;
#2068 = CARTESIAN_POINT ( 'NONE',  ( 31.04442699002431993, 7.209453229046475009, 164.8083258472544230 ) ) ;
#2069 = CARTESIAN_POINT ( 'NONE',  ( 15.24356964375000167, -3.323476615752272600, -4.603124999385474148 ) ) ;
#2070 = CARTESIAN_POINT ( 'NONE',  ( -13.62178482187498396, 198.5843750006145569, 23.59362340125808188 ) ) ;
#2071 = CARTESIAN_POINT ( 'NONE',  ( 34.52528910822917396, -5.407089921784861808, 168.7762980561585380 ) ) ;
#2072 =( BOUNDED_CURVE ( )  B_SPLINE_CURVE ( 2, ( #2525, #25644, #36454, #34361, #8407, #24903, #1962, #36644, #3266 ),
 .UNSPECIFIED., .F., .F. ) 
 B_SPLINE_CURVE_WITH_KNOTS ( ( 3, 2, 2, 2, 3 ),
 ( 0.6458333333333333703, 0.6527777777777777901, 0.6666666666666666297, 0.6805555555555555802, 0.6875000000000000000 ),
 .UNSPECIFIED. ) 
 CURVE ( )  GEOMETRIC_REPRESENTATION_ITEM ( )  RATIONAL_B_SPLINE_CURVE ( ( 0.9330127018922192983, 0.9330127018922198534, 1.000000000000000000, 0.8660254037844387076, 1.000000000000000000, 0.8660254037844387076, 1.000000000000000000, 0.9330127018922194093, 0.9330127018922194093 ) ) 
 REPRESENTATION_ITEM ( '' )  );
#2073 = CARTESIAN_POINT ( 'NONE',  ( 28.43742163191258499, -5.196152422706638241, 169.4312579874681148 ) ) ;
#2074 = CARTESIAN_POINT ( 'NONE',  ( 10.56230152254410903, 0.000000000000000000, -2.250000000000057732 ) ) ;
#2075 = CARTESIAN_POINT ( 'NONE',  ( 26.99999999999999645, 249.7750000000000057, -7.347880794884117764E-16 ) ) ;
#2076 = DIRECTION ( 'NONE',  ( 1.000000000000000000, 0.000000000000000000, 0.000000000000000000 ) ) ;
#2077 = CARTESIAN_POINT ( 'NONE',  ( -0.1745138560723084320, 8.789813717898553591, -9.500000000000005329 ) ) ;
#2078 = CARTESIAN_POINT ( 'NONE',  ( 5.778771075727756162E-15, 195.4718750006145171, 31.45816453501076637 ) ) ;
#2080 = ORIENTED_EDGE ( 'NONE', *, *, #22684, .F. ) ;
#2079 = VERTEX_POINT ( 'NONE', #21052 ) ;
#2081 = CARTESIAN_POINT ( 'NONE',  ( 26.99999999999999645, 196.7750000012290172, -15.58845726811990495 ) ) ;
#2082 = CARTESIAN_POINT ( 'NONE',  ( 21.00000000000000000, 245.3593750006145342, 6.646953231504538984 ) ) ;
#2083 = CYLINDRICAL_SURFACE ( 'NONE', #16524, 5.999999999999998224 ) ;
#2084 = AXIS2_PLACEMENT_3D ( 'NONE', #26295, #17974, #2991 ) ;
#2085 = CARTESIAN_POINT ( 'NONE',  ( 18.12178482187499640, 4.985214923628404904, -3.365624999385474769 ) ) ;
#2086 = CARTESIAN_POINT ( 'NONE',  ( 15.53471296425188797, 121.7773137178985650, 2.908627838312457747 ) ) ;
#2087 = CARTESIAN_POINT ( 'NONE',  ( 20.99999999999999645, 244.2624999999999602, 5.999999999999998224 ) ) ;
#2088 = CARTESIAN_POINT ( 'NONE',  ( 26.75643035624999655, -3.323476615752267715, -1.865624999385470772 ) ) ;
#2089 = CARTESIAN_POINT ( 'NONE',  ( 22.80587116629411781, -3.604726614523238837, -8.109374999385527971 ) ) ;
#2090 = EDGE_LOOP ( 'NONE', ( #4509, #18606, #4185, #1735 ) ) ;
#2091 = CARTESIAN_POINT ( 'NONE',  ( 26.99999999999999645, 199.0250000012290457, -15.58845726811990495 ) ) ;
#2092 = CARTESIAN_POINT ( 'NONE',  ( 7.228626920339068285, 107.8726862821014549, -10.49813415415989581 ) ) ;
#2093 =( BOUNDED_CURVE ( )  B_SPLINE_CURVE ( 2, ( #2964, #14532, #17944, #15093, #20983, #26642, #12807 ),
 .UNSPECIFIED., .F., .F. ) 
 B_SPLINE_CURVE_WITH_KNOTS ( ( 3, 2, 2, 3 ),
 ( 0.7608695652173899093, 0.7681159420289841444, 0.7753623188405783795, 0.7826086956521727256 ),
 .UNSPECIFIED. ) 
 CURVE ( )  GEOMETRIC_REPRESENTATION_ITEM ( )  RATIONAL_B_SPLINE_CURVE ( ( 1.000000000000026645, 0.8660254037844120623, 1.000000000000000000, 0.8660254037844387076, 1.000000000000000000, 0.8660254037844612451, 0.9999999999999774625 ) ) 
 REPRESENTATION_ITEM ( '' )  );
#2094 = CARTESIAN_POINT ( 'NONE',  ( -40.49627896937850835, 201.4690446883607251, -2.162041339862721845 ) ) ;
#2095 = CARTESIAN_POINT ( 'NONE',  ( 15.24356964374999990, 244.3093750006144944, -3.323476615752268604 ) ) ;
#2096 = CARTESIAN_POINT ( 'NONE',  ( -4.694659320240884604E-14, 197.5250000012290172, 27.00000000000000000 ) ) ;
#2097 = CARTESIAN_POINT ( 'NONE',  ( -64.64211230271182274, 203.5309553116391612, 1.857196546604092280 ) ) ;
#2098 = CARTESIAN_POINT ( 'NONE',  ( -7.228626920339069173, 121.6726862821014521, 10.49813415415989581 ) ) ;
#2099 = CARTESIAN_POINT ( 'NONE',  ( 13.56230152254410548, 5.196152422706630247, -1.312499998771005094 ) ) ;
#2100 = CARTESIAN_POINT ( 'NONE',  ( -37.73288769728821279, 203.5309553116391612, -1.857196546604028775 ) ) ;
#2101 = CARTESIAN_POINT ( 'NONE',  ( 21.00000000000000355, 0.000000000000000000, 50.00000000000001421 ) ) ;
#2102 = CARTESIAN_POINT ( 'NONE',  ( 16.56230152254411081, -6.928203230275514990, -8.887500000000020606 ) ) ;
#2103 = CARTESIAN_POINT ( 'NONE',  ( -8.632099005475501130, 115.3476862821014493, -13.23911966647218996 ) ) ;
#2104 = CARTESIAN_POINT ( 'NONE',  ( 0.000000000000000000, 150.0000000000000000, 0.000000000000000000 ) ) ;
#2105 = CARTESIAN_POINT ( 'NONE',  ( 10.49813415415989581, 8.972686282101431487, 7.228626920339068285 ) ) ;
#2106 = CARTESIAN_POINT ( 'NONE',  ( 13.56230152254410548, 5.196152422706636465, -9.975000000000012079 ) ) ;
#2107 = VERTEX_POINT ( 'NONE', #23887 ) ;
#2108 = CYLINDRICAL_SURFACE ( 'NONE', #17316, 5.999999999999994671 ) ;
#2109 = CARTESIAN_POINT ( 'NONE',  ( -8.843639120294326972, 85.73518628210145209, 3.474262827703335166 ) ) ;
#2110 = CYLINDRICAL_SURFACE ( 'NONE', #30301, 5.999999999999999112 ) ;
#2111 = CARTESIAN_POINT ( 'NONE',  ( 13.62178482187501416, 195.0031250006145456, 23.59362340125806767 ) ) ;
#2112 = CARTESIAN_POINT ( 'NONE',  ( 18.00000000000000355, 246.9812500012290570, 5.196152422706632912 ) ) ;
#2113 = CARTESIAN_POINT ( 'NONE',  ( -27.24356964374999635, 197.1968750006145115, 15.72908226750539384 ) ) ;
#2114 = CARTESIAN_POINT ( 'NONE',  ( 26.99999999999999645, 7.347880794884117764E-16, -1.518749998770940746 ) ) ;
#2115 = CARTESIAN_POINT ( 'NONE',  ( 21.00000000000000000, 242.0124999999999886, 5.999999999999998224 ) ) ;
#2116 = CARTESIAN_POINT ( 'NONE',  ( -8.710071997420207879, 51.91481371789856070, 3.796722387233182339 ) ) ;
#2117 = CARTESIAN_POINT ( 'NONE',  ( 24.00000000000000000, -5.196152422706629359, -8.399999999999991473 ) ) ;
#2118 = VERTEX_POINT ( 'NONE', #15541 ) ;
#2119 = CARTESIAN_POINT ( 'NONE',  ( 26.99999999999999645, 242.2187500012290684, -3.464101615137755275 ) ) ;
#2120 = CARTESIAN_POINT ( 'NONE',  ( 11.48171059495408208, 56.51481371789855501, -4.944772684328420986 ) ) ;
#2121 = CARTESIAN_POINT ( 'NONE',  ( 16.56230152254411436, 7.209453229046482114, -5.259374999385500793 ) ) ;
#2122 = CARTESIAN_POINT ( 'NONE',  ( -27.24356964374999635, 198.9406250006145171, 15.72908226750539384 ) ) ;
#2123 = CARTESIAN_POINT ( 'NONE',  ( 26.75643035624999655, 3.323476615752271712, -7.190624999385489602 ) ) ;
#2124 = CARTESIAN_POINT ( 'NONE',  ( -2.660918448318004614, 36.10231371789853938, -12.46528703574811558 ) ) ;
#2125 = ORIENTED_EDGE ( 'NONE', *, *, #27701, .F. ) ;
#2126 = UNCERTAINTY_MEASURE_WITH_UNIT (LENGTH_MEASURE( 1.000000000000000082E-05 ), #20862, 'distance_accuracy_value', 'NONE');
#2127 = CARTESIAN_POINT ( 'NONE',  ( 22.80587116629411781, 7.646167579472024665E-16, -0.4218749993855352987 ) ) ;
#2128 = CARTESIAN_POINT ( 'NONE',  ( 10.56230152254410903, 0.000000000000000000, -5.737499998771017573 ) ) ;
#2129 = CARTESIAN_POINT ( 'NONE',  ( -30.40252896937849769, 206.6499508600178387, -5.571401726697954970 ) ) ;
#2130 = CARTESIAN_POINT ( 'NONE',  ( -42.67336230271183695, 215.6869285224997270, 3.149950860017831200 ) ) ;
#2131 = LINE ( 'NONE', #10852, #3467 ) ;
#2132 = PRESENTATION_STYLE_ASSIGNMENT (( #28100 ) ) ;
#2133 = CARTESIAN_POINT ( 'NONE',  ( -26.99999999999999645, 196.4375000000000284, 15.58845726811991561 ) ) ;
#2134 = CARTESIAN_POINT ( 'NONE',  ( 12.53471296425189330, 75.77731371789855075, 2.311890736173451977 ) ) ;
#2135 = CARTESIAN_POINT ( 'NONE',  ( -64.64211230271182274, 205.5309553116392465, 1.321298161741817356 ) ) ;
#2136 = CARTESIAN_POINT ( 'NONE',  ( -43.07663769728823411, 204.3130714775002730, 3.149950860017883603 ) ) ;
#2137 = CARTESIAN_POINT ( 'NONE',  ( -1.045839947578415010E-13, 195.7250000012290343, 27.00000000000000355 ) ) ;
#2138 = DIRECTION ( 'NONE',  ( 0.000000000000000000, 0.000000000000000000, 1.000000000000000000 ) ) ;
#2139 = CARTESIAN_POINT ( 'NONE',  ( -8.927990412390371944, 35.52731371789855075, -13.04141134922778988 ) ) ;
#2140 = CARTESIAN_POINT ( 'NONE',  ( -38.51711230271182984, 218.4690446883607535, -2.393094931466363651 ) ) ;
#2141 = CARTESIAN_POINT ( 'NONE',  ( -7.228626920339069173, 20.47268628210144570, 10.49813415415989581 ) ) ;
#2142 = CARTESIAN_POINT ( 'NONE',  ( 7.228626920339068285, 61.87268628210145494, -10.49813415415989581 ) ) ;
#2143 = CARTESIAN_POINT ( 'NONE',  ( -10.83675517735155047, 4.660186282101435928, -11.08355503943142750 ) ) ;
#2144 = CARTESIAN_POINT ( 'NONE',  ( 10.56230152254410726, 0.000000000000000000, -1.350000000000045608 ) ) ;
#2145 = CARTESIAN_POINT ( 'NONE',  ( -1.045839947578415010E-13, 194.8250000012290570, 27.00000000000000355 ) ) ;
#2146 = VERTEX_POINT ( 'NONE', #35428 ) ;
#2147 = CARTESIAN_POINT ( 'NONE',  ( -6.092822981423970496, 38.58518628210143930, 14.25334919248782661 ) ) ;
#2148 = CARTESIAN_POINT ( 'NONE',  ( -1.926257025242585782E-15, 195.6406250006145342, -31.45816453501076637 ) ) ;
#2149 = CARTESIAN_POINT ( 'NONE',  ( 13.62178482187499640, 197.4593750006145285, -23.59362340125807123 ) ) ;
#2150 = LINE ( 'NONE', #1964, #13540 ) ;
#2151 = CARTESIAN_POINT ( 'NONE',  ( 24.99999999999999289, 0.000000000000000000, -8.000000000000000000 ) ) ;
#2152 = CARTESIAN_POINT ( 'NONE',  ( 1.120210788295102201E-13, 196.4000000012290741, -27.00000000000000711 ) ) ;
#2153 = AXIS2_PLACEMENT_3D ( 'NONE', #3610, #32227, #12521 ) ;
#2154 = CARTESIAN_POINT ( 'NONE',  ( 21.00000000000000000, 247.7218750006145171, 6.646953231504538984 ) ) ;
#2155 = CARTESIAN_POINT ( 'NONE',  ( -8.152565276336593669, 117.7523137178985735, -5.233372021372610483 ) ) ;
#2156 = CARTESIAN_POINT ( 'NONE',  ( 23.87821517812499650, 242.5093750006145399, -4.985214923628404904 ) ) ;
#2157 = ORIENTED_EDGE ( 'NONE', *, *, #11690, .F. ) ;
#2158 = CYLINDRICAL_SURFACE ( 'NONE', #6659, 5.999999999999999112 ) ;
#2159 = CARTESIAN_POINT ( 'NONE',  ( 24.00000000000000000, 247.9562500012290229, 5.196152422706629359 ) ) ;
#2160 = CARTESIAN_POINT ( 'NONE',  ( -4.622313124798826500, 115.1648137178985678, 11.61527771782809637 ) ) ;
#2161 = CARTESIAN_POINT ( 'NONE',  ( 19.68408634441910721, -5.407089921784855591, -9.440624999385555327 ) ) ;
#2162 = CARTESIAN_POINT ( 'NONE',  ( 33.86345018673919327, -5.407089921784855591, 161.2114445675243530 ) ) ;
#2163 = CARTESIAN_POINT ( 'NONE',  ( 21.00000000000000000, 6.646953231504538984, -0.8156249993854914893 ) ) ;
#2164 = CARTESIAN_POINT ( 'NONE',  ( 26.99999999999999645, 196.2125000000000057, -15.58845726811990495 ) ) ;
#2165 = EDGE_CURVE ( 'NONE', #205, #18251, #37105, .T. ) ;
#2166 = VERTEX_POINT ( 'NONE', #35239 ) ;
#2167 = VERTEX_POINT ( 'NONE', #29940 ) ;
#2168 = ORIENTED_EDGE ( 'NONE', *, *, #25401, .F. ) ;
#2169 = CARTESIAN_POINT ( 'NONE',  ( 21.00000000000000000, -6.928203230275506996, -5.681249998770944387 ) ) ;
#2170 = CARTESIAN_POINT ( 'NONE',  ( 20.99999999999999645, 6.646953231504538984, -3.403124999385474858 ) ) ;
#2171 = CARTESIAN_POINT ( 'NONE',  ( 22.56230152254410726, 7.347880794884117764E-16, -3.262499998771012599 ) ) ;
#2172 = CARTESIAN_POINT ( 'NONE',  ( 15.00000000000021316, 3.464101615137874735, -4.537499999999988987 ) ) ;
#2173 = CARTESIAN_POINT ( 'NONE',  ( 18.12178482187500350, 248.0218750006145001, 4.985214923628407568 ) ) ;
#2174 = CARTESIAN_POINT ( 'NONE',  ( 12.46528703574805874, 63.59768628210145636, 2.660918448318279950 ) ) ;
#2175 = CARTESIAN_POINT ( 'NONE',  ( 0.000000000000000000, 0.000000000000000000, 5.000000000000000000 ) ) ;
#2176 = EDGE_CURVE ( 'NONE', #26234, #22829, #20863, .T. ) ;
#2177 = CARTESIAN_POINT ( 'NONE',  ( 15.38158308873944158, 224.9824450966943346, -2.114697272284929763 ) ) ;
#2178 = CARTESIAN_POINT ( 'NONE',  ( -37.13169563604516554, 210.1155267958017703, 4.499999999999996447 ) ) ;
#2179 = CARTESIAN_POINT ( 'NONE',  ( 37.03385145495223441, 7.347880794884117764E-16, 164.4254812707998497 ) ) ;
#2180 = CARTESIAN_POINT ( 'NONE',  ( 11.48171059495408208, 130.1148137178985564, -4.944772684328420986 ) ) ;
#2181 = CARTESIAN_POINT ( 'NONE',  ( -36.14955436395490551, 214.8429017333601792, -4.673758765035196383 ) ) ;
#2182 = CARTESIAN_POINT ( 'NONE',  ( -58.31622103062156981, 212.1620413398628671, 8.530955311639223382 ) ) ;
#2183 = ADVANCED_FACE ( 'NONE', ( #24261 ), #18015, .T. ) ;
#2184 = CARTESIAN_POINT ( 'NONE',  ( 18.12178482187499640, 4.985214923628404904, -2.578124999385478233 ) ) ;
#2185 = CARTESIAN_POINT ( 'NONE',  ( -13.62178482187498396, 197.1781250006145569, 23.59362340125808188 ) ) ;
#2186 = CARTESIAN_POINT ( 'NONE',  ( 3.257655550456945548, 86.70231371789851949, 15.46528703574811736 ) ) ;
#2187 = CARTESIAN_POINT ( 'NONE',  ( -67.21502896937850835, 217.3034525342667962, -4.350049139982195001 ) ) ;
#2188 = EDGE_CURVE ( 'NONE', #6071, #13579, #21881, .T. ) ;
#2189 = VERTEX_POINT ( 'NONE', #21239 ) ;
#2190 = CARTESIAN_POINT ( 'NONE',  ( 26.99999999999983658, -3.464101615137843648, -6.562499999999986677 ) ) ;
#2191 = CARTESIAN_POINT ( 'NONE',  ( -8.962234695871760692, 131.1601862821014777, 8.715434833791933400 ) ) ;
#2192 = CARTESIAN_POINT ( 'NONE',  ( -15.50000000000000533, 58.71018628210145351, -0.1745138560725808530 ) ) ;
#2193 = CARTESIAN_POINT ( 'NONE',  ( 17.00000000000000000, 4.898587196589406912E-16, 50.17464377163448574 ) ) ;
#2194 = CARTESIAN_POINT ( 'NONE',  ( 37.24953043470598146, 7.646167579472024665E-16, 164.0960550422537096 ) ) ;
#2195 = CARTESIAN_POINT ( 'NONE',  ( -6.092822981423970496, 84.58518628210146062, 14.25334919248782661 ) ) ;
#2196 = VECTOR ( 'NONE', #32723, 1000.000000000000114 ) ;
#2197 = CARTESIAN_POINT ( 'NONE',  ( -46.44122103062156270, 208.3738570449994256, -6.530955311639227823 ) ) ;
#2198 = CARTESIAN_POINT ( 'NONE',  ( 19.68408634441910721, 5.407089921784857367, -5.690624999385579308 ) ) ;
#2199 = CARTESIAN_POINT ( 'NONE',  ( 9.465287035748067623, 17.59768628210143504, 2.064181346179272847 ) ) ;
#2200 = PLANE ( 'NONE',  #31590 ) ;
#2201 = CARTESIAN_POINT ( 'NONE',  ( -68.40997103062156270, 215.5714017266979852, 3.350049139982118618 ) ) ;
#2202 = DIRECTION ( 'NONE',  ( -1.000000000000000000, 0.000000000000000000, 0.000000000000000000 ) ) ;
#2203 = CARTESIAN_POINT ( 'NONE',  ( 2.660918448318279950, 61.29768628210143788, -12.46528703574805697 ) ) ;
#2204 = CARTESIAN_POINT ( 'NONE',  ( 26.99999999999999645, 197.5624999999999716, -15.58845726811990495 ) ) ;
#2205 = CARTESIAN_POINT ( 'NONE',  ( 7.234628195640295800, 197.5450961906613827, 27.00000000000001066 ) ) ;
#2207 = CARTESIAN_POINT ( 'NONE',  ( 10.31873187879410736, -3.604726614523244610, -1.509374999385515670 ) ) ;
#2206 = CARTESIAN_POINT ( 'NONE',  ( 8.843639120294328748, 25.93518628210144072, -3.474262827703334722 ) ) ;
#2208 = CARTESIAN_POINT ( 'NONE',  ( 15.24356964375000167, 248.9968750006145513, 3.323476615752272600 ) ) ;
#2209 = VERTEX_POINT ( 'NONE', #32966 ) ;
#2210 = CARTESIAN_POINT ( 'NONE',  ( 26.99999999999999645, 7.347880794884117764E-16, -3.374999999999989342 ) ) ;
#2211 = CARTESIAN_POINT ( 'NONE',  ( 25.96202780814182631, -3.113882786269718483, -8.000000000000003553 ) ) ;
#2212 = CARTESIAN_POINT ( 'NONE',  ( 36.97825818540390941, 3.604726614523243278, 160.9953990444431611 ) ) ;
#2213 = CARTESIAN_POINT ( 'NONE',  ( 16.56230152254411436, 7.209453229046475009, -2.053124999385520066 ) ) ;
#2214 = CARTESIAN_POINT ( 'NONE',  ( 34.50404489593442747, 5.407089921784857367, 168.5334755984986828 ) ) ;
#2215 = CARTESIAN_POINT ( 'NONE',  ( 21.00000000000000000, 244.4874999999999829, -6.928203230275506996 ) ) ;
#2216 = CARTESIAN_POINT ( 'NONE',  ( 1.069080835302379631E-14, 195.6124999999999829, 27.00000000000000000 ) ) ;
#2217 = CARTESIAN_POINT ( 'NONE',  ( -10.49813415415989404, 87.17268628210145209, -7.228626920339069173 ) ) ;
#2218 = EDGE_LOOP ( 'NONE', ( #26929, #14715, #15035, #29987 ) ) ;
#2219 = ORIENTED_EDGE ( 'NONE', *, *, #1145, .T. ) ;
#2220 = CARTESIAN_POINT ( 'NONE',  ( 13.49999999999999645, 196.8125000012290400, -23.38268590217984766 ) ) ;
#2221 = CARTESIAN_POINT ( 'NONE',  ( 10.49999999999999645, 252.0000000000000000, 2.500000000000000000 ) ) ;
#2222 = EDGE_CURVE ( 'NONE', #13040, #5701, #9847, .T. ) ;
#2223 = CARTESIAN_POINT ( 'NONE',  ( 13.23911966647199812, 48.75231371789854506, 8.632099005475788900 ) ) ;
#2224 = CARTESIAN_POINT ( 'NONE',  ( 26.75643035624999655, 3.323476615752271712, -9.440624999385470062 ) ) ;
#2225 = ADVANCED_FACE ( 'NONE', ( #12877 ), #29745, .F. ) ;
#2226 = CARTESIAN_POINT ( 'NONE',  ( 21.00000000000000000, 242.0968750006145456, -6.646953231504538984 ) ) ;
#2227 = CARTESIAN_POINT ( 'NONE',  ( -52.77455436395490551, 206.6211998817774997, 3.209657149897401585 ) ) ;
#2228 = VECTOR ( 'NONE', #19325, 1000.000000000000000 ) ;
#2229 = CARTESIAN_POINT ( 'NONE',  ( 20.00041244883536606, 239.7473985345926053, -5.668978318349186196 ) ) ;
#2230 = CARTESIAN_POINT ( 'NONE',  ( -5.233372021372612259, 32.65231371789855075, 8.152565276336593669 ) ) ;
#2231 = ADVANCED_FACE ( 'NONE', ( #15730 ), #27280, .F. ) ;
#2232 = CARTESIAN_POINT ( 'NONE',  ( 22.80587116629410716, 7.646167579472015790E-16, -9.365624999385563143 ) ) ;
#2233 = CARTESIAN_POINT ( 'NONE',  ( -0.1745138560723084320, 91.58981371789856496, -9.500000000000005329 ) ) ;
#2234 = CARTESIAN_POINT ( 'NONE',  ( -13.62178482187498396, 199.0343750006145456, 23.59362340125808188 ) ) ;
#2235 = CARTESIAN_POINT ( 'NONE',  ( 4.622313124798831829, 18.56481371789855928, -11.61527771782809282 ) ) ;
#2236 = EDGE_CURVE ( 'NONE', #14024, #33229, #26477, .T. ) ;
#2237 = CARTESIAN_POINT ( 'NONE',  ( -12.50000000000000355, 67.91018628210144925, -0.1745138560725492671 ) ) ;
#2238 = CARTESIAN_POINT ( 'NONE',  ( 10.56230152254411259, -3.464101615137757051, -10.19999999877101082 ) ) ;
#2239 = FACE_OUTER_BOUND ( 'NONE', #20647, .T. ) ;
#2240 = CARTESIAN_POINT ( 'NONE',  ( 33.98111043944852128, -5.407089921784855591, 162.5563074099482037 ) ) ;
#2241 = CARTESIAN_POINT ( 'NONE',  ( 10.31873187879411091, -3.604726614523244610, -9.609374999385535077 ) ) ;
#2242 = CARTESIAN_POINT ( 'NONE',  ( 16.56230152254411436, -7.209453229046482114, -5.934374999385510385 ) ) ;
#2243 = CYLINDRICAL_SURFACE ( 'NONE', #18562, 5.999999999999994671 ) ;
#2244 = DIRECTION ( 'NONE',  ( 0.000000000000000000, 0.000000000000000000, 1.000000000000000000 ) ) ;
#2245 = CARTESIAN_POINT ( 'NONE',  ( -8.710071997420127943, 68.48518628210145209, -3.796722387233380402 ) ) ;
#2246 = DIRECTION ( 'NONE',  ( 0.000000000000000000, 0.000000000000000000, -1.000000000000000000 ) ) ;
#2247 = CARTESIAN_POINT ( 'NONE',  ( 2.311890736173175753, 111.3226862821014720, 12.53471296425194836 ) ) ;
#2248 = CYLINDRICAL_SURFACE ( 'NONE', #20898, 8.000000000000000000 ) ;
#2249 = CARTESIAN_POINT ( 'NONE',  ( 26.99999999999999645, 248.5187500012290513, -3.464101615137755275 ) ) ;
#2250 = ORIENTED_EDGE ( 'NONE', *, *, #33561, .F. ) ;
#2251 = CARTESIAN_POINT ( 'NONE',  ( 34.11184405356999605, 5.407089921784857367, 164.0505994570858093 ) ) ;
#2252 = CARTESIAN_POINT ( 'NONE',  ( 21.00000000000000000, 6.646953231504538984, -4.303124999385465443 ) ) ;
#2253 = AXIS2_PLACEMENT_3D ( 'NONE', #35133, #26231, #3115 ) ;
#2254 = CARTESIAN_POINT ( 'NONE',  ( 13.62178482187501416, 197.7593750006145399, 23.59362340125806767 ) ) ;
#2255 = CARTESIAN_POINT ( 'NONE',  ( 28.20742792136773858, 5.407089921784862696, 168.1997419705030552 ) ) ;
#2256 = CARTESIAN_POINT ( 'NONE',  ( 34.19887935716262461, 5.196152422706637353, 166.4427416532051609 ) ) ;
#2257 = CARTESIAN_POINT ( 'NONE',  ( 0.000000000000000000, 200.0000000000000000, 0.000000000000000000 ) ) ;
#2258 = CARTESIAN_POINT ( 'NONE',  ( 26.75643035624999655, 241.0468750006145058, 3.323476615752267715 ) ) ;
#2259 = DIRECTION ( 'NONE',  ( 0.000000000000000000, 0.000000000000000000, -1.000000000000000000 ) ) ;
#2260 = CARTESIAN_POINT ( 'NONE',  ( -10.49813415416004858, 134.4273137178985849, 7.228626920338839135 ) ) ;
#2261 = CARTESIAN_POINT ( 'NONE',  ( -10.69584247140444866, 140.6476862821014890, 6.932735513423972762 ) ) ;
#2263 = VERTEX_POINT ( 'NONE', #3405 ) ;
#2262 = VERTEX_POINT ( 'NONE', #29366 ) ;
#2264 = CARTESIAN_POINT ( 'NONE',  ( 15.24356964374999990, 244.3468750006145171, 0.000000000000000000 ) ) ;
#2265 = B_SPLINE_CURVE_WITH_KNOTS ( 'NONE', 3,
 ( #22801, #8950, #17115, #34351 ),
 .UNSPECIFIED., .F., .F.,
 ( 4, 4 ),
 ( 0.000000000000000000, 1.000000000000000000 ),
 .UNSPECIFIED. ) ;
#2266 = LINE ( 'NONE', #16314, #18341 ) ;
#2267 = EDGE_CURVE ( 'NONE', #1610, #12755, #4683, .T. ) ;
#2268 = CARTESIAN_POINT ( 'NONE',  ( 23.87821517812499650, 4.985214923628404904, -4.340624999385478411 ) ) ;
#2269 = CARTESIAN_POINT ( 'NONE',  ( 15.50000000000000533, 112.2898137178985678, -0.1745138560722452326 ) ) ;
#2270 = DIRECTION ( 'NONE',  ( -0.000000000000000000, -1.000000000000000000, -0.000000000000000000 ) ) ;
#2271 = CARTESIAN_POINT ( 'NONE',  ( 18.12178482187500350, -4.985214923628407568, -0.6281249993854709501 ) ) ;
#2272 = CARTESIAN_POINT ( 'NONE',  ( 22.80587116629412137, 7.646167579472024665E-16, -8.521874999385502747 ) ) ;
#2273 = PRODUCT_DEFINITION_SHAPE ( 'NONE', 'NONE',  #37511 ) ;
#2274 = CARTESIAN_POINT ( 'NONE',  ( -13.50000000000000533, 199.1375000012290286, -23.38268590217984411 ) ) ;
#2275 = CARTESIAN_POINT ( 'NONE',  ( -6.932735513423968321, 106.1476862821014606, -10.69584247140445221 ) ) ;
#2276 = CARTESIAN_POINT ( 'NONE',  ( 13.44051670066911264, -5.407089921784859143, -2.765624999385540850 ) ) ;
#2277 = CARTESIAN_POINT ( 'NONE',  ( -46.43377896937850835, 207.8379586601372750, 8.530955311639258909 ) ) ;
#2278 = CARTESIAN_POINT ( 'NONE',  ( 20.99999999999999645, 243.7843750006145171, -6.646953231504538984 ) ) ;
#2279 = CARTESIAN_POINT ( 'NONE',  ( 26.97716818855048260, 0.000000000000000000, 49.47706554351410801 ) ) ;
#2280 = CARTESIAN_POINT ( 'NONE',  ( -32.18377896937850124, 208.9097554298617183, 4.530955311639234040 ) ) ;
#2281 = CARTESIAN_POINT ( 'NONE',  ( -0.1745138560725500443, 120.8101862821014691, 12.50000000000000355 ) ) ;
#2282 = CARTESIAN_POINT ( 'NONE',  ( 10.56230152254410903, 3.464101615137752166, -1.274999998770995679 ) ) ;
#2283 =( REPRESENTATION_RELATIONSHIP ('NONE','NONE', #4304, #6520 ) REPRESENTATION_RELATIONSHIP_WITH_TRANSFORMATION ( #1064 )SHAPE_REPRESENTATION_RELATIONSHIP( ) );
#2284 = CARTESIAN_POINT ( 'NONE',  ( -43.27455436395490551, 205.1570982666397356, 4.673758765035198159 ) ) ;
#2285 = DIRECTION ( 'NONE',  ( -0.000000000000000000, -1.000000000000000000, -0.000000000000000000 ) ) ;
#2286 = DIRECTION ( 'NONE',  ( 0.000000000000000000, 0.000000000000000000, -1.000000000000000000 ) ) ;
#2287 = CARTESIAN_POINT ( 'NONE',  ( -3.257655550457281723, 111.8976862821014606, 15.46528703574804986 ) ) ;
#2288 = CARTESIAN_POINT ( 'NONE',  ( -4.944772684328673229, 10.98518628210143433, 11.48171059495397728 ) ) ;
#2289 =( BOUNDED_CURVE ( )  B_SPLINE_CURVE ( 2, ( #27246, #1836, #16257, #30474, #1269, #21760, #1651 ),
 .UNSPECIFIED., .F., .F. ) 
 B_SPLINE_CURVE_WITH_KNOTS ( ( 3, 2, 2, 3 ),
 ( 0.7173913043478249429, 0.7246376811594196221, 0.7318840579710143013, 0.7349428514613199903 ),
 .UNSPECIFIED. ) 
 CURVE ( )  GEOMETRIC_REPRESENTATION_ITEM ( )  RATIONAL_B_SPLINE_CURVE ( ( 1.000000000000020428, 0.8660254037844181685, 1.000000000000000000, 0.8660254037844387076, 1.000000000000000000, 0.9434475140576754626, 0.9346381638529801528 ) ) 
 REPRESENTATION_ITEM ( '' )  );
#2290 = DIRECTION ( 'NONE',  ( 0.000000000000000000, -0.000000000000000000, 1.000000000000000000 ) ) ;
#2291 = CARTESIAN_POINT ( 'NONE',  ( -7.954856959092191815, 123.9726862821014493, -5.529263428287477744 ) ) ;
#2292 = CARTESIAN_POINT ( 'NONE',  ( 19.68408634441910721, 5.407089921784857367, -0.2906249993855358760 ) ) ;
#2293 = CYLINDRICAL_SURFACE ( 'NONE', #36650, 5.999999999999998224 ) ;
#2294 = ORIENTED_EDGE ( 'NONE', *, *, #16417, .T. ) ;
#2295 = CARTESIAN_POINT ( 'NONE',  ( 20.99999999999999645, 185.0294372515228645, 0.000000000000000000 ) ) ;
#2296 = CARTESIAN_POINT ( 'NONE',  ( 5.529263428287477744, 80.27268628210143220, -7.954856959092191815 ) ) ;
#2297 = SURFACE_STYLE_USAGE ( .BOTH. , #31119 ) ;
#2298 = CARTESIAN_POINT ( 'NONE',  ( 27.24356964375000700, 195.9406250006145456, 15.72908226750537075 ) ) ;
#2299 = CARTESIAN_POINT ( 'NONE',  ( 23.99999999999999645, 5.196152422706631135, -2.849999999999991651 ) ) ;
#2300 = CARTESIAN_POINT ( 'NONE',  ( -13.62178482187498396, 197.6843750006145228, 23.59362340125808188 ) ) ;
#2301 = EDGE_CURVE ( 'NONE', #8916, #12071, #18778, .T. ) ;
#2302 = CARTESIAN_POINT ( 'NONE',  ( 25.01087993033039325, 0.000000000000000000, 164.6868468578000488 ) ) ;
#2303 = CARTESIAN_POINT ( 'NONE',  ( 22.56230152254390475, 3.464101615137881840, -3.787500000000044942 ) ) ;
#2304 = CARTESIAN_POINT ( 'NONE',  ( 1.715153634034445762, 55.07731371789854080, -9.534712964251895073 ) ) ;
#2305 = CARTESIAN_POINT ( 'NONE',  ( 26.99999999999999645, 3.464101615137755275, -8.287500000000004974 ) ) ;
#2306 = AXIS2_PLACEMENT_3D ( 'NONE', #32116, #31750, #14880 ) ;
#2307 = ORIENTED_EDGE ( 'NONE', *, *, #11411, .F. ) ;
#2308 = ADVANCED_FACE ( 'NONE', ( #24627 ), #13071, .T. ) ;
#2309 = CARTESIAN_POINT ( 'NONE',  ( 23.99999999999999645, 240.9062500012290684, -5.196152422706631135 ) ) ;
#2310 = CARTESIAN_POINT ( 'NONE',  ( -12.53471296425189152, 71.17731371789855643, -2.311890736173453309 ) ) ;
#2311 = CARTESIAN_POINT ( 'NONE',  ( 16.56230152254411436, 7.209453229046482114, -7.059374999385483740 ) ) ;
#2312 = CARTESIAN_POINT ( 'NONE',  ( 21.00000000000000000, 6.646953231504538984, -7.115624999385463667 ) ) ;
#2313 = CARTESIAN_POINT ( 'NONE',  ( -4.622313124798826500, 32.36481371789854933, 11.61527771782809637 ) ) ;
#2314 = EDGE_CURVE ( 'NONE', #21803, #18034, #2265, .T. ) ;
#2315 =( BOUNDED_CURVE ( )  B_SPLINE_CURVE ( 2, ( #26791, #15432, #23962, #30909, #22012, #33566, #6519, #33750, #10623, #36582, #13286, #10250, #36206, #3671, #7417, #18988, #13100, #16511, #26981, #4562, #822, #35505, #16137, #19368, #22202, #24842, #28058, #15241, #1527, #32665, #13473, #36393, #25025, #7790, #6706, #10439, #24655, #18278, #7603, #30727, #16323, #18094, #29635, #9552, #29822, #28420, #3017, #17250, #20096, #37499, #16884, #26139, #34488, #36950, #25584, #11551, #22568, #10812, #31825, #31097, #22384, #8348, #5306, #23124, #33934, #37320, #7975, #22942, #16698, #31278, #2276, #20285, #11370, #8530, #14586, #34668, #8713, #25957, #2641, #37137, #11182, #28791, #28976, #5119, #19740, #2460, #5860, #31642, #28246, #19549, #34115, #19920, #5670, #2828, #28604, #13853, #14400, #25400, #10997, #17438, #8166, #14034, #14218, #22755, #34304, #31459, #25768, #5482, #17066, #23873, #26893, #20657, #26510, #21226, #15339, #29731, #15147, #35604, #32389, #541, #11923, #14963, #923, #23490, #172, #32766, #20473, #11739, #12492, #6429, #35041, #24059, #18190, #3765, #9650, #35412, #35227, #32012, #12107, #6802, #3202, #18003, #29546, #32204, #18377, #29927, #3955, #15530, #23309, #359, #727, #14778, #21038, #9276, #34855, #8895, #23680, #20848, #6043, #3584, #17629, #26697, #12299, #9462, #29159, #26322, #32575, #9088, #6239, #6615, #17816, #29354, #3394, #24433, #24617, #7193, #7743, #24799, #7006, #13249, #7561, #19327, #36538, #30864, #27270, #16282, #21972, #36164, #19136, #30118, #10581, #15910, #18576, #22160, #33704, #33335, #18946, #36350, #21600, #10019, #21784, #10395, #10210, #4889, #27086, #1486, #13060, #12678, #7375, #24977, #21412, #33149, #1111, #4148, #24248, #33517, #18764, #4703, #1860, #35792, #1296, #30684, #35983, #30500, #30306, #9834, #27830, #15720, #13429, #32954, #4521, #12867, #4330, #27458, #16095, #27648, #1675, #25542, #28013, #5440, #31781, #8669, #28561, #36728, #25728, #17022, #2232, #19695, #2418, #28382, #37094, #37281, #13812, #13991, #2602, #22898, #34625, #10767, #25359, #34073, #11510, #2046, #22339, #13625, #36904 ),
 .UNSPECIFIED., .F., .F. ) 
 B_SPLINE_CURVE_WITH_KNOTS ( ( 3, 2, 2, 2, 2, 2, 2, 2, 2, 2, 2, 2, 2, 2, 2, 2, 2, 2, 2, 2, 2, 2, 2, 2, 2, 2, 2, 2, 2, 2, 2, 2, 2, 2, 2, 2, 2, 2, 2, 2, 2, 2, 2, 2, 2, 2, 2, 2, 2, 2, 2, 2, 2, 2, 2, 2, 2, 2, 2, 2, 2, 2, 2, 2, 2, 2, 2, 2, 2, 2, 2, 2, 2, 2, 2, 2, 2, 2, 2, 2, 2, 2, 2, 2, 2, 2, 2, 2, 2, 2, 2, 2, 2, 2, 2, 2, 2, 2, 2, 2, 2, 2, 2, 2, 2, 2, 2, 2, 2, 2, 2, 2, 2, 2, 2, 2, 2, 2, 2, 2, 2, 2, 2, 2, 2, 2, 2, 2, 2, 2, 2, 2, 3 ),
 ( 0.000000000000000000, 0.007499808116169960973, 0.01499961623233992195, 0.02249942434850988118, 0.02999923246467984389, 0.03749904058084980313, 0.04499884869701976237, 0.05249865681318972854, 0.05999846492935968778, 0.06749827304552964702, 0.07499808116169960626, 0.08249788927786955162, 0.08999769739403952473, 0.09749750551020949785, 0.1049973136263794571, 0.1124971217425494163, 0.1199969298587193756, 0.1274967379748893348, 0.1349965460910592940, 0.1424963542072292533, 0.1499961623233992125, 0.1574959704395691995, 0.1649957785557391032, 0.1724955866719090902, 0.1799953947880790495, 0.1874952029042490087, 0.1949950110204189957, 0.2024948191365889549, 0.2099946272527589142, 0.2174944353689288457, 0.2249942434850988326, 0.2324940516012687641, 0.2399938597174387511, 0.2474936678336087381, 0.2549934759497786696, 0.2624932840659486288, 0.2699930921821185881, 0.2774929002982886028, 0.2849927084144585065, 0.2924925165306284103, 0.2999923246467984250, 0.3074921327629683843, 0.3149919408791383990, 0.3224917489953083582, 0.3299915571114782065, 0.3374913652276482212, 0.3449911733438181805, 0.3524909814599881952, 0.3599907895761580989, 0.3674905976923280582, 0.3749904058084980174, 0.3824902139246679766, 0.3899900220408379914, 0.3974898301570078951, 0.4049896382731779099, 0.4124894463893478136, 0.4199892545055178283, 0.4274890626216877321, 0.4349888707378576913, 0.4424886788540277061, 0.4499884869701976653, 0.4574882950863676245, 0.4649881032025375283, 0.4724879113187074875, 0.4799877194348775022, 0.4874875275510474615, 0.4949873356672174762, 0.5024871437833873244, 0.5099869518995573392, 0.5174867600157272429, 0.5249865681318972577, 0.5324863762480671614, 0.5399861843642371761, 0.5474859924804070799, 0.5549858005965772056, 0.5624856087127469983, 0.5699854168289170131, 0.5774852249450870278, 0.5849850330612568206, 0.5924848411774269463, 0.5999846492935968501, 0.6074844574097668648, 0.6149842655259367685, 0.6224840736421066723, 0.6299838817582767980, 0.6374836898744465907, 0.6449834979906167165, 0.6524833061067866202, 0.6599831142229564129, 0.6674829223391265387, 0.6749827304552964424, 0.6824825385714665682, 0.6899823466876363609, 0.6974821548038062646, 0.7049819629199763904, 0.7124817710361461831, 0.7199815791523161979, 0.7274813872684862126, 0.7349811953846561163, 0.7424810035008261311, 0.7499808116169960348, 0.7574806197331660496, 0.7649804278493359533, 0.7724802359655059680, 0.7799800440816759828, 0.7874798521978458865, 0.7949796603140157902, 0.8024794684301858050, 0.8099792765463558197, 0.8174790846625257235, 0.8249788927786956272, 0.8324787008948656419, 0.8399785090110356567, 0.8474783171272055604, 0.8549781252433754641, 0.8624779333595454789, 0.8699777414757153826, 0.8774775495918853974, 0.8849773577080554121, 0.8924771658242253158, 0.8999769739403953306, 0.9074767820565652343, 0.9149765901727352491, 0.9224763982889051528, 0.9299762064050750565, 0.9374760145212451823, 0.9449758226374149750, 0.9524756307535849897, 0.9599754388697550045, 0.9674752469859249082, 0.9749750551020949230, 0.9824748632182648267, 0.9859330816693211430 ),
 .UNSPECIFIED. ) 
 CURVE ( )  GEOMETRIC_REPRESENTATION_ITEM ( )  RATIONAL_B_SPLINE_CURVE ( ( 1.000000000000000000, 0.8660254037844387076, 1.000000000000000000, 0.8660254037844387076, 1.000000000000000000, 0.8660254037844387076, 1.000000000000000000, 0.8660254037844387076, 1.000000000000000000, 0.8660254037844387076, 1.000000000000000000, 0.8660254037844387076, 1.000000000000000000, 0.8660254037844387076, 1.000000000000000000, 0.8660254037844387076, 1.000000000000000000, 0.8660254037844387076, 1.000000000000000000, 0.8660254037844387076, 1.000000000000000000, 0.8660254037844387076, 1.000000000000000000, 0.8660254037844387076, 1.000000000000000000, 0.8660254037844387076, 1.000000000000000000, 0.8660254037844387076, 1.000000000000000000, 0.8660254037844387076, 1.000000000000000000, 0.8660254037844387076, 1.000000000000000000, 0.8660254037844387076, 1.000000000000000000, 0.8660254037844387076, 1.000000000000000000, 0.8660254037844387076, 1.000000000000000000, 0.8660254037844387076, 1.000000000000000000, 0.8660254037844387076, 1.000000000000000000, 0.8660254037844387076, 1.000000000000000000, 0.8660254037844387076, 1.000000000000000000, 0.8660254037844387076, 1.000000000000000000, 0.8660254037844387076, 1.000000000000000000, 0.8660254037844387076, 1.000000000000000000, 0.8660254037844387076, 1.000000000000000000, 0.8660254037844387076, 1.000000000000000000, 0.8660254037844387076, 1.000000000000000000, 0.8660254037844387076, 1.000000000000000000, 0.8660254037844387076, 1.000000000000000000, 0.8660254037844387076, 1.000000000000000000, 0.8660254037844387076, 1.000000000000000000, 0.8660254037844387076, 1.000000000000000000, 0.8660254037844387076, 1.000000000000000000, 0.8660254037844387076, 1.000000000000000000, 0.8660254037844387076, 1.000000000000000000, 0.8660254037844387076, 1.000000000000000000, 0.8660254037844387076, 1.000000000000000000, 0.8660254037844387076, 1.000000000000000000, 0.8660254037844387076, 1.000000000000000000, 0.8660254037844387076, 1.000000000000000000, 0.8660254037844387076, 1.000000000000000000, 0.8660254037844387076, 1.000000000000000000, 0.8660254037844387076, 1.000000000000000000, 0.8660254037844387076, 1.000000000000000000, 0.8660254037844387076, 1.000000000000000000, 0.8660254037844387076, 1.000000000000000000, 0.8660254037844387076, 1.000000000000000000, 0.8660254037844387076, 1.000000000000000000, 0.8660254037844387076, 1.000000000000000000, 0.8660254037844387076, 1.000000000000000000, 0.8660254037844387076, 1.000000000000000000, 0.8660254037844387076, 1.000000000000000000, 0.8660254037844387076, 1.000000000000000000, 0.8660254037844387076, 1.000000000000000000, 0.8660254037844387076, 1.000000000000000000, 0.8660254037844387076, 1.000000000000000000, 0.8660254037844387076, 1.000000000000000000, 0.8660254037844387076, 1.000000000000000000, 0.8660254037844387076, 1.000000000000000000, 0.8660254037844387076, 1.000000000000000000, 0.8660254037844387076, 1.000000000000000000, 0.8660254037844387076, 1.000000000000000000, 0.8660254037844387076, 1.000000000000000000, 0.8660254037844387076, 1.000000000000000000, 0.8660254037844387076, 1.000000000000000000, 0.8660254037844387076, 1.000000000000000000, 0.8660254037844387076, 1.000000000000000000, 0.8660254037844387076, 1.000000000000000000, 0.8660254037844387076, 1.000000000000000000, 0.8660254037844387076, 1.000000000000000000, 0.8660254037844387076, 1.000000000000000000, 0.8660254037844387076, 1.000000000000000000, 0.8660254037844387076, 1.000000000000000000, 0.8660254037844387076, 1.000000000000000000, 0.8660254037844387076, 1.000000000000000000, 0.8660254037844387076, 1.000000000000000000, 0.8660254037844387076, 1.000000000000000000, 0.8660254037844387076, 1.000000000000000000, 0.8660254037844387076, 1.000000000000000000, 0.8660254037844387076, 1.000000000000000000, 0.8660254037844387076, 1.000000000000000000, 0.8660254037844387076, 1.000000000000000000, 0.8660254037844387076, 1.000000000000000000, 0.8660254037844387076, 1.000000000000000000, 0.8660254037844387076, 1.000000000000000000, 0.8660254037844387076, 1.000000000000000000, 0.8660254037844387076, 1.000000000000000000, 0.8660254037844387076, 1.000000000000000000, 0.8660254037844387076, 1.000000000000000000, 0.8660254037844387076, 1.000000000000000000, 0.8660254037844387076, 1.000000000000000000, 0.8660254037844387076, 1.000000000000000000, 0.8660254037844387076, 1.000000000000000000, 0.8660254037844387076, 1.000000000000000000, 0.8660254037844387076, 1.000000000000000000, 0.8660254037844387076, 1.000000000000000000, 0.8660254037844387076, 1.000000000000000000, 0.8660254037844387076, 1.000000000000000000, 0.8660254037844387076, 1.000000000000000000, 0.8660254037844387076, 1.000000000000000000, 0.8660254037844387076, 1.000000000000000000, 0.8660254037844387076, 1.000000000000000000, 0.8660254037844387076, 1.000000000000000000, 0.8660254037844387076, 1.000000000000000000, 0.8660254037844387076, 1.000000000000000000, 0.8660254037844387076, 1.000000000000000000, 0.8660254037844387076, 1.000000000000000000, 0.8660254037844387076, 1.000000000000000000, 0.8660254037844387076, 1.000000000000000000, 0.8660254037844387076, 1.000000000000000000, 0.8660254037844387076, 1.000000000000000000, 0.8660254037844387076, 1.000000000000000000, 0.8660254037844387076, 1.000000000000000000, 0.8660254037844387076, 1.000000000000000000, 0.8660254037844387076, 1.000000000000000000, 0.8660254037844387076, 1.000000000000000000, 0.8660254037844387076, 1.000000000000000000, 0.8660254037844387076, 1.000000000000000000, 0.8660254037844387076, 1.000000000000000000, 0.8660254037844387076, 1.000000000000000000, 0.8660254037844387076, 1.000000000000000000, 0.8660254037844387076, 1.000000000000000000, 0.8660254037844387076, 1.000000000000000000, 0.8660254037844387076, 1.000000000000000000, 0.8660254037844387076, 1.000000000000000000, 0.8660254037844387076, 1.000000000000000000, 0.8660254037844387076, 1.000000000000000000, 0.8660254037844387076, 1.000000000000000000, 0.8660254037844387076, 1.000000000000000000, 0.9382232967258800072, 0.9334180070662969619 ) ) 
 REPRESENTATION_ITEM ( '' )  );
#2316 = ORIENTED_EDGE ( 'NONE', *, *, #22130, .T. ) ;
#2317 = AXIS2_PLACEMENT_3D ( 'NONE', #21030, #26883, #32566 ) ;
#2318 = CARTESIAN_POINT ( 'NONE',  ( 10.31873187879410914, 0.000000000000000000, -2.446874999385534544 ) ) ;
#2319 = PRODUCT_RELATED_PRODUCT_CATEGORY ( 'part', '', ( #37371 ) ) ;
#2320 = CARTESIAN_POINT ( 'NONE',  ( 8.715434833791931624, 9.260186282101429356, 8.962234695871760692 ) ) ;
#2321 = CARTESIAN_POINT ( 'NONE',  ( 28.20742792136773858, 5.407089921784862696, 168.1997419705030552 ) ) ;
#2322 = CARTESIAN_POINT ( 'NONE',  ( -43.06919563604516554, 216.5000000000000000, -0.1155267958017906493 ) ) ;
#2323 = CARTESIAN_POINT ( 'NONE',  ( 37.38683221308021842, 7.347880794884117764E-16, 168.4600697980714017 ) ) ;
#2324 = CYLINDRICAL_SURFACE ( 'NONE', #23074, 8.000000000000000000 ) ;
#2325 = CARTESIAN_POINT ( 'NONE',  ( -34.17038769728823411, 208.6787018382581778, 4.469044688360752637 ) ) ;
#2326 = CARTESIAN_POINT ( 'NONE',  ( -43.47247103062156981, 206.6499508600178672, 5.571401726697986057 ) ) ;
#2327 = ORIENTED_EDGE ( 'NONE', *, *, #19803, .F. ) ;
#2328 = AXIS2_PLACEMENT_3D ( 'NONE', #30872, #25550, #34270 ) ;
#2329 = CARTESIAN_POINT ( 'NONE',  ( -28.81129111113878594, 202.7130252932614383, 3.311965150308325612 ) ) ;
#2330 = FACE_OUTER_BOUND ( 'NONE', #20588, .T. ) ;
#2331 = CARTESIAN_POINT ( 'NONE',  ( 15.53471296425188797, 38.97731371789853938, 2.908627838312457747 ) ) ;
#2332 = CARTESIAN_POINT ( 'NONE',  ( -30.40252896937850124, 205.6499508600178103, -7.303452534266820173 ) ) ;
#2333 = CARTESIAN_POINT ( 'NONE',  ( -12.46528703574805697, 12.99768628210143362, -2.660918448318280838 ) ) ;
#2334 = CARTESIAN_POINT ( 'NONE',  ( 11.48171059495397728, 63.88518628210145067, 4.944772684328674117 ) ) ;
#2335 = CARTESIAN_POINT ( 'NONE',  ( -13.04141134922759804, 13.57268628210145422, -8.927990412390657937 ) ) ;
#2336 = CARTESIAN_POINT ( 'NONE',  ( 19.56230152254411792, 5.196152422706637353, -1.950000000000035039 ) ) ;
#2337 = CARTESIAN_POINT ( 'NONE',  ( 13.50000000000001421, 194.8625000012290513, 23.38268590217984055 ) ) ;
#2338 = ORIENTED_EDGE ( 'NONE', *, *, #13660, .T. ) ;
#2339 = CARTESIAN_POINT ( 'NONE',  ( -14.38691631536207183, 21.33518628210144641, 5.770363421893814682 ) ) ;
#2340 = CARTESIAN_POINT ( 'NONE',  ( -27.24356964375000700, 194.8294844423495817, -9.915847621322177119 ) ) ;
#2341 = CARTESIAN_POINT ( 'NONE',  ( 27.24356964375000700, 199.1468750006145285, 15.72908226750537075 ) ) ;
#2342 = CARTESIAN_POINT ( 'NONE',  ( -3.253724281355068545E-15, 198.9874999999999829, -27.00000000000000000 ) ) ;
#2343 = CARTESIAN_POINT ( 'NONE',  ( 25.29522554115172639, 0.000000000000000000, 167.9369320615487311 ) ) ;
#2344 = FACE_OUTER_BOUND ( 'NONE', #9960, .T. ) ;
#2345 = CARTESIAN_POINT ( 'NONE',  ( 8.962234695871762469, 6.960186282101432198, -8.715434833791931624 ) ) ;
#2346 = CARTESIAN_POINT ( 'NONE',  ( 18.12178482187499640, 247.9843750006145342, -4.985214923628404904 ) ) ;
#2347 = CARTESIAN_POINT ( 'NONE',  ( -5.233372021372612259, 106.2523137178985451, 8.152565276336593669 ) ) ;
#2348 = CARTESIAN_POINT ( 'NONE',  ( 20.99999999999999645, 242.5468750006145342, -6.646953231504538984 ) ) ;
#2349 = ORIENTED_EDGE ( 'NONE', *, *, #7960, .F. ) ;
#2350 = CARTESIAN_POINT ( 'NONE',  ( -65.24330436395489130, 210.1155267958017134, -6.500000000000000888 ) ) ;
#2351 = SURFACE_STYLE_FILL_AREA ( #13545 ) ;
#2352 = CARTESIAN_POINT ( 'NONE',  ( -0.1745138560722763466, 119.1898137178985593, -12.50000000000000355 ) ) ;
#2353 = CARTESIAN_POINT ( 'NONE',  ( 10.31873187879411091, -3.604726614523240613, -10.00312499938551802 ) ) ;
#2354 = CARTESIAN_POINT ( 'NONE',  ( 37.01911243981686539, 7.646167579472015790E-16, 161.4623653091736628 ) ) ;
#2355 = DIRECTION ( 'NONE',  ( 0.000000000000000000, 0.000000000000000000, -1.000000000000000000 ) ) ;
#2356 = CARTESIAN_POINT ( 'NONE',  ( -1.909035429704832693E-15, 196.2875000000000227, -31.17691453623979214 ) ) ;
#2357 = VERTEX_POINT ( 'NONE', #405 ) ;
#2358 = ORIENTED_EDGE ( 'NONE', *, *, #23097, .T. ) ;
#2359 = ORIENTED_EDGE ( 'NONE', *, *, #5005, .F. ) ;
#2360 = CARTESIAN_POINT ( 'NONE',  ( 15.00000000000000000, 3.464101615137752166, -5.831249998770964282 ) ) ;
#2361 = CARTESIAN_POINT ( 'NONE',  ( 26.75643035624999655, -3.323476615752267271, -3.103124999385467042 ) ) ;
#2362 = CARTESIAN_POINT ( 'NONE',  ( 10.56230152254410726, 0.000000000000000000, -0.9000000000000396572 ) ) ;
#2363 = FACE_OUTER_BOUND ( 'NONE', #30294, .T. ) ;
#2364 = CARTESIAN_POINT ( 'NONE',  ( 21.00000000000000000, 249.6343750006145399, -6.646953231504538984 ) ) ;
#2365 = CARTESIAN_POINT ( 'NONE',  ( 12.53471296425194836, 53.82268628210144357, -2.311890736173178418 ) ) ;
#2366 = CARTESIAN_POINT ( 'NONE',  ( -58.11086230271183695, 213.1499508600178387, -5.686928522499747451 ) ) ;
#2367 = CARTESIAN_POINT ( 'NONE',  ( 5.205286459873386562, 215.9230175775471423, -0.9779651927395711652 ) ) ;
#2368 = CARTESIAN_POINT ( 'NONE',  ( -38.51711230271182984, 214.4690446883608104, -1.321298161741814914 ) ) ;
#2369 = CARTESIAN_POINT ( 'NONE',  ( 1.120210788295102201E-13, 197.1875000000000568, -27.00000000000000711 ) ) ;
#2370 = CARTESIAN_POINT ( 'NONE',  ( 24.98473320761322114, -3.464101615137757051, 164.3879884495968611 ) ) ;
#2371 = CARTESIAN_POINT ( 'NONE',  ( 8.962234695871567070, 122.6398137178985621, 8.715434833792127023 ) ) ;
#2372 = CARTESIAN_POINT ( 'NONE',  ( -34.76413769728823411, 213.1499508600178672, 5.686928522499718142 ) ) ;
#2373 = CARTESIAN_POINT ( 'NONE',  ( -39.71205436395491262, 216.1378603801730094, 6.307003348497944195 ) ) ;
#2374 = CARTESIAN_POINT ( 'NONE',  ( 26.75643035624999655, 3.323476615752271268, -1.340624999385481075 ) ) ;
#2375 = CARTESIAN_POINT ( 'NONE',  ( 13.62178482187499640, 196.5031250006145456, -23.59362340125807123 ) ) ;
#2376 = CARTESIAN_POINT ( 'NONE',  ( -11.08355503943118592, 90.43981371789854506, -10.83675517735179383 ) ) ;
#2377 = CARTESIAN_POINT ( 'NONE',  ( -66.02752896937849414, 214.3500491399821897, 7.303452534266821949 ) ) ;
#2378 = ORIENTED_EDGE ( 'NONE', *, *, #13301, .T. ) ;
#2379 = CARTESIAN_POINT ( 'NONE',  ( 20.99999999999999289, 240.8874999999999886, -5.999999999999997335 ) ) ;
#2380 = CARTESIAN_POINT ( 'NONE',  ( -12.50000000000000355, 113.9101862821014493, -0.1745138560725492671 ) ) ;
#2381 = EDGE_CURVE ( 'NONE', #34425, #11807, #4459, .T. ) ;
#2382 = CARTESIAN_POINT ( 'NONE',  ( 13.04141134922759804, 73.37268628210144072, 8.927990412390657937 ) ) ;
#2383 = CARTESIAN_POINT ( 'NONE',  ( 25.44230085693126497, 0.000000000000000000, 169.6180106133541869 ) ) ;
#2384 = CARTESIAN_POINT ( 'NONE',  ( 30.88264414254898682, 7.209453229046482114, 162.9591394389216532 ) ) ;
#2385 = CARTESIAN_POINT ( 'NONE',  ( 10.83675517735155225, 82.86018628210146630, 11.08355503943142573 ) ) ;
#2386 = CARTESIAN_POINT ( 'NONE',  ( 16.56230152254411081, 7.209453229046475009, -6.553124999385508964 ) ) ;
#2387 = CARTESIAN_POINT ( 'NONE',  ( 0.1745138560725194299, 24.21018628210144996, -9.500000000000005329 ) ) ;
#2388 = FACE_OUTER_BOUND ( 'NONE', #26406, .T. ) ;
#2389 = CARTESIAN_POINT ( 'NONE',  ( -63.46205436395489841, 214.6737587650352168, 4.842901733360204908 ) ) ;
#2390 = CARTESIAN_POINT ( 'NONE',  ( -77.00000000000002842, 210.0000000000000000, -3.000000000000000000 ) ) ;
#2391 = CARTESIAN_POINT ( 'NONE',  ( -0.1745138560725500443, 56.41018628210145636, 12.50000000000000355 ) ) ;
#2392 = CARTESIAN_POINT ( 'NONE',  ( -1.909035429704832693E-15, 198.0875000000000341, -31.17691453623979214 ) ) ;
#2393 = CYLINDRICAL_SURFACE ( 'NONE', #17194, 5.999999999999999112 ) ;
#2395 = CARTESIAN_POINT ( 'NONE',  ( 22.80587116629411781, 7.646167579472024665E-16, -0.8718749993855412495 ) ) ;
#2394 = CARTESIAN_POINT ( 'NONE',  ( 2.064181346179272847, 24.49768628210144072, -9.465287035748065847 ) ) ;
#2396 = CARTESIAN_POINT ( 'NONE',  ( 15.24356964375000167, 249.4468750006144830, 3.323476615752272600 ) ) ;
#2397 = ORIENTED_EDGE ( 'NONE', *, *, #35638, .F. ) ;
#2398 = CARTESIAN_POINT ( 'NONE',  ( 15.00000000000000000, 0.000000000000000000, -4.049999999999998046 ) ) ;
#2399 = CARTESIAN_POINT ( 'NONE',  ( 25.55176585154777769, -3.713212129012403828, -8.000000000000000000 ) ) ;
#2400 = CARTESIAN_POINT ( 'NONE',  ( 22.80587116629410360, 7.646167579472015790E-16, -2.615624999385557370 ) ) ;
#2401 = CARTESIAN_POINT ( 'NONE',  ( 33.61057809361597748, 5.196152422706637353, 159.7184274410858507 ) ) ;
#2402 = CARTESIAN_POINT ( 'NONE',  ( 18.00000000000000000, 244.5250000000000057, -5.196152422706630247 ) ) ;
#2403 = LINE ( 'NONE', #34432, #8203 ) ;
#2404 = ADVANCED_FACE ( 'NONE', ( #11971 ), #31579, .F. ) ;
#2405 = CARTESIAN_POINT ( 'NONE',  ( -2.660918448318275509, 93.49768628210145494, 12.46528703574805874 ) ) ;
#2406 = EDGE_LOOP ( 'NONE', ( #8339, #18616, #28272, #15794 ) ) ;
#2407 = VERTEX_POINT ( 'NONE', #6535 ) ;
#2408 = CARTESIAN_POINT ( 'NONE',  ( -13.49999999999998401, 196.1375000012290286, 23.38268590217985476 ) ) ;
#2409 = CARTESIAN_POINT ( 'NONE',  ( -82.45892874490161262, 210.6708926576488921, 5.000000000000000000 ) ) ;
#2410 = CARTESIAN_POINT ( 'NONE',  ( 14.38691631536194393, 30.06481371789855572, 5.770363421894124656 ) ) ;
#2411 = CARTESIAN_POINT ( 'NONE',  ( 23.87821517812499650, 4.985214923628404904, -8.053124999385484983 ) ) ;
#2412 = EDGE_CURVE ( 'NONE', #21814, #23956, #15632, .T. ) ;
#2413 = CARTESIAN_POINT ( 'NONE',  ( 23.87821517812500005, 241.9093750006145456, 4.985214923628404016 ) ) ;
#2414 = CARTESIAN_POINT ( 'NONE',  ( -40.50372103062156981, 214.5309553116392749, -1.090244570138262148 ) ) ;
#2415 = CARTESIAN_POINT ( 'NONE',  ( 28.46356835473687852, 5.196152422706636465, 169.7301163968956530 ) ) ;
#2416 = CARTESIAN_POINT ( 'NONE',  ( 30.78459393195788607, -7.209453229046482114, 161.8384204035683922 ) ) ;
#2417 = CARTESIAN_POINT ( 'NONE',  ( 8.152565276336593669, 30.35231371789855359, 5.233372021372610483 ) ) ;
#2418 = CARTESIAN_POINT ( 'NONE',  ( 19.68408634441910721, -5.407089921784855591, -9.440624999385555327 ) ) ;
#2419 = AXIS2_PLACEMENT_3D ( 'NONE', #186, #17642, #35053 ) ;
#2420 = CARTESIAN_POINT ( 'NONE',  ( 7.954856959092311719, 102.2273137178985678, -5.529263428287300108 ) ) ;
#2421 = CARTESIAN_POINT ( 'NONE',  ( -27.24356964374999990, 197.5718750006145399, -15.72908226750537786 ) ) ;
#2422 = CARTESIAN_POINT ( 'NONE',  ( 0.1745138560722461762, 142.1898137178985451, 15.50000000000000533 ) ) ;
#2423 = CARTESIAN_POINT ( 'NONE',  ( 10.69584247140445221, 71.64768628210146062, -6.932735513423970097 ) ) ;
#2424 = DIRECTION ( 'NONE',  ( -0.5887012860850800999, 0.8083506638593009885, 0.000000000000000000 ) ) ;
#2425 = DIRECTION ( 'NONE',  ( 0.000000000000000000, -0.000000000000000000, 1.000000000000000000 ) ) ;
#2426 = CARTESIAN_POINT ( 'NONE',  ( 37.56002276824448671, -3.604726614523238837, 167.6449986542055797 ) ) ;
#2427 = CARTESIAN_POINT ( 'NONE',  ( 20.99999999999999289, 242.2374999999999545, -5.999999999999997335 ) ) ;
#2428 = CARTESIAN_POINT ( 'NONE',  ( 22.80587116629411071, 3.604726614523243278, -9.384374999385521221 ) ) ;
#2429 = CARTESIAN_POINT ( 'NONE',  ( 26.99999999999999645, 7.347880794884117764E-16, -6.468749998770951137 ) ) ;
#2430 = AXIS2_PLACEMENT_3D ( 'NONE', #11023, #32038, #6068 ) ;
#2431 = CARTESIAN_POINT ( 'NONE',  ( 0.1745138560725194299, 79.41018628210144925, -9.500000000000005329 ) ) ;
#2432 = FACE_OUTER_BOUND ( 'NONE', #27389, .T. ) ;
#2433 = CARTESIAN_POINT ( 'NONE',  ( 8.715434833791931624, 110.4601862821014606, 8.962234695871760692 ) ) ;
#2434 = CARTESIAN_POINT ( 'NONE',  ( 22.60769515458672885, 248.9674038105676459, -5.999999999999998224 ) ) ;
#2435 = CARTESIAN_POINT ( 'NONE',  ( 19.56230152254410370, 5.196152422706631135, -3.637499998771026810 ) ) ;
#2436 = VERTEX_POINT ( 'NONE', #9755 ) ;
#2437 = CARTESIAN_POINT ( 'NONE',  ( 27.59788244552635206, -5.407089921784859143, 161.2326053007238897 ) ) ;
#2438 = CARTESIAN_POINT ( 'NONE',  ( 15.24356964374999990, 3.323476615752268604, -8.728124999385462601 ) ) ;
#2440 = EDGE_CURVE ( 'NONE', #17126, #14209, #3309, .T. ) ;
#2439 = CARTESIAN_POINT ( 'NONE',  ( -1.045839947578415010E-13, 196.0625000000000284, 27.00000000000000355 ) ) ;
#2441 = CARTESIAN_POINT ( 'NONE',  ( 34.44684893975629336, -5.407089921784861808, 167.8797228278759803 ) ) ;
#2442 = CARTESIAN_POINT ( 'NONE',  ( 37.10248660225891371, 7.347880794884125653E-16, 165.2099845943227479 ) ) ;
#2443 = CARTESIAN_POINT ( 'NONE',  ( 1.069080835302379631E-14, 198.3124999999999716, 27.00000000000000000 ) ) ;
#2444 = CARTESIAN_POINT ( 'NONE',  ( 18.12178482187499640, 241.2343750006145342, -4.985214923628404904 ) ) ;
#2445 = CARTESIAN_POINT ( 'NONE',  ( -27.24356964375000345, 198.9031250006145228, 0.000000000000000000 ) ) ;
#2446 = CARTESIAN_POINT ( 'NONE',  ( -12.50000000000000355, 116.8898137178985621, 0.1745138560722786503 ) ) ;
#2447 = CARTESIAN_POINT ( 'NONE',  ( 11.61527771782819940, 136.3351862821014606, -4.622313124798573369 ) ) ;
#2448 = MECHANICAL_DESIGN_GEOMETRIC_PRESENTATION_REPRESENTATION (  '', ( #13958 ), #24243 ) ;
#2450 = EDGE_LOOP ( 'NONE', ( #21675, #11995 ) ) ;
#2449 = ORIENTED_EDGE ( 'NONE', *, *, #3200, .F. ) ;
#2451 = CARTESIAN_POINT ( 'NONE',  ( 23.87821517812499650, 243.2968750006145058, -4.985214923628404904 ) ) ;
#2452 = EDGE_CURVE ( 'NONE', #25376, #8033, #29837, .T. ) ;
#2453 = DIRECTION ( 'NONE',  ( -0.000000000000000000, 0.000000000000000000, -1.000000000000000000 ) ) ;
#2454 = CARTESIAN_POINT ( 'NONE',  ( -5.770363421894122880, 105.9648137178985650, 14.38691631536194393 ) ) ;
#2455 = DIRECTION ( 'NONE',  ( 0.000000000000000000, 0.000000000000000000, -1.000000000000000000 ) ) ;
#2456 = CARTESIAN_POINT ( 'NONE',  ( 15.24356964375000167, -3.323476615752272600, -1.115624999385467442 ) ) ;
#2457 = CARTESIAN_POINT ( 'NONE',  ( 22.80587116629411426, 7.646167579472024665E-16, -7.621874999385519267 ) ) ;
#2458 = CARTESIAN_POINT ( 'NONE',  ( -20.86978604919638869, 194.8026013911397740, -17.51182792271053046 ) ) ;
#2459 = CARTESIAN_POINT ( 'NONE',  ( -7.228626920339069173, 112.4726862821014493, 10.49813415415989581 ) ) ;
#2460 = CARTESIAN_POINT ( 'NONE',  ( 10.31873187879411091, 3.604726614523236616, -3.328124999385545291 ) ) ;
#2461 = ADVANCED_FACE ( 'NONE', ( #21331 ), #11842, .F. ) ;
#2462 = CARTESIAN_POINT ( 'NONE',  ( -39.50669563604516554, 209.8844732041981729, -8.500000000000003553 ) ) ;
#2463 = CARTESIAN_POINT ( 'NONE',  ( 20.99999999999999645, 243.5593750006144944, 6.646953231504538984 ) ) ;
#2464 = DIRECTION ( 'NONE',  ( -0.000000000000000000, -1.000000000000000000, -0.000000000000000000 ) ) ;
#2465 = CARTESIAN_POINT ( 'NONE',  ( -30.00669563604516554, 209.8844732041982297, -4.499999999999996447 ) ) ;
#2466 = CARTESIAN_POINT ( 'NONE',  ( -2.660918448318275509, 121.0976862821014635, 12.46528703574805874 ) ) ;
#2467 = CARTESIAN_POINT ( 'NONE',  ( 19.56230152254410370, 5.196152422706631135, -3.637499998771026810 ) ) ;
#2468 = CARTESIAN_POINT ( 'NONE',  ( -48.42038769728821990, 208.1428034533959703, 6.469044688360770401 ) ) ;
#2469 = CARTESIAN_POINT ( 'NONE',  ( -56.70466238434235606, 244.2363183625454894, -7.500000000000000000 ) ) ;
#2470 = VECTOR ( 'NONE', #10254, 1000.000000000000000 ) ;
#2471 = CARTESIAN_POINT ( 'NONE',  ( 22.56230152254412147, 7.347880794884125653E-16, -8.775000000000032330 ) ) ;
#2472 = CARTESIAN_POINT ( 'NONE',  ( -11.08355503943142573, 103.5601862821014407, 10.83675517735155402 ) ) ;
#2473 = CARTESIAN_POINT ( 'NONE',  ( -2.311890736173176641, 14.72268628210143859, -12.53471296425194659 ) ) ;
#2474 = ADVANCED_FACE ( 'NONE', ( #32117 ), #1777, .T. ) ;
#2475 = CARTESIAN_POINT ( 'NONE',  ( 22.60769515458672885, 244.5236538117967200, -5.999999999999998224 ) ) ;
#2476 = CARTESIAN_POINT ( 'NONE',  ( -8.152565276336710909, 140.6476862821014322, 5.233372021372435512 ) ) ;
#2477 = CARTESIAN_POINT ( 'NONE',  ( 16.56230152254411081, -7.209453229046475009, -2.278124999385533478 ) ) ;
#2478 = CARTESIAN_POINT ( 'NONE',  ( -0.5000000000000052180, 244.5000000000000000, -11.00000000000000000 ) ) ;
#2479 = ORIENTED_EDGE ( 'NONE', *, *, #2440, .F. ) ;
#2480 = CARTESIAN_POINT ( 'NONE',  ( 25.32464060422194052, 0.000000000000000000, 168.2731477709303363 ) ) ;
#2481 = CARTESIAN_POINT ( 'NONE',  ( 1.715153634034233487, 65.32268628210144357, 9.534712964251941258 ) ) ;
#2482 = CARTESIAN_POINT ( 'NONE',  ( 13.62178482187499640, 195.1531250006145513, -23.59362340125807123 ) ) ;
#2483 = DIRECTION ( 'NONE',  ( 0.000000000000000000, 0.000000000000000000, 1.000000000000000000 ) ) ;
#2484 = CARTESIAN_POINT ( 'NONE',  ( -1.926257025242585782E-15, 195.2468750006145513, -31.45816453501075927 ) ) ;
#2485 = CARTESIAN_POINT ( 'NONE',  ( 2.999999999999997335, 244.5000000000000000, 0.000000000000000000 ) ) ;
#2486 = DIRECTION ( 'NONE',  ( 1.047113545471812582E-14, 0.1163425707149433608, -0.9932091452657082487 ) ) ;
#2487 = CARTESIAN_POINT ( 'NONE',  ( -8.710071997420207879, 33.51481371789854791, 3.796722387233182339 ) ) ;
#2488 = DIRECTION ( 'NONE',  ( -0.000000000000000000, -1.000000000000000000, -0.000000000000000000 ) ) ;
#2489 = ORIENTED_EDGE ( 'NONE', *, *, #31608, .T. ) ;
#2490 = CARTESIAN_POINT ( 'NONE',  ( 15.00000000000000000, 242.4062500012290400, 0.000000000000000000 ) ) ;
#2491 = CARTESIAN_POINT ( 'NONE',  ( -10.49813415416004858, 60.82731371789855501, 7.228626920338840023 ) ) ;
#2492 = CARTESIAN_POINT ( 'NONE',  ( 22.80587116629411781, -3.604726614523238837, -8.109374999385527971 ) ) ;
#2493 = CARTESIAN_POINT ( 'NONE',  ( 23.87821517812499650, 4.985214923628404904, -8.053124999385484983 ) ) ;
#2494 = CARTESIAN_POINT ( 'NONE',  ( -2.311890736173448424, 32.07731371789855501, 12.53471296425189330 ) ) ;
#2495 = AXIS2_PLACEMENT_3D ( 'NONE', #12120, #9663, #15162 ) ;
#2496 = ORIENTED_EDGE ( 'NONE', *, *, #19625, .T. ) ;
#2497 = CARTESIAN_POINT ( 'NONE',  ( 10.31873187879410203, 3.604726614523240613, -1.134374999385481697 ) ) ;
#2498 = CARTESIAN_POINT ( 'NONE',  ( -12.53471296425194836, 12.42268628210144321, 2.311890736173176641 ) ) ;
#2499 = CARTESIAN_POINT ( 'NONE',  ( 37.37045902776835504, 3.604726614523243278, 165.4782751858559777 ) ) ;
#2500 = CARTESIAN_POINT ( 'NONE',  ( -41.09002896937850124, 204.4285982733020433, 3.350049139982171020 ) ) ;
#2501 = DIRECTION ( 'NONE',  ( 1.000000000000000000, 0.000000000000000000, 0.000000000000000000 ) ) ;
#2502 =( NAMED_UNIT ( * ) SI_UNIT ( $, .STERADIAN. ) SOLID_ANGLE_UNIT ( ) );
#2503 = CARTESIAN_POINT ( 'NONE',  ( 15.00000000000000000, 0.000000000000000000, -7.649999999999989697 ) ) ;
#2504 = EDGE_CURVE ( 'NONE', #13411, #31515, #16569, .T. ) ;
#2505 = CARTESIAN_POINT ( 'NONE',  ( -32.58705436395489841, 206.7903428501026042, -3.378800118222489157 ) ) ;
#2506 =( BOUNDED_SURFACE ( )  B_SPLINE_SURFACE ( 1, 2, ( 
 ( #13707, #36433, #4971, #33972, #19780, #1760, #25259, #19222, #1941, #13512, #36621, #10475, #30586, #11037, #30953, #4789, #10663, #33417, #22052, #4602, #16181, #22243, #33606, #7645, #28282, #36808, #27731, #16552, #24697, #16922, #10850, #8013, #10292, #19588, #31137, #36993, #5155, #16735, #2321, #31315, #13892, #25439, #28463, #13143, #36249, #29013, #11965, #34898, #215, #31867, #5522, #20327, #37357, #34707, #8940, #26178, #8754, #26364, #11410, #3057, #17106, #28832, #11780, #34343, #14627, #20516, #20697, #3246, #17480, #23346, #17292, #32054, #25623, #22979, #5900, #2867, #14820, #6084, #11590, #17669, #14440, #25995, #29205, #24, #34528, #6282, #399, #23536, #35081, #2499, #28646, #9131, #32242, #17857, #14073, #37180, #23166, #11221, #8388, #22793, #19957, #31499, #2684, #14259, #25809, #8568, #20135, #31681, #5711, #1343, #18046, #6850, #35458, #32622, #29778, #6660, #15194, #23726, #27313, #9695, #9508, #21084, #12149, #29588, #20889, #35264, #3808, #26741, #23917, #7051, #18425, #32430, #26934, #3433, #33191, #12343, #18234, #26553, #35837, #12724, #15764, #27128, #15384, #964, #12915, #1153, #582, #21271, #30161, #29969, #3998, #24478, #24293, #9879, #32809, #6475, #15572, #775, #24104, #21459, #32999, #35649, #36024, #12540, #18619, #3625, #4190, #10064, #9319, #21639, #7234, #29399, #15001, #34260, #19876, #33567, #5438, #4374, #27689, #37092, #8122, #20054, #31418, #28380, #22896, #19693, #5263, #13989, #31233, #1717, #23077, #17020, #28745, #28559, #18808, #33380, #2600, #2785, #14172, #25726, #25540, #2416, #37279, #24656, #11326, #16840, #11140, #7418, #17206, #34444, #30350, #1528, #5622, #22717, #8304, #21827, #34623, #16138, #24843, #8483, #14359, #25913, #13287, #31599, #37458, #11508, #15953, #36207, #36394, #27506, #13101, #10251, #10440, #18989, #30546, #4563, #22013, #32526, #6001, #35179, #11691, #34997, #17954, #2971, #20799, #15101, #26843, #9415, #23636, #9225, #23444, #32341, #31779, #17581, #26462, #9040, #20991, #6379, #17764, #12252, #20612, #32152, #3345, #6192, #29114, #12445, #29497, #18143, #3536 ),
 ( #26651, #14541, #682, #29305, #14913, #23264, #6569, #23822, #20236, #28936, #29685, #496, #12062, #34808, #24013, #3158, #14728, #35364, #3719, #15291, #26277, #873, #8667, #5814, #17396, #26096, #309, #126, #8853, #20427, #31971, #11875, #35742, #27404, #18899, #7510, #24197, #13012, #4099, #1246, #35930, #12816, #21365, #29875, #33468, #15859, #15670, #27221, #18330, #9788, #27035, #3908, #9972, #32904, #30064, #13198, #24566, #1058, #33099, #9603, #1812, #18526, #24385, #32716, #4469, #30451, #21918, #33286, #21552, #7142, #19084, #7324, #6756, #1436, #36299, #36120, #10160, #30635, #16048, #27595, #21735, #12632, #15480, #1626, #18716, #24750, #6958, #4652, #30255, #10346, #4282, #27785, #16234, #13380, #35559, #21177, #8256, #19276, #25307, #36859, #19829, #2738, #24933, #10904, #22478, #36487, #13761, #16606, #7696, #5026, #31368, #25493, #5391, #28148, #2179, #22107, #28701, #25681, #4840, #31551, #16971, #33656, #25122, #28333, #30816, #34025, #8070, #31006, #16419, #11279, #19646, #10717, #11093, #31188, #5211, #33844, #34211, #2556, #22291, #28513, #16788, #7883, #8436, #2370, #13944, #27966, #19457, #37045, #20005, #22667, #14125, #37231, #22849, #34398, #5575, #10531, #17161, #1996, #13569, #36679, #20188, #20562, #8619, #17531, #14491, #34765, #32293, #5765, #11462, #11827, #3295, #29065, #25863, #32476, #2922, #6333, #17715, #14867, #29449, #6523, #3484, #3109, #18097, #34946, #8992, #9368, #14676, #31737, #23775, #31921, #264, #17345, #448, #26226, #28888, #17905, #14310, #26603, #35313, #32104, #26048, #29637, #23216, #12202, #37412, #23031, #34578, #23398, #75, #6137, #9179, #11640, #8807, #29254, #26413, #20379, #12015, #5952, #23586, #35128, #20748, #15054, #633, #20943, #32853, #826, #7458, #4419, #21129, #10295, #21684, #12393, #3860, #7096, #35508, #4046, #15618, #9744, #23965, #27547, #6903, #26983, #27358, #35879, #18475, #12583, #12961, #18849, #1009, #33236, #9921, #24149, #24700, #27172, #1196, #6709, #35692, #24339, #36252, #21316, #30016, #21505, #7275, #30396, #24519, #3673, #21867, #19037, #33420 ) ),
 .UNSPECIFIED., .F., .F., .F. ) 
 B_SPLINE_SURFACE_WITH_KNOTS ( ( 2, 2 ),
 ( 3, 2, 2, 2, 2, 2, 2, 2, 2, 2, 2, 2, 2, 2, 2, 2, 2, 2, 2, 2, 2, 2, 2, 2, 2, 2, 2, 2, 2, 2, 2, 2, 2, 2, 2, 2, 2, 2, 2, 2, 2, 2, 2, 2, 2, 2, 2, 2, 2, 2, 2, 2, 2, 2, 2, 2, 2, 2, 2, 2, 2, 2, 2, 2, 2, 2, 2, 2, 2, 2, 2, 2, 2, 2, 2, 2, 2, 2, 2, 2, 2, 2, 2, 2, 2, 2, 2, 2, 2, 2, 2, 2, 2, 2, 2, 2, 2, 2, 2, 2, 2, 2, 2, 2, 2, 2, 2, 2, 2, 2, 2, 2, 2, 2, 2, 2, 2, 2, 2, 2, 2, 2, 2, 2, 2, 2, 2, 2, 2, 2, 2, 2, 2, 2, 3 ),
 ( 0.000000000000000000, 1.000000000000000000 ),
 ( 0.000000000000000000, 0.007246376811594202987, 0.01449275362318840597, 0.02173913043478260809, 0.02898550724637681195, 0.03623188405797101580, 0.04347826086956521618, 0.05072463768115942351, 0.05797101449275362389, 0.06521739130434782428, 0.07246376811594203160, 0.07971014492753622505, 0.08695652173913043237, 0.09420289855072463969, 0.1014492753623188470, 0.1086956521739130405, 0.1159420289855072478, 0.1231884057971014551, 0.1304347826086956486, 0.1376811594202898559, 0.1449275362318840632, 0.1521739130434782705, 0.1594202898550724501, 0.1666666666666666574, 0.1739130434782608647, 0.1811594202898550721, 0.1884057971014492794, 0.1956521739130434867, 0.2028985507246376940, 0.2101449275362318736, 0.2173913043478260809, 0.2246376811594202882, 0.2318840579710144956, 0.2391304347826087029, 0.2463768115942029102, 0.2536231884057971175, 0.2608695652173912971, 0.2681159420289855322, 0.2753623188405797118, 0.2826086956521738913, 0.2898550724637681264, 0.2971014492753623060, 0.3043478260869565410, 0.3115942028985507206, 0.3188405797101449002, 0.3260869565217391353, 0.3333333333333333148, 0.3405797101449275499, 0.3478260869565217295, 0.3550724637681159646, 0.3623188405797101441, 0.3695652173913043237, 0.3768115942028985588, 0.3840579710144927383, 0.3913043478260869734, 0.3985507246376811530, 0.4057971014492753881, 0.4130434782608695676, 0.4202898550724637472, 0.4275362318840579823, 0.4347826086956521618, 0.4420289855072463969, 0.4492753623188405765, 0.4565217391304347561, 0.4637681159420289911, 0.4710144927536231707, 0.4782608695652174058, 0.4855072463768115854, 0.4927536231884058204, 0.5000000000000000000, 0.5072463768115942351, 0.5144927536231883591, 0.5217391304347825942, 0.5289855072463768293, 0.5362318840579710644, 0.5434782608695651884, 0.5507246376811594235, 0.5579710144927536586, 0.5652173913043477826, 0.5724637681159420177, 0.5797101449275362528, 0.5869565217391304879, 0.5942028985507246119, 0.6014492753623188470, 0.6086956521739130821, 0.6159420289855072062, 0.6231884057971014412, 0.6304347826086956763, 0.6376811594202898004, 0.6449275362318840354, 0.6521739130434782705, 0.6594202898550725056, 0.6666666666666666297, 0.6739130434782608647, 0.6811594202898550998, 0.6884057971014492239, 0.6956521739130434590, 0.7028985507246376940, 0.7101449275362319291, 0.7173913043478260532, 0.7246376811594202882, 0.7318840579710145233, 0.7391304347826086474, 0.7463768115942028825, 0.7536231884057971175, 0.7608695652173913526, 0.7681159420289854767, 0.7753623188405797118, 0.7826086956521739468, 0.7898550724637680709, 0.7971014492753623060, 0.8043478260869565410, 0.8115942028985507761, 0.8188405797101449002, 0.8260869565217391353, 0.8333333333333333703, 0.8405797101449274944, 0.8478260869565217295, 0.8550724637681159646, 0.8623188405797101996, 0.8695652173913043237, 0.8768115942028985588, 0.8840579710144927938, 0.8913043478260869179, 0.8985507246376811530, 0.9057971014492753881, 0.9130434782608695121, 0.9202898550724637472, 0.9275362318840579823, 0.9347826086956522174, 0.9420289855072463414, 0.9492753623188405765, 0.9565217391304348116, 0.9637681159420289356, 0.9662082944262200268 ),
 .UNSPECIFIED. ) 
 GEOMETRIC_REPRESENTATION_ITEM ( )  RATIONAL_B_SPLINE_SURFACE ( (
 ( 1.000000000000000000, 0.8660254037844387076, 1.000000000000000000, 0.8660254037844387076, 1.000000000000000000, 0.8660254037844387076, 1.000000000000000000, 0.8660254037844387076, 1.000000000000000000, 0.8660254037844387076, 1.000000000000000000, 0.8660254037844387076, 1.000000000000000000, 0.8660254037844387076, 1.000000000000000000, 0.8660254037844387076, 1.000000000000000000, 0.8660254037844387076, 1.000000000000000000, 0.8660254037844387076, 1.000000000000000000, 0.8660254037844387076, 1.000000000000000000, 0.8660254037844387076, 1.000000000000000000, 0.8660254037844387076, 1.000000000000000000, 0.8660254037844387076, 1.000000000000000000, 0.8660254037844387076, 1.000000000000000000, 0.8660254037844387076, 1.000000000000000000, 0.8660254037844387076, 1.000000000000000000, 0.8660254037844387076, 1.000000000000000000, 0.8660254037844387076, 1.000000000000000000, 0.8660254037844387076, 1.000000000000000000, 0.8660254037844387076, 1.000000000000000000, 0.8660254037844387076, 1.000000000000000000, 0.8660254037844387076, 1.000000000000000000, 0.8660254037844387076, 1.000000000000000000, 0.8660254037844387076, 1.000000000000000000, 0.8660254037844387076, 1.000000000000000000, 0.8660254037844387076, 1.000000000000000000, 0.8660254037844387076, 1.000000000000000000, 0.8660254037844387076, 1.000000000000000000, 0.8660254037844387076, 1.000000000000000000, 0.8660254037844387076, 1.000000000000000000, 0.8660254037844387076, 1.000000000000000000, 0.8660254037844387076, 1.000000000000000000, 0.8660254037844387076, 1.000000000000000000, 0.8660254037844387076, 1.000000000000000000, 0.8660254037844387076, 1.000000000000000000, 0.8660254037844387076, 1.000000000000000000, 0.8660254037844387076, 1.000000000000000000, 0.8660254037844387076, 1.000000000000000000, 0.8660254037844387076, 1.000000000000000000, 0.8660254037844387076, 1.000000000000000000, 0.8660254037844387076, 1.000000000000000000, 0.8660254037844387076, 1.000000000000000000, 0.8660254037844387076, 1.000000000000000000, 0.8660254037844387076, 1.000000000000000000, 0.8660254037844387076, 1.000000000000000000, 0.8660254037844387076, 1.000000000000000000, 0.8660254037844387076, 1.000000000000000000, 0.8660254037844387076, 1.000000000000000000, 0.8660254037844387076, 1.000000000000000000, 0.8660254037844387076, 1.000000000000000000, 0.8660254037844387076, 1.000000000000000000, 0.8660254037844387076, 1.000000000000000000, 0.8660254037844387076, 1.000000000000000000, 0.8660254037844387076, 1.000000000000000000, 0.8660254037844387076, 1.000000000000000000, 0.8660254037844387076, 1.000000000000000000, 0.8660254037844387076, 1.000000000000000000, 0.8660254037844387076, 1.000000000000000000, 0.8660254037844387076, 1.000000000000000000, 0.8660254037844387076, 1.000000000000000000, 0.8660254037844387076, 1.000000000000000000, 0.8660254037844387076, 1.000000000000000000, 0.8660254037844387076, 1.000000000000000000, 0.8660254037844387076, 1.000000000000000000, 0.8660254037844387076, 1.000000000000000000, 0.8660254037844387076, 1.000000000000000000, 0.8660254037844387076, 1.000000000000000000, 0.8660254037844387076, 1.000000000000000000, 0.8660254037844387076, 1.000000000000000000, 0.8660254037844387076, 1.000000000000000000, 0.8660254037844387076, 1.000000000000000000, 0.8660254037844387076, 1.000000000000000000, 0.8660254037844387076, 1.000000000000000000, 0.8660254037844387076, 1.000000000000000000, 0.8660254037844387076, 1.000000000000000000, 0.8660254037844387076, 1.000000000000000000, 0.8660254037844387076, 1.000000000000000000, 0.8660254037844387076, 1.000000000000000000, 0.8660254037844387076, 1.000000000000000000, 0.8660254037844387076, 1.000000000000000000, 0.8660254037844387076, 1.000000000000000000, 0.8660254037844387076, 1.000000000000000000, 0.8660254037844387076, 1.000000000000000000, 0.8660254037844387076, 1.000000000000000000, 0.8660254037844387076, 1.000000000000000000, 0.8660254037844387076, 1.000000000000000000, 0.8660254037844387076, 1.000000000000000000, 0.8660254037844387076, 1.000000000000000000, 0.8660254037844387076, 1.000000000000000000, 0.8660254037844387076, 1.000000000000000000, 0.8660254037844387076, 1.000000000000000000, 0.8660254037844387076, 1.000000000000000000, 0.8660254037844387076, 1.000000000000000000, 0.8660254037844387076, 1.000000000000000000, 0.8660254037844387076, 1.000000000000000000, 0.8660254037844387076, 1.000000000000000000, 0.8660254037844387076, 1.000000000000000000, 0.8660254037844387076, 1.000000000000000000, 0.8660254037844387076, 1.000000000000000000, 0.8660254037844387076, 1.000000000000000000, 0.8660254037844387076, 1.000000000000000000, 0.8660254037844387076, 1.000000000000000000, 0.8660254037844387076, 1.000000000000000000, 0.8660254037844387076, 1.000000000000000000, 0.8660254037844387076, 1.000000000000000000, 0.8660254037844387076, 1.000000000000000000, 0.8660254037844387076, 1.000000000000000000, 0.8660254037844387076, 1.000000000000000000, 0.8660254037844387076, 1.000000000000000000, 0.8660254037844387076, 1.000000000000000000, 0.8660254037844387076, 1.000000000000000000, 0.8660254037844387076, 1.000000000000000000, 0.8660254037844387076, 1.000000000000000000, 0.8660254037844387076, 1.000000000000000000, 0.8660254037844387076, 1.000000000000000000, 0.8660254037844387076, 1.000000000000000000, 0.8660254037844387076, 1.000000000000000000, 0.8660254037844387076, 1.000000000000000000, 0.8660254037844387076, 1.000000000000000000, 0.8660254037844387076, 1.000000000000000000, 0.8660254037844387076, 1.000000000000000000, 0.8660254037844387076, 1.000000000000000000, 0.8660254037844387076, 1.000000000000000000, 0.8660254037844387076, 1.000000000000000000, 0.8660254037844387076, 1.000000000000000000, 0.8660254037844387076, 1.000000000000000000, 0.8660254037844387076, 1.000000000000000000, 0.8660254037844387076, 1.000000000000000000, 0.8660254037844387076, 1.000000000000000000, 0.8660254037844387076, 1.000000000000000000, 0.8660254037844387076, 1.000000000000000000, 0.8660254037844387076, 1.000000000000000000, 0.9548847740583508159, 0.9401541683247176540),
 ( 1.000000000000000000, 0.8660254037844387076, 1.000000000000000000, 0.8660254037844387076, 1.000000000000000000, 0.8660254037844387076, 1.000000000000000000, 0.8660254037844387076, 1.000000000000000000, 0.8660254037844387076, 1.000000000000000000, 0.8660254037844387076, 1.000000000000000000, 0.8660254037844387076, 1.000000000000000000, 0.8660254037844387076, 1.000000000000000000, 0.8660254037844387076, 1.000000000000000000, 0.8660254037844387076, 1.000000000000000000, 0.8660254037844387076, 1.000000000000000000, 0.8660254037844387076, 1.000000000000000000, 0.8660254037844387076, 1.000000000000000000, 0.8660254037844387076, 1.000000000000000000, 0.8660254037844387076, 1.000000000000000000, 0.8660254037844387076, 1.000000000000000000, 0.8660254037844387076, 1.000000000000000000, 0.8660254037844387076, 1.000000000000000000, 0.8660254037844387076, 1.000000000000000000, 0.8660254037844387076, 1.000000000000000000, 0.8660254037844387076, 1.000000000000000000, 0.8660254037844387076, 1.000000000000000000, 0.8660254037844387076, 1.000000000000000000, 0.8660254037844387076, 1.000000000000000000, 0.8660254037844387076, 1.000000000000000000, 0.8660254037844387076, 1.000000000000000000, 0.8660254037844387076, 1.000000000000000000, 0.8660254037844387076, 1.000000000000000000, 0.8660254037844387076, 1.000000000000000000, 0.8660254037844387076, 1.000000000000000000, 0.8660254037844387076, 1.000000000000000000, 0.8660254037844387076, 1.000000000000000000, 0.8660254037844387076, 1.000000000000000000, 0.8660254037844387076, 1.000000000000000000, 0.8660254037844387076, 1.000000000000000000, 0.8660254037844387076, 1.000000000000000000, 0.8660254037844387076, 1.000000000000000000, 0.8660254037844387076, 1.000000000000000000, 0.8660254037844387076, 1.000000000000000000, 0.8660254037844387076, 1.000000000000000000, 0.8660254037844387076, 1.000000000000000000, 0.8660254037844387076, 1.000000000000000000, 0.8660254037844387076, 1.000000000000000000, 0.8660254037844387076, 1.000000000000000000, 0.8660254037844387076, 1.000000000000000000, 0.8660254037844387076, 1.000000000000000000, 0.8660254037844387076, 1.000000000000000000, 0.8660254037844387076, 1.000000000000000000, 0.8660254037844387076, 1.000000000000000000, 0.8660254037844387076, 1.000000000000000000, 0.8660254037844387076, 1.000000000000000000, 0.8660254037844387076, 1.000000000000000000, 0.8660254037844387076, 1.000000000000000000, 0.8660254037844387076, 1.000000000000000000, 0.8660254037844387076, 1.000000000000000000, 0.8660254037844387076, 1.000000000000000000, 0.8660254037844387076, 1.000000000000000000, 0.8660254037844387076, 1.000000000000000000, 0.8660254037844387076, 1.000000000000000000, 0.8660254037844387076, 1.000000000000000000, 0.8660254037844387076, 1.000000000000000000, 0.8660254037844387076, 1.000000000000000000, 0.8660254037844387076, 1.000000000000000000, 0.8660254037844387076, 1.000000000000000000, 0.8660254037844387076, 1.000000000000000000, 0.8660254037844387076, 1.000000000000000000, 0.8660254037844387076, 1.000000000000000000, 0.8660254037844387076, 1.000000000000000000, 0.8660254037844387076, 1.000000000000000000, 0.8660254037844387076, 1.000000000000000000, 0.8660254037844387076, 1.000000000000000000, 0.8660254037844387076, 1.000000000000000000, 0.8660254037844387076, 1.000000000000000000, 0.8660254037844387076, 1.000000000000000000, 0.8660254037844387076, 1.000000000000000000, 0.8660254037844387076, 1.000000000000000000, 0.8660254037844387076, 1.000000000000000000, 0.8660254037844387076, 1.000000000000000000, 0.8660254037844387076, 1.000000000000000000, 0.8660254037844387076, 1.000000000000000000, 0.8660254037844387076, 1.000000000000000000, 0.8660254037844387076, 1.000000000000000000, 0.8660254037844387076, 1.000000000000000000, 0.8660254037844387076, 1.000000000000000000, 0.8660254037844387076, 1.000000000000000000, 0.8660254037844387076, 1.000000000000000000, 0.8660254037844387076, 1.000000000000000000, 0.8660254037844387076, 1.000000000000000000, 0.8660254037844387076, 1.000000000000000000, 0.8660254037844387076, 1.000000000000000000, 0.8660254037844387076, 1.000000000000000000, 0.8660254037844387076, 1.000000000000000000, 0.8660254037844387076, 1.000000000000000000, 0.8660254037844387076, 1.000000000000000000, 0.8660254037844387076, 1.000000000000000000, 0.8660254037844387076, 1.000000000000000000, 0.8660254037844387076, 1.000000000000000000, 0.8660254037844387076, 1.000000000000000000, 0.8660254037844387076, 1.000000000000000000, 0.8660254037844387076, 1.000000000000000000, 0.8660254037844387076, 1.000000000000000000, 0.8660254037844387076, 1.000000000000000000, 0.8660254037844387076, 1.000000000000000000, 0.8660254037844387076, 1.000000000000000000, 0.8660254037844387076, 1.000000000000000000, 0.8660254037844387076, 1.000000000000000000, 0.8660254037844387076, 1.000000000000000000, 0.8660254037844387076, 1.000000000000000000, 0.8660254037844387076, 1.000000000000000000, 0.8660254037844387076, 1.000000000000000000, 0.8660254037844387076, 1.000000000000000000, 0.8660254037844387076, 1.000000000000000000, 0.8660254037844387076, 1.000000000000000000, 0.8660254037844387076, 1.000000000000000000, 0.8660254037844387076, 1.000000000000000000, 0.8660254037844387076, 1.000000000000000000, 0.8660254037844387076, 1.000000000000000000, 0.8660254037844387076, 1.000000000000000000, 0.8660254037844387076, 1.000000000000000000, 0.8660254037844387076, 1.000000000000000000, 0.8660254037844387076, 1.000000000000000000, 0.8660254037844387076, 1.000000000000000000, 0.8660254037844387076, 1.000000000000000000, 0.8660254037844387076, 1.000000000000000000, 0.8660254037844387076, 1.000000000000000000, 0.8660254037844387076, 1.000000000000000000, 0.8660254037844387076, 1.000000000000000000, 0.8660254037844387076, 1.000000000000000000, 0.8660254037844387076, 1.000000000000000000, 0.8660254037844387076, 1.000000000000000000, 0.8660254037844387076, 1.000000000000000000, 0.8660254037844387076, 1.000000000000000000, 0.8660254037844387076, 1.000000000000000000, 0.9548847740583508159, 0.9401541683247176540) ) ) 
 REPRESENTATION_ITEM ( '' )  SURFACE ( )  );
#2507 = EDGE_CURVE ( 'NONE', #149, #36238, #24352, .T. ) ;
#2508 = CARTESIAN_POINT ( 'NONE',  ( -39.31622103062156270, 211.6261429550005744, 6.530955311639227823 ) ) ;
#2509 = CARTESIAN_POINT ( 'NONE',  ( 2.999999999999997335, 244.5000000000000000, 5.000000000000000000 ) ) ;
#2510 = ORIENTED_EDGE ( 'NONE', *, *, #29857, .F. ) ;
#2511 = CARTESIAN_POINT ( 'NONE',  ( 1.069080835302379631E-14, 197.9750000012290343, 27.00000000000000000 ) ) ;
#2512 = CARTESIAN_POINT ( 'NONE',  ( 20.99999999999999645, 0.000000000000000000, -8.000000000000000000 ) ) ;
#2513 = CARTESIAN_POINT ( 'NONE',  ( 14.25334919248795451, 19.71481371789854720, -6.092822981423661410 ) ) ;
#2514 = CARTESIAN_POINT ( 'NONE',  ( -33.96502896937850124, 217.3034525342667962, -4.350049139982195001 ) ) ;
#2515 = CARTESIAN_POINT ( 'NONE',  ( 1.715153634034233487, 138.9226862821014663, 9.534712964251941258 ) ) ;
#2516 = VECTOR ( 'NONE', #35484, 1000.000000000000000 ) ;
#2517 = EDGE_CURVE ( 'NONE', #18936, #37055, #3453, .T. ) ;
#2518 = CARTESIAN_POINT ( 'NONE',  ( -6.932735513423968321, 41.74768628210144783, -10.69584247140445221 ) ) ;
#2519 = ADVANCED_FACE ( 'NONE', ( #4986 ), #21698, .T. ) ;
#2520 = CARTESIAN_POINT ( 'NONE',  ( 22.56230152254412502, -3.464101615137755275, -5.662500000000022737 ) ) ;
#2521 = CARTESIAN_POINT ( 'NONE',  ( -14.50000000000000533, 237.0000000000000000, 2.500000000000000000 ) ) ;
#2522 = ORIENTED_EDGE ( 'NONE', *, *, #21319, .F. ) ;
#2523 = CARTESIAN_POINT ( 'NONE',  ( -11.61527771782819940, 140.9351862821014834, 4.622313124798574258 ) ) ;
#2524 = VECTOR ( 'NONE', #12034, 1000.000000000000000 ) ;
#2525 = CARTESIAN_POINT ( 'NONE',  ( -1.045839947578415010E-13, 196.1750000012290229, 27.00000000000000355 ) ) ;
#2526 = CARTESIAN_POINT ( 'NONE',  ( -27.24356964374999990, 197.5718750006145399, -15.72908226750537786 ) ) ;
#2527 = DIRECTION ( 'NONE',  ( 0.000000000000000000, 0.000000000000000000, 1.000000000000000000 ) ) ;
#2528 = CARTESIAN_POINT ( 'NONE',  ( 24.65789917220240213, 0.000000000000000000, 160.6522583305284968 ) ) ;
#2529 = CARTESIAN_POINT ( 'NONE',  ( 26.99999999999999645, 195.7625000000000171, -15.58845726811990495 ) ) ;
#2530 = CARTESIAN_POINT ( 'NONE',  ( 20.99999999999999645, 250.0000000000000000, 5.999999999999999112 ) ) ;
#2531 =( BOUNDED_CURVE ( )  B_SPLINE_CURVE ( 2, ( #12084, #1086, #27060, #1270, #30091, #29707, #24408, #4496, #897 ),
 .UNSPECIFIED., .F., .F. ) 
 B_SPLINE_CURVE_WITH_KNOTS ( ( 3, 2, 2, 2, 3 ),
 ( 0.1847826086956521618, 0.1884057971014492794, 0.1956521739130434867, 0.2028985507246376940, 0.2065217391304347838 ),
 .UNSPECIFIED. ) 
 CURVE ( )  GEOMETRIC_REPRESENTATION_ITEM ( )  RATIONAL_B_SPLINE_CURVE ( ( 0.9330127018922194093, 0.9330127018922190762, 1.000000000000000000, 0.8660254037844387076, 1.000000000000000000, 0.8660254037844387076, 1.000000000000000000, 0.9330127018922194093, 0.9330127018922194093 ) ) 
 REPRESENTATION_ITEM ( '' )  );
#2532 = CARTESIAN_POINT ( 'NONE',  ( 15.24356964375000167, 244.4968750006145228, 3.323476615752272600 ) ) ;
#2533 = CARTESIAN_POINT ( 'NONE',  ( 5.233372021372610483, 110.8523137178985252, -8.152565276336593669 ) ) ;
#2534 = CARTESIAN_POINT ( 'NONE',  ( 26.75643035624999655, 241.5718750006145399, -3.323476615752271268 ) ) ;
#2535 = ORIENTED_EDGE ( 'NONE', *, *, #13434, .T. ) ;
#2536 = CARTESIAN_POINT ( 'NONE',  ( -65.63913769728823411, 206.8500491399821044, -5.686928522499717253 ) ) ;
#2537 = CARTESIAN_POINT ( 'NONE',  ( 7.234628195640295800, 197.0950961906613941, 27.00000000000001066 ) ) ;
#2538 = CARTESIAN_POINT ( 'NONE',  ( 18.00000000000000355, 249.2312500012290570, 5.196152422706632912 ) ) ;
#2539 = CARTESIAN_POINT ( 'NONE',  ( -8.962234695871565293, 118.0398137178985678, -8.715434833792128799 ) ) ;
#2540 = CARTESIAN_POINT ( 'NONE',  ( 13.44051670066911086, 5.407089921784856479, -9.215624999385523708 ) ) ;
#2541 = CARTESIAN_POINT ( 'NONE',  ( 30.75027635825099281, -7.209453229046475009, 161.4461687411947821 ) ) ;
#2542 = CARTESIAN_POINT ( 'NONE',  ( 22.56230152254410370, 0.000000000000000000, -10.00000000000000000 ) ) ;
#2543 = CARTESIAN_POINT ( 'NONE',  ( -26.99999999999998934, 195.9875000000000114, 15.58845726811991561 ) ) ;
#2544 = ORIENTED_EDGE ( 'NONE', *, *, #13634, .T. ) ;
#2545 = ORIENTED_EDGE ( 'NONE', *, *, #19779, .F. ) ;
#2546 = ORIENTED_EDGE ( 'NONE', *, *, #30573, .F. ) ;
#2547 = CARTESIAN_POINT ( 'NONE',  ( 24.00000000000000000, -5.196152422706629359, -7.443749998770954335 ) ) ;
#2548 = CARTESIAN_POINT ( 'NONE',  ( 20.99999999999999645, -6.646953231504538984, -2.728124999385465266 ) ) ;
#2549 = CARTESIAN_POINT ( 'NONE',  ( 19.56230152254412502, -5.196152422706635576, -4.350000000000076028 ) ) ;
#2550 = DIRECTION ( 'NONE',  ( 1.659705900203722642E-32, -2.710505431213758127E-16, -1.000000000000000000 ) ) ;
#2551 = CARTESIAN_POINT ( 'NONE',  ( 26.75643035624999655, 248.1343750006145115, 3.323476615752267715 ) ) ;
#2552 = CARTESIAN_POINT ( 'NONE',  ( -10.69584247140444866, 57.84768628210144925, 6.932735513423972762 ) ) ;
#2553 = PLANE ( 'NONE',  #22436 ) ;
#2554 = CARTESIAN_POINT ( 'NONE',  ( 4.999999999999997335, 215.9999999999999716, 0.1963495407219033040 ) ) ;
#2555 = CARTESIAN_POINT ( 'NONE',  ( -35.94419563604516554, 205.4999999999999716, 0.1155267958017633378 ) ) ;
#2556 = CARTESIAN_POINT ( 'NONE',  ( 36.95867962683237806, 3.464101615137755275, 163.5662633436956810 ) ) ;
#2557 = CARTESIAN_POINT ( 'NONE',  ( 2.311890736173452865, 110.2773137178985650, -12.53471296425189152 ) ) ;
#2558 = CARTESIAN_POINT ( 'NONE',  ( -40.50372103062156981, 216.5309553116391612, -1.626142955000564383 ) ) ;
#2559 = CARTESIAN_POINT ( 'NONE',  ( -44.65997103062156981, 217.3034525342668815, 4.350049139982096413 ) ) ;
#2560 = CARTESIAN_POINT ( 'NONE',  ( 26.75643035624999655, 3.323476615752271268, -3.590624999385492178 ) ) ;
#2561 = CARTESIAN_POINT ( 'NONE',  ( 19.56230152254411436, -5.196152422706629359, -4.237499998771044218 ) ) ;
#2562 = CARTESIAN_POINT ( 'NONE',  ( -2.908627838312453306, 87.27731371789855075, 15.53471296425188797 ) ) ;
#2563 = CARTESIAN_POINT ( 'NONE',  ( -33.96502896937850124, 215.5714017266979567, -3.350049139982168800 ) ) ;
#2564 = ORIENTED_EDGE ( 'NONE', *, *, #9364, .F. ) ;
#2565 = CARTESIAN_POINT ( 'NONE',  ( 36.91619120224290640, 7.347880794884117764E-16, 163.0806184283759706 ) ) ;
#2566 = CARTESIAN_POINT ( 'NONE',  ( 12.46528703574805874, 100.3976862821014464, 2.660918448318279950 ) ) ;
#2567 = CARTESIAN_POINT ( 'NONE',  ( 15.46528703574804986, 72.79768628210145209, 3.257655550457285720 ) ) ;
#2568 = CARTESIAN_POINT ( 'NONE',  ( 16.56230152254410726, 0.000000000000000000, -10.00000000000000000 ) ) ;
#2569 = CARTESIAN_POINT ( 'NONE',  ( 33.91084112185822619, 5.407089921784862696, 161.7531254346117464 ) ) ;
#2570 = CARTESIAN_POINT ( 'NONE',  ( -5.770363421893818234, 60.43518628210146204, -14.38691631536207005 ) ) ;
#2571 =( BOUNDED_CURVE ( )  B_SPLINE_CURVE ( 2, ( #3457, #27152, #12370, #29227, #32263, #20914, #421, #23939, #15026 ),
 .UNSPECIFIED., .F., .F. ) 
 B_SPLINE_CURVE_WITH_KNOTS ( ( 3, 2, 2, 2, 3 ),
 ( 0.6875000000000000000, 0.6944444444444444198, 0.7083333333333333703, 0.7222222222222222099, 0.7291666666666667407 ),
 .UNSPECIFIED. ) 
 CURVE ( )  GEOMETRIC_REPRESENTATION_ITEM ( )  RATIONAL_B_SPLINE_CURVE ( ( 0.9330127018922194093, 0.9330127018922194093, 1.000000000000000000, 0.8660254037844387076, 1.000000000000000000, 0.8660254037844387076, 1.000000000000000000, 0.9330127018922187432, 0.9330127018922192983 ) ) 
 REPRESENTATION_ITEM ( '' )  );
#2572 = CARTESIAN_POINT ( 'NONE',  ( 22.80587116629410360, 7.646167579472015790E-16, -6.665624999385527438 ) ) ;
#2573 = CARTESIAN_POINT ( 'NONE',  ( 1.715153634034233487, 19.32268628210144001, 9.534712964251941258 ) ) ;
#2574 = DIRECTION ( 'NONE',  ( -0.5887012860850800999, 0.8083506638593009885, -0.000000000000000000 ) ) ;
#2575 = CARTESIAN_POINT ( 'NONE',  ( -57.92038769728821990, 208.1428034533959703, 6.469044688360770401 ) ) ;
#2576 = VECTOR ( 'NONE', #17244, 1000.000000000000000 ) ;
#2577 = CARTESIAN_POINT ( 'NONE',  ( 0.000000000000000000, 0.000000000000000000, 0.000000000000000000 ) ) ;
#2578 = CARTESIAN_POINT ( 'NONE',  ( -6.932735513423968321, 50.94768628210144357, -10.69584247140445221 ) ) ;
#2579 = CARTESIAN_POINT ( 'NONE',  ( 26.99999999999999645, 198.0125000000000455, -15.58845726811990495 ) ) ;
#2580 = CARTESIAN_POINT ( 'NONE',  ( 8.710071997420127943, 17.88518628210143646, 3.796722387233375073 ) ) ;
#2581 = CARTESIAN_POINT ( 'NONE',  ( 26.75643035624999655, 248.7718750006145001, -3.323476615752271268 ) ) ;
#2582 = ORIENTED_EDGE ( 'NONE', *, *, #17982, .F. ) ;
#2583 = CARTESIAN_POINT ( 'NONE',  ( 15.00000000000000000, 0.000000000000000000, -5.399999999999987921 ) ) ;
#2584 = CARTESIAN_POINT ( 'NONE',  ( 23.99999999999999645, 243.5499999999999829, -5.196152422706631135 ) ) ;
#2585 = CARTESIAN_POINT ( 'NONE',  ( 27.47531968228746990, -5.407089921784865361, 159.8317065065323845 ) ) ;
#2586 = CARTESIAN_POINT ( 'NONE',  ( 13.44051670066911441, 5.407089921784856479, -2.915624999385552307 ) ) ;
#2587 = CARTESIAN_POINT ( 'NONE',  ( 37.64990212795299840, 3.604726614523238837, 168.6723244366126551 ) ) ;
#2588 = CARTESIAN_POINT ( 'NONE',  ( 15.00000000000000000, 243.2500000000000000, 0.000000000000000000 ) ) ;
#2589 = DIRECTION ( 'NONE',  ( 0.000000000000000000, 0.000000000000000000, 1.000000000000000000 ) ) ;
#2590 = CARTESIAN_POINT ( 'NONE',  ( 2.660918448318279950, 61.29768628210144499, -12.46528703574805874 ) ) ;
#2591 = ORIENTED_EDGE ( 'NONE', *, *, #11969, .F. ) ;
#2592 = ORIENTED_EDGE ( 'NONE', *, *, #17340, .F. ) ;
#2593 = CARTESIAN_POINT ( 'NONE',  ( -27.00000000000000355, 196.9250000012290229, -15.58845726811989429 ) ) ;
#2594 = CARTESIAN_POINT ( 'NONE',  ( 18.00000000000000000, 5.196152422706630247, -4.968749998770949361 ) ) ;
#2595 = CARTESIAN_POINT ( 'NONE',  ( -13.23911966647199812, 34.95231371789854080, -8.632099005475788900 ) ) ;
#2596 = CARTESIAN_POINT ( 'NONE',  ( 18.12178482187499640, 4.985214923628404904, -7.978124999385494576 ) ) ;
#2597 = CARTESIAN_POINT ( 'NONE',  ( 23.87821517812500005, 243.2593750006145399, 4.985214923628404016 ) ) ;
#2598 = CARTESIAN_POINT ( 'NONE',  ( -50.00372103062156981, 214.5309553116392749, -1.090244570138262148 ) ) ;
#2599 = DIRECTION ( 'NONE',  ( 0.000000000000000000, 0.000000000000000000, 1.000000000000000000 ) ) ;
#2600 = CARTESIAN_POINT ( 'NONE',  ( 33.91084112185822619, 5.407089921784862696, 161.7531254346117464 ) ) ;
#2601 = CARTESIAN_POINT ( 'NONE',  ( -7.954856959092309943, 42.42731371789855643, 5.529263428287300108 ) ) ;
#2602 = CARTESIAN_POINT ( 'NONE',  ( 13.44051670066911086, 5.407089921784856479, -9.665624999385530103 ) ) ;
#2603 = CARTESIAN_POINT ( 'NONE',  ( 27.10290335425204233, 195.0000000000000000, -0.6671862432530482057 ) ) ;
#2604 = CARTESIAN_POINT ( 'NONE',  ( -27.24356964374999990, 199.3718750006145513, -15.72908226750537786 ) ) ;
#2605 = CARTESIAN_POINT ( 'NONE',  ( -0.1745138560722763466, 17.98981371789853867, -12.50000000000000355 ) ) ;
#2606 = ORIENTED_EDGE ( 'NONE', *, *, #4345, .F. ) ;
#2607 = CARTESIAN_POINT ( 'NONE',  ( 10.49813415415989581, 64.17268628210143788, 7.228626920339068285 ) ) ;
#2608 = CARTESIAN_POINT ( 'NONE',  ( 25.33444562538816669, 0.000000000000000000, 168.3852196756899957 ) ) ;
#2609 = CARTESIAN_POINT ( 'NONE',  ( 23.99999999999999645, 245.3500000000000227, -5.196152422706631135 ) ) ;
#2610 = CARTESIAN_POINT ( 'NONE',  ( 34.48606902399273366, -5.407089921784861808, 168.3280104420172449 ) ) ;
#2611 = CARTESIAN_POINT ( 'NONE',  ( 24.19849202207515404, 7.686353184319911769, -10.30110366105550135 ) ) ;
#2612 = CARTESIAN_POINT ( 'NONE',  ( 16.56230152254411436, 7.209453229046482114, -9.759374999385554972 ) ) ;
#2613 = DIRECTION ( 'NONE',  ( 0.000000000000000000, 0.000000000000000000, -1.000000000000000000 ) ) ;
#2614 = CARTESIAN_POINT ( 'NONE',  ( 9.500000000000005329, 81.71018628210144641, 0.1745138560725188748 ) ) ;
#2615 = CARTESIAN_POINT ( 'NONE',  ( 22.56230152254410370, 7.347880794884117764E-16, -1.012499998771038134 ) ) ;
#2616 = CARTESIAN_POINT ( 'NONE',  ( -10.49813415415989581, 105.5726862821014578, -7.228626920339068285 ) ) ;
#2617 = CARTESIAN_POINT ( 'NONE',  ( 22.60769515458673595, 249.8674038105676516, -6.000000000000000000 ) ) ;
#2618 = DIRECTION ( 'NONE',  ( -0.000000000000000000, 1.000000000000000000, -0.000000000000000000 ) ) ;
#2619 = ORIENTED_EDGE ( 'NONE', *, *, #17340, .T. ) ;
#2620 = CARTESIAN_POINT ( 'NONE',  ( 27.74168942105997360, 5.407089921784856479, 162.8763265525752786 ) ) ;
#2621 = CARTESIAN_POINT ( 'NONE',  ( 26.75643035624999655, 7.049594010296217766E-16, -6.665624999385472371 ) ) ;
#2622 = CARTESIAN_POINT ( 'NONE',  ( -7.946041369334237991, 195.0000000000000000, 26.05901981062767092 ) ) ;
#2623 = CARTESIAN_POINT ( 'NONE',  ( 25.02561894546576582, 0.000000000000000000, 167.6499628194262357 ) ) ;
#2624 = CARTESIAN_POINT ( 'NONE',  ( 31.19395356112219986, -6.928203230275514990, 166.5174223755558955 ) ) ;
#2625 = CARTESIAN_POINT ( 'NONE',  ( -49.64999999999999858, 244.5000000000000000, -5.000000000000001776 ) ) ;
#2626 = CARTESIAN_POINT ( 'NONE',  ( 26.99999999999999645, 249.7374999999999829, 3.464101615137751278 ) ) ;
#2627 = CARTESIAN_POINT ( 'NONE',  ( -1.926257025242585782E-15, 199.6906250006145456, -31.45816453501076637 ) ) ;
#2628 = CARTESIAN_POINT ( 'NONE',  ( 0.1745138560722779009, 114.5898137178985650, 12.50000000000000355 ) ) ;
#2629 = CARTESIAN_POINT ( 'NONE',  ( -11.61527771782819940, 122.5351862821014635, 4.622313124798574258 ) ) ;
#2631 = VERTEX_POINT ( 'NONE', #27747 ) ;
#2630 = EDGE_LOOP ( 'NONE', ( #9394, #2897, #16899, #8425 ) ) ;
#2632 = CARTESIAN_POINT ( 'NONE',  ( 23.87821517812500005, 241.3468750006145171, 4.985214923628404016 ) ) ;
#2633 = CARTESIAN_POINT ( 'NONE',  ( 19.56230152254412502, -5.196152422706635576, -2.100000000000074252 ) ) ;
#2634 = CARTESIAN_POINT ( 'NONE',  ( 13.04141134922778988, 93.02731371789853654, -8.927990412390371944 ) ) ;
#2635 = CARTESIAN_POINT ( 'NONE',  ( 12.53471296425194836, 90.62268628210146915, -2.311890736173178418 ) ) ;
#2636 = EDGE_CURVE ( 'NONE', #407, #26185, #30970, .T. ) ;
#2637 = CARTESIAN_POINT ( 'NONE',  ( 21.00000000000000000, -6.646953231504538984, -2.840624999385488181 ) ) ;
#2638 = SHAPE_REPRESENTATION ( 'handle', ( #17215 ), #15973 ) ;
#2639 = CARTESIAN_POINT ( 'NONE',  ( -13.50000000000000533, 197.3375000012290457, -23.38268590217984411 ) ) ;
#2640 = CARTESIAN_POINT ( 'NONE',  ( -12.50000000000000355, 113.9101862821014493, -0.1745138560725492671 ) ) ;
#2641 = CARTESIAN_POINT ( 'NONE',  ( 22.80587116629410716, 7.646167579472015790E-16, -3.065624999385535787 ) ) ;
#2642 = EDGE_CURVE ( 'NONE', #34685, #32085, #8558, .T. ) ;
#2643 = CARTESIAN_POINT ( 'NONE',  ( 15.24356964375000167, 243.4843750006145058, 3.323476615752272600 ) ) ;
#2644 = CARTESIAN_POINT ( 'NONE',  ( 26.99999999999999645, 7.347880794884117764E-16, -2.925000000000010925 ) ) ;
#2645 = CARTESIAN_POINT ( 'NONE',  ( -54.15252896937850124, 206.6499508600178387, -5.571401726697954970 ) ) ;
#2646 = CARTESIAN_POINT ( 'NONE',  ( -12.50000000000000355, 113.9101862821014493, -0.1745138560725492671 ) ) ;
#2647 = CARTESIAN_POINT ( 'NONE',  ( 16.56230152254410726, 6.928203230275506996, -3.599999998771000520 ) ) ;
#2648 = CARTESIAN_POINT ( 'NONE',  ( -40.30580436395489841, 216.5000000000000000, 0.1155267958017343610 ) ) ;
#2649 = CARTESIAN_POINT ( 'NONE',  ( 20.99999999999999645, 0.000000000000000000, -8.000000000000000000 ) ) ;
#2650 = CARTESIAN_POINT ( 'NONE',  ( -7.234628195640302017, 198.8549038117967029, 27.00000000000000711 ) ) ;
#2651 = CARTESIAN_POINT ( 'NONE',  ( -13.04141134922759804, 96.37268628210144072, -8.927990412390657937 ) ) ;
#2652 = EDGE_CURVE ( 'NONE', #21280, #24290, #22616, .T. ) ;
#2653 = CARTESIAN_POINT ( 'NONE',  ( -6.932735513423968321, 23.34768628210144570, -10.69584247140445221 ) ) ;
#2654 = LINE ( 'NONE', #3216, #27316 ) ;
#2655 = CARTESIAN_POINT ( 'NONE',  ( 14.99999999999989697, -3.464101615137695767, -2.606249998770969523 ) ) ;
#2656 = CARTESIAN_POINT ( 'NONE',  ( -2.064181346179269738, 139.4976862821014549, 9.465287035748067623 ) ) ;
#2657 = CARTESIAN_POINT ( 'NONE',  ( 16.56230152254411436, 7.209453229046475009, -2.503124999385547778 ) ) ;
#2658 = CARTESIAN_POINT ( 'NONE',  ( 25.01527935017339033, 0.000000000000000000, 50.00000000000000000 ) ) ;
#2659 = ORIENTED_EDGE ( 'NONE', *, *, #22083, .T. ) ;
#2660 = CARTESIAN_POINT ( 'NONE',  ( 37.60414536301047406, -3.604726614523235284, 168.1493222201144988 ) ) ;
#2661 = MECHANICAL_DESIGN_GEOMETRIC_PRESENTATION_REPRESENTATION (  '', ( #35945 ), #19635 ) ;
#2662 = CARTESIAN_POINT ( 'NONE',  ( 6.840914352312096547, 62.16018628210144925, -6.594114490232313663 ) ) ;
#2663 = AXIS2_PLACEMENT_3D ( 'NONE', #6384, #14544, #17209 ) ;
#2664 = CARTESIAN_POINT ( 'NONE',  ( 22.60769515458672885, 243.8888461906613543, 5.999999999999997335 ) ) ;
#2665 = CARTESIAN_POINT ( 'NONE',  ( -20.86978606573367045, 194.8588513912095266, -17.51182790300216752 ) ) ;
#2666 = FACE_OUTER_BOUND ( 'NONE', #17186, .T. ) ;
#2667 = CARTESIAN_POINT ( 'NONE',  ( -13.62178482187498396, 195.8843750006145399, 23.59362340125808188 ) ) ;
#2668 = DIRECTION ( 'NONE',  ( 0.000000000000000000, 0.000000000000000000, -1.000000000000000000 ) ) ;
#2669 = VECTOR ( 'NONE', #5948, 1000.000000000000000 ) ;
#2670 = DIRECTION ( 'NONE',  ( 1.000000000000000000, 0.000000000000000000, 0.000000000000000000 ) ) ;
#2671 = CARTESIAN_POINT ( 'NONE',  ( -8.152565276336593669, 34.95231371789854080, -5.233372021372610483 ) ) ;
#2672 = CARTESIAN_POINT ( 'NONE',  ( 13.62178482187501416, 198.6593750006145456, 23.59362340125806767 ) ) ;
#2673 = ORIENTED_EDGE ( 'NONE', *, *, #581, .F. ) ;
#2674 = VERTEX_POINT ( 'NONE', #1959 ) ;
#2675 = CARTESIAN_POINT ( 'NONE',  ( 26.75643035624999655, 249.0718750006145115, -7.049594010296217766E-16 ) ) ;
#2676 = CARTESIAN_POINT ( 'NONE',  ( 2.311890736173452421, 45.87731371789855217, -12.53471296425189152 ) ) ;
#2677 = CARTESIAN_POINT ( 'NONE',  ( 10.31873187879410736, 0.000000000000000000, -8.296874999385501326 ) ) ;
#2678 = CARTESIAN_POINT ( 'NONE',  ( 26.75643035624999655, -3.323476615752267715, -9.515624999385494220 ) ) ;
#2679 = CARTESIAN_POINT ( 'NONE',  ( -11.48171059495408208, 15.11481371789855110, 4.944772684328421875 ) ) ;
#2680 = VERTEX_POINT ( 'NONE', #35055 ) ;
#2681 = CARTESIAN_POINT ( 'NONE',  ( 10.31873187879410736, -3.604726614523244610, -1.509374999385515670 ) ) ;
#2682 = CARTESIAN_POINT ( 'NONE',  ( -12.50000000000000355, 3.510186282101451560, -0.1745138560725492671 ) ) ;
#2683 = EDGE_CURVE ( 'NONE', #6822, #28262, #9292, .T. ) ;
#2684 = CARTESIAN_POINT ( 'NONE',  ( 37.32797060317886917, 7.646167579472024665E-16, 164.9926302705362957 ) ) ;
#2685 = CARTESIAN_POINT ( 'NONE',  ( -37.92336230271182984, 215.6869285224997270, 3.149950860017831200 ) ) ;
#2686 = DIRECTION ( 'NONE',  ( -0.000000000000000000, -1.000000000000000000, -0.000000000000000000 ) ) ;
#2687 =( NAMED_UNIT ( * ) PLANE_ANGLE_UNIT ( ) SI_UNIT ( $, .RADIAN. ) );
#2688 = CARTESIAN_POINT ( 'NONE',  ( -18.84057396323613176, 195.0000000000000000, 19.60903927252854118 ) ) ;
#2689 = CARTESIAN_POINT ( 'NONE',  ( -59.29836230271182984, 206.0451222850691977, -2.149950860017851184 ) ) ;
#2690 = CARTESIAN_POINT ( 'NONE',  ( -42.08705436395489841, 205.3262412349647263, -4.842901733360204020 ) ) ;
#2691 = CARTESIAN_POINT ( 'NONE',  ( 25.22335353682449721, 3.604726614523236616, 169.9100795407218811 ) ) ;
#2692 = ORIENTED_EDGE ( 'NONE', *, *, #1304, .T. ) ;
#2693 = CARTESIAN_POINT ( 'NONE',  ( 22.56230152254411792, 7.347880794884125653E-16, -4.725000000000035172 ) ) ;
#2694 = CARTESIAN_POINT ( 'NONE',  ( 25.32464060422194052, 0.000000000000000000, 168.2731477709303363 ) ) ;
#2695 = CARTESIAN_POINT ( 'NONE',  ( 10.83675517735179206, 28.33981371789855430, -11.08355503943118769 ) ) ;
#2696 = CARTESIAN_POINT ( 'NONE',  ( -34.16294563604517265, 216.1378603801729241, -6.307003348498026796 ) ) ;
#2697 = CARTESIAN_POINT ( 'NONE',  ( -12.50000000000000355, 12.71018628210143753, -0.1745138560725492671 ) ) ;
#2698 = CARTESIAN_POINT ( 'NONE',  ( -12.53471296425194836, 40.02268628210143930, 2.311890736173176641 ) ) ;
#2699 = CARTESIAN_POINT ( 'NONE',  ( 10.56230152254410548, 0.000000000000000000, -4.050000000000054001 ) ) ;
#2700 = VERTEX_POINT ( 'NONE', #28299 ) ;
#2701 = CARTESIAN_POINT ( 'NONE',  ( -13.50000000000000533, 198.6875000012290400, -23.38268590217984411 ) ) ;
#2702 = CARTESIAN_POINT ( 'NONE',  ( 13.62178482187499640, 196.1093750006145342, -23.59362340125807123 ) ) ;
#2703 = PLANE ( 'NONE',  #2042 ) ;
#2704 = CARTESIAN_POINT ( 'NONE',  ( -27.00000000000000355, 198.6125000000000114, -15.58845726811989429 ) ) ;
#2705 = DIRECTION ( 'NONE',  ( -1.000000000000000000, 0.000000000000000000, 0.000000000000000000 ) ) ;
#2706 = CARTESIAN_POINT ( 'NONE',  ( -81.00000000000002842, 206.0000000000000000, 2.500000000000002220 ) ) ;
#2707 = ADVANCED_FACE ( 'NONE', ( #11238, #6257, #19795 ), #37195, .F. ) ;
#2708 = CARTESIAN_POINT ( 'NONE',  ( 15.24356964375000167, 245.8468750006145171, 3.323476615752272600 ) ) ;
#2709 = CARTESIAN_POINT ( 'NONE',  ( -8.152565276336593669, 99.35231371789856780, -5.233372021372610483 ) ) ;
#2710 = CARTESIAN_POINT ( 'NONE',  ( 20.99999999999999645, 240.9718750006145456, 6.646953231504538984 ) ) ;
#2711 = VERTEX_POINT ( 'NONE', #28480 ) ;
#2712 = DIRECTION ( 'NONE',  ( 0.000000000000000000, 0.000000000000000000, 1.000000000000000000 ) ) ;
#2713 = CARTESIAN_POINT ( 'NONE',  ( -26.99999999999999645, 195.9875000000000114, 15.58845726811991561 ) ) ;
#2714 = CARTESIAN_POINT ( 'NONE',  ( 21.00000000000000000, 245.6687500012290570, 6.928203230275506996 ) ) ;
#2715 = ORIENTED_EDGE ( 'NONE', *, *, #2992, .F. ) ;
#2716 = CARTESIAN_POINT ( 'NONE',  ( -0.1745138560722763466, 109.9898137178985706, -12.50000000000000355 ) ) ;
#2717 = CARTESIAN_POINT ( 'NONE',  ( 22.80587116629411781, -3.604726614523238837, -0.9093749993854999270 ) ) ;
#2718 = CARTESIAN_POINT ( 'NONE',  ( 24.48470861703815515, -3.604726614523240613, 161.4673294743943188 ) ) ;
#2719 = VECTOR ( 'NONE', #15417, 1000.000000000000000 ) ;
#2720 = CARTESIAN_POINT ( 'NONE',  ( 15.24356964375000167, -3.323476615752272600, -1.115624999385467442 ) ) ;
#2721 = CARTESIAN_POINT ( 'NONE',  ( 4.944772684328420986, 58.81481371789855217, 11.48171059495408208 ) ) ;
#2722 = CARTESIAN_POINT ( 'NONE',  ( 13.50000000000001421, 196.1000000000000227, 23.38268590217984055 ) ) ;
#2723 = ORIENTED_EDGE ( 'NONE', *, *, #30417, .T. ) ;
#2724 = AXIS2_PLACEMENT_3D ( 'NONE', #10371, #33121, #18923 ) ;
#2725 = ORIENTED_EDGE ( 'NONE', *, *, #34443, .F. ) ;
#2726 = ORIENTED_EDGE ( 'NONE', *, *, #14588, .T. ) ;
#2727 = CARTESIAN_POINT ( 'NONE',  ( 26.99999999999999645, -3.464101615137751278, -6.506249998770941900 ) ) ;
#2728 = CARTESIAN_POINT ( 'NONE',  ( 15.24356964374999990, 3.323476615752268604, -2.428124999385457006 ) ) ;
#2729 = CARTESIAN_POINT ( 'NONE',  ( -77.00000000000002842, 210.0000000000000000, -2.499999999999998668 ) ) ;
#2730 = CARTESIAN_POINT ( 'NONE',  ( 19.00081571707366379, 5.492723647597353320, -10.12707781181608979 ) ) ;
#2731 = CARTESIAN_POINT ( 'NONE',  ( -7.228626920339069173, 57.27268628210144641, 10.49813415415989581 ) ) ;
#2732 = EDGE_CURVE ( 'NONE', #10880, #4926, #27922, .T. ) ;
#2733 =( BOUNDED_CURVE ( )  B_SPLINE_CURVE ( 3, ( #31686, #26557, #585, #12155 ),
 .UNSPECIFIED., .F., .F. ) 
 B_SPLINE_CURVE_WITH_KNOTS ( ( 4, 4 ),
 ( 3.141592653589793116, 6.283185307179586232 ),
 .UNSPECIFIED. ) 
 CURVE ( )  GEOMETRIC_REPRESENTATION_ITEM ( )  RATIONAL_B_SPLINE_CURVE ( ( 1.000000000000000000, 0.3333333333333333703, 0.3333333333333333703, 1.000000000000000000 ) ) 
 REPRESENTATION_ITEM ( '' )  );
#2734 = CARTESIAN_POINT ( 'NONE',  ( -54.15252896937850124, 206.6499508600178387, -5.571401726697954970 ) ) ;
#2735 = CARTESIAN_POINT ( 'NONE',  ( 17.03503949639525317, 220.5732280096082150, -4.520320870633828036 ) ) ;
#2736 = ADVANCED_FACE ( 'NONE', ( #14977 ), #32026, .F. ) ;
#2737 = CARTESIAN_POINT ( 'NONE',  ( -40.89211230271183695, 205.5309553116392465, 1.321298161741817356 ) ) ;
#2738 = CARTESIAN_POINT ( 'NONE',  ( 37.07633987954171317, 3.464101615137755275, 164.9111261861195601 ) ) ;
#2739 = CARTESIAN_POINT ( 'NONE',  ( -12.46528703574811558, 98.20231371789856212, 2.660918448318003726 ) ) ;
#2740 = CARTESIAN_POINT ( 'NONE',  ( -33.77455436395490551, 205.1570982666397356, 4.673758765035198159 ) ) ;
#2741 = CARTESIAN_POINT ( 'NONE',  ( -45.64955436395490551, 216.3070033484980002, -6.137860380172975638 ) ) ;
#2742 = CARTESIAN_POINT ( 'NONE',  ( 23.87821517812500005, -4.985214923628404016, -3.703124999385493332 ) ) ;
#2743 = CARTESIAN_POINT ( 'NONE',  ( 15.53471296425188797, 84.97731371789856780, 2.908627838312457747 ) ) ;
#2744 = CARTESIAN_POINT ( 'NONE',  ( -35.35044563604516554, 205.1570982666397072, -4.673758765035155527 ) ) ;
#2745 = AXIS2_PLACEMENT_3D ( 'NONE', #12131, #34882, #9488 ) ;
#2746 = VERTEX_POINT ( 'NONE', #16751 ) ;
#2747 = DIRECTION ( 'NONE',  ( -0.1219804832088935975, -0.9925324990730152175, 0.000000000000000000 ) ) ;
#2748 = CARTESIAN_POINT ( 'NONE',  ( 10.69584247140445221, 108.4476862821014578, -6.932735513423970097 ) ) ;
#2749 = CARTESIAN_POINT ( 'NONE',  ( -6.092822981423970496, 38.58518628210143930, 14.25334919248782661 ) ) ;
#2750 = VECTOR ( 'NONE', #5758, 1000.000000000000000 ) ;
#2751 = DIRECTION ( 'NONE',  ( 0.000000000000000000, 0.000000000000000000, -1.000000000000000000 ) ) ;
#2752 =( BOUNDED_CURVE ( )  B_SPLINE_CURVE ( 2, ( #3093, #17700, #34931, #3280, #8976, #14661, #11625, #23200, #20925 ),
 .UNSPECIFIED., .F., .F. ) 
 B_SPLINE_CURVE_WITH_KNOTS ( ( 3, 2, 2, 2, 3 ),
 ( 0.2708333333333333703, 0.2777777777777777901, 0.2916666666666666852, 0.3055555555555555802, 0.3125000000000000000 ),
 .UNSPECIFIED. ) 
 CURVE ( )  GEOMETRIC_REPRESENTATION_ITEM ( )  RATIONAL_B_SPLINE_CURVE ( ( 0.9330127018922194093, 0.9330127018922196314, 1.000000000000000000, 0.8660254037844387076, 1.000000000000000000, 0.8660254037844387076, 1.000000000000000000, 0.9330127018922194093, 0.9330127018922194093 ) ) 
 REPRESENTATION_ITEM ( '' )  );
#2753 = CARTESIAN_POINT ( 'NONE',  ( 37.09591843811324452, 3.604726614523243278, 162.3402618868670118 ) ) ;
#2754 = CARTESIAN_POINT ( 'NONE',  ( -15.53471296425195369, 58.42268628210145209, 2.908627838312118019 ) ) ;
#2755 = CARTESIAN_POINT ( 'NONE',  ( 19.68408634441910721, -5.407089921784855591, -9.440624999385555327 ) ) ;
#2756 = DIRECTION ( 'NONE',  ( 0.000000000000000000, 0.000000000000000000, 1.000000000000000000 ) ) ;
#2757 = CARTESIAN_POINT ( 'NONE',  ( -50.99330436395489841, 210.1155267958017134, -6.500000000000000888 ) ) ;
#2758 = CARTESIAN_POINT ( 'NONE',  ( 18.00000000000000355, 243.3812500012290343, 5.196152422706632912 ) ) ;
#2759 = CARTESIAN_POINT ( 'NONE',  ( -12.46528703574805697, 40.59768628210144215, -2.660918448318280838 ) ) ;
#2760 = CARTESIAN_POINT ( 'NONE',  ( 27.00000000000001066, 197.4875000000000114, 15.58845726811988897 ) ) ;
#2761 = CARTESIAN_POINT ( 'NONE',  ( -27.00000000000000355, 197.8625000012290513, 0.000000000000000000 ) ) ;
#2762 = CARTESIAN_POINT ( 'NONE',  ( -8.710071997420127943, 13.28518628210143149, -3.796722387233380402 ) ) ;
#2763 = CARTESIAN_POINT ( 'NONE',  ( 15.24356964375000167, 248.0968750006145456, 3.323476615752272600 ) ) ;
#2764 = ORIENTED_EDGE ( 'NONE', *, *, #13312, .F. ) ;
#2765 = CARTESIAN_POINT ( 'NONE',  ( 26.99999999999999645, 7.347880794884117764E-16, -4.275000000000001243 ) ) ;
#2766 = DIRECTION ( 'NONE',  ( 0.000000000000000000, 0.000000000000000000, 1.000000000000000000 ) ) ;
#2767 = CARTESIAN_POINT ( 'NONE',  ( 36.89654967657799745, 7.646167579472024665E-16, 160.0614665149821576 ) ) ;
#2768 = CARTESIAN_POINT ( 'NONE',  ( 13.44051670066911619, -5.407089921784859143, -5.465624999385548577 ) ) ;
#2769 = CARTESIAN_POINT ( 'NONE',  ( 24.61867908796596183, 0.000000000000000000, 160.2039707163872038 ) ) ;
#2770 = CARTESIAN_POINT ( 'NONE',  ( 21.00000000000000000, 240.8875000000000171, -6.928203230275506996 ) ) ;
#2771 = EDGE_CURVE ( 'NONE', #31898, #11836, #30370, .T. ) ;
#2772 = FACE_OUTER_BOUND ( 'NONE', #7674, .T. ) ;
#2773 = CARTESIAN_POINT ( 'NONE',  ( -4.622313124798576922, 69.63518628210145778, -11.61527771782819762 ) ) ;
#2774 = ORIENTED_EDGE ( 'NONE', *, *, #260, .F. ) ;
#2775 = VERTEX_POINT ( 'NONE', #5174 ) ;
#2776 = CARTESIAN_POINT ( 'NONE',  ( 30.95863305570354029, -6.928203230275514990, 163.8276966907082226 ) ) ;
#2777 = CARTESIAN_POINT ( 'NONE',  ( 13.49999999999999645, 195.9125000012290343, -23.38268590217984766 ) ) ;
#2778 = CARTESIAN_POINT ( 'NONE',  ( 27.00000000000036593, 3.464101615137540779, -5.081249998770964282 ) ) ;
#2779 = CARTESIAN_POINT ( 'NONE',  ( -13.23911966647199812, 44.15231371789854364, -8.632099005475788900 ) ) ;
#2780 = ADVANCED_FACE ( 'NONE', ( #20488 ), #35241, .F. ) ;
#2781 = CARTESIAN_POINT ( 'NONE',  ( 0.000000000000000000, 2.000000000000000000, -5.000000000000000000 ) ) ;
#2782 = CARTESIAN_POINT ( 'NONE',  ( 23.87821517812500005, 243.7093750006145285, 4.985214923628404016 ) ) ;
#2783 = CARTESIAN_POINT ( 'NONE',  ( -47.43080436395489841, 205.4999999999999716, -0.1155267958017894420 ) ) ;
#2784 = CARTESIAN_POINT ( 'NONE',  ( 5.499999999999994671, 244.5000000000000000, 0.000000000000000000 ) ) ;
#2785 = CARTESIAN_POINT ( 'NONE',  ( 37.01747826964035681, 3.604726614523243278, 161.4436866585844541 ) ) ;
#2786 = CARTESIAN_POINT ( 'NONE',  ( 6.840914352311949109, 12.23981371789853512, 6.594114490232462877 ) ) ;
#2787 = CARTESIAN_POINT ( 'NONE',  ( -69.39955436395486288, 214.8429017333601792, -4.673758765035196383 ) ) ;
#2788 = DIRECTION ( 'NONE',  ( -2.775557561562891351E-17, 0.000000000000000000, 1.000000000000000000 ) ) ;
#2789 = CARTESIAN_POINT ( 'NONE',  ( 17.55485740163879527, 195.0000000000000000, 20.80657516995691836 ) ) ;
#2790 = CARTESIAN_POINT ( 'NONE',  ( -13.62178482187498396, 196.3343750006145285, 23.59362340125808188 ) ) ;
#2791 = CARTESIAN_POINT ( 'NONE',  ( -8.927990412390371944, 127.5273137178985792, -13.04141134922778988 ) ) ;
#2792 =( BOUNDED_CURVE ( )  B_SPLINE_CURVE ( 2, ( #25036, #28068, #36593, #19750, #10633, #31109, #13862, #25410, #22580 ),
 .UNSPECIFIED., .F., .F. ) 
 B_SPLINE_CURVE_WITH_KNOTS ( ( 3, 2, 2, 2, 3 ),
 ( 0.06250000000000000000, 0.06944444444444444753, 0.08333333333333332871, 0.09722222222222222376, 0.1041666666666666713 ),
 .UNSPECIFIED. ) 
 CURVE ( )  GEOMETRIC_REPRESENTATION_ITEM ( )  RATIONAL_B_SPLINE_CURVE ( ( 0.9330127018922194093, 0.9330127018922194093, 1.000000000000000000, 0.8660254037844387076, 1.000000000000000000, 0.8660254037844387076, 1.000000000000000000, 0.9330127018922192983, 0.9330127018922194093 ) ) 
 REPRESENTATION_ITEM ( '' )  );
#2793 = VECTOR ( 'NONE', #22023, 1000.000000000000000 ) ;
#2794 = ORIENTED_EDGE ( 'NONE', *, *, #25444, .T. ) ;
#2795 = CARTESIAN_POINT ( 'NONE',  ( -0.1745138560725500443, 38.01018628210144357, 12.50000000000000355 ) ) ;
#2796 = CARTESIAN_POINT ( 'NONE',  ( -4.694659320240884604E-14, 197.8625000000000114, 27.00000000000000000 ) ) ;
#2797 = LINE ( 'NONE', #14369, #8396 ) ;
#2798 = CARTESIAN_POINT ( 'NONE',  ( 36.82301201863464968, 7.646167579472015790E-16, 159.2209272384671976 ) ) ;
#2799 = CARTESIAN_POINT ( 'NONE',  ( 24.00000000000000000, -5.196152422706629359, -2.043749998770966414 ) ) ;
#2800 = CARTESIAN_POINT ( 'NONE',  ( 16.56230152254411436, 7.209453229046482114, -8.859374999385529748 ) ) ;
#2801 = CARTESIAN_POINT ( 'NONE',  ( 24.62194742831963623, -3.464101615138128754, 160.2413280175655643 ) ) ;
#2802 = CARTESIAN_POINT ( 'NONE',  ( 7.954856959092191815, 73.37268628210144072, 5.529263428287477744 ) ) ;
#2803 = CARTESIAN_POINT ( 'NONE',  ( 0.000000000000000000, 210.0000000000000284, 0.000000000000000000 ) ) ;
#2804 = AXIS2_PLACEMENT_3D ( 'NONE', #21586, #33689, #2032 ) ;
#2805 = CARTESIAN_POINT ( 'NONE',  ( 12.50000000000000355, 90.91018628210146346, 0.1745138560725507937 ) ) ;
#2806 = LINE ( 'NONE', #8687, #33009 ) ;
#2807 = CARTESIAN_POINT ( 'NONE',  ( -7.234628195640302017, 195.2549038117967086, 27.00000000000000711 ) ) ;
#2808 = ORIENTED_EDGE ( 'NONE', *, *, #7091, .T. ) ;
#2809 = CARTESIAN_POINT ( 'NONE',  ( 36.98316069593345645, 3.604726614523238837, 161.0514349962108156 ) ) ;
#2810 = CARTESIAN_POINT ( 'NONE',  ( 18.12178482187499640, 4.985214923628404904, -6.965624999385466865 ) ) ;
#2811 = CARTESIAN_POINT ( 'NONE',  ( -27.24356964375000345, 195.3218750006145399, -15.72908226750537786 ) ) ;
#2812 = CARTESIAN_POINT ( 'NONE',  ( 25.02235060511272735, 3.604726614523240613, 167.6126055182477614 ) ) ;
#2813 = CARTESIAN_POINT ( 'NONE',  ( 28.14980768084533125, 5.196152422706636465, 166.1438154837653656 ) ) ;
#2814 = DIRECTION ( 'NONE',  ( 0.000000000000000000, 0.000000000000000000, 1.000000000000000000 ) ) ;
#2815 = CARTESIAN_POINT ( 'NONE',  ( 21.00000000000000000, 240.9718750006145456, 6.646953231504538984 ) ) ;
#2816 = CARTESIAN_POINT ( 'NONE',  ( 5.778771075727756162E-15, 199.0156250006145342, 31.45816453501076637 ) ) ;
#2817 = CARTESIAN_POINT ( 'NONE',  ( 8.715434833792128799, 120.3398137178985650, -8.962234695871567070 ) ) ;
#2818 = CARTESIAN_POINT ( 'NONE',  ( -4.622313124798576922, 124.8351862821014748, -11.61527771782819762 ) ) ;
#2820 = EDGE_LOOP ( 'NONE', ( #232, #22651, #21479, #3234 ) ) ;
#2819 = ORIENTED_EDGE ( 'NONE', *, *, #13347, .T. ) ;
#2821 = CARTESIAN_POINT ( 'NONE',  ( 5.778771075727756162E-15, 197.2156250006145513, 31.45816453501075927 ) ) ;
#2822 = CARTESIAN_POINT ( 'NONE',  ( 18.12178482187499640, 241.1218750006145228, -4.985214923628404904 ) ) ;
#2823 = CARTESIAN_POINT ( 'NONE',  ( 15.00000000000000000, 0.000000000000000000, -2.700000000000008171 ) ) ;
#2824 = CARTESIAN_POINT ( 'NONE',  ( -10.83675517735179028, 97.33981371789856496, 11.08355503943118947 ) ) ;
#2825 = CARTESIAN_POINT ( 'NONE',  ( 26.75643035624999655, 3.323476615752271712, -1.790624999385476812 ) ) ;
#2826 = CARTESIAN_POINT ( 'NONE',  ( 27.00000000000001066, 197.1500000012290172, 15.58845726811988897 ) ) ;
#2827 = CARTESIAN_POINT ( 'NONE',  ( 5.529263428287300108, 76.92731371789854222, 7.954856959092309943 ) ) ;
#2828 = CARTESIAN_POINT ( 'NONE',  ( 16.56230152254411081, -7.209453229046475009, -3.628124999385553107 ) ) ;
#2829 = CARTESIAN_POINT ( 'NONE',  ( 23.87821517812500005, 242.6968750006145115, 4.985214923628404016 ) ) ;
#2830 = CARTESIAN_POINT ( 'NONE',  ( -10.49813415416004858, 70.02731371789855075, 7.228626920338839135 ) ) ;
#2831 = VECTOR ( 'NONE', #373, 1000.000000000000000 ) ;
#2832 = CARTESIAN_POINT ( 'NONE',  ( 22.60769515458672885, 240.2325961894323143, 5.999999999999997335 ) ) ;
#2833 = CARTESIAN_POINT ( 'NONE',  ( -0.1745138560725500443, 111.6101862821014521, 12.50000000000000355 ) ) ;
#2834 = CARTESIAN_POINT ( 'NONE',  ( 16.56230152254411081, -6.928203230275506996, -4.724999998771005849 ) ) ;
#2835 = CARTESIAN_POINT ( 'NONE',  ( -39.71205436395490551, 214.6737587650352168, 4.842901733360204908 ) ) ;
#2836 = CARTESIAN_POINT ( 'NONE',  ( 26.99999999999999645, 239.8937500012290229, 3.464101615137751278 ) ) ;
#2837 = CARTESIAN_POINT ( 'NONE',  ( 2.999999999999997335, 237.0000000000000000, -5.000000000000000000 ) ) ;
#2838 = CARTESIAN_POINT ( 'NONE',  ( -15.50000000000000533, 95.51018628210147199, -0.1745138560725808530 ) ) ;
#2839 = AXIS2_PLACEMENT_3D ( 'NONE', #27460, #15532, #7009 ) ;
#2840 = CARTESIAN_POINT ( 'NONE',  ( 2.311890736173175753, 10.12268628210144428, 12.53471296425194659 ) ) ;
#2841 = CARTESIAN_POINT ( 'NONE',  ( 24.00000000000000000, -5.196152422706629359, -0.2999999999999947153 ) ) ;
#2842 = CARTESIAN_POINT ( 'NONE',  ( 15.00000000000000000, 241.4687500012290684, -3.464101615137752610 ) ) ;
#2843 = CARTESIAN_POINT ( 'NONE',  ( 9.534712964251941258, 127.4226862821014521, -1.715153634034235708 ) ) ;
#2844 = EDGE_CURVE ( 'NONE', #14300, #3985, #33020, .T. ) ;
#2845 = ORIENTED_EDGE ( 'NONE', *, *, #16439, .F. ) ;
#2846 = CARTESIAN_POINT ( 'NONE',  ( 34.46482481169798717, 5.407089921784857367, 168.0851879843573897 ) ) ;
#2847 = CARTESIAN_POINT ( 'NONE',  ( -3.474262827703337830, 60.43518628210146204, -8.843639120294326972 ) ) ;
#2848 = CARTESIAN_POINT ( 'NONE',  ( 26.75643035624999655, 3.323476615752271712, -1.228124999385458160 ) ) ;
#2849 = DIRECTION ( 'NONE',  ( -0.000000000000000000, 1.000000000000000000, -0.000000000000000000 ) ) ;
#2850 = CARTESIAN_POINT ( 'NONE',  ( 20.99999999999999645, 0.000000000000000000, -8.000000000000000000 ) ) ;
#2851 = CARTESIAN_POINT ( 'NONE',  ( -27.24356964374999990, 195.3218750006145399, -15.72908226750537786 ) ) ;
#2852 = CARTESIAN_POINT ( 'NONE',  ( 15.00000000000039613, 3.464101615137982204, -3.131249998770963217 ) ) ;
#2853 = CARTESIAN_POINT ( 'NONE',  ( 25.28215217963232675, 3.464101615137679779, 167.7875028556106258 ) ) ;
#2854 = CARTESIAN_POINT ( 'NONE',  ( -2.064181346179062349, 36.10231371789854649, -9.465287035748106703 ) ) ;
#2855 = CARTESIAN_POINT ( 'NONE',  ( 25.16776026727616511, 0.000000000000000000, 166.4799973143651926 ) ) ;
#2856 = ORIENTED_EDGE ( 'NONE', *, *, #33700, .F. ) ;
#2857 = ORIENTED_EDGE ( 'NONE', *, *, #34192, .F. ) ;
#2858 = CARTESIAN_POINT ( 'NONE',  ( 18.12178482187499640, 248.3218750006145115, -4.985214923628404904 ) ) ;
#2859 = CARTESIAN_POINT ( 'NONE',  ( -4.622313124798826500, 41.56481371789855217, 11.61527771782809637 ) ) ;
#2860 = CARTESIAN_POINT ( 'NONE',  ( 19.68408634441911786, -5.407089921784861808, -9.496874999385534366 ) ) ;
#2861 = CARTESIAN_POINT ( 'NONE',  ( 26.75643035624999655, 7.049594010296217766E-16, -9.478124999385496352 ) ) ;
#2862 = CARTESIAN_POINT ( 'NONE',  ( -15.50000000000000533, 144.4898137178985280, 0.1745138560722471477 ) ) ;
#2863 = EDGE_CURVE ( 'NONE', #23355, #12420, #31331, .T. ) ;
#2864 = ORIENTED_EDGE ( 'NONE', *, *, #24228, .T. ) ;
#2865 = CARTESIAN_POINT ( 'NONE',  ( 22.80587116629411781, 3.604726614523243278, -3.084374999385516514 ) ) ;
#2866 = CARTESIAN_POINT ( 'NONE',  ( -27.24356964374999635, 198.4906250006145569, 15.72908226750539384 ) ) ;
#2867 = CARTESIAN_POINT ( 'NONE',  ( 31.19640481644053409, 7.209453229046482114, 166.5454403520519122 ) ) ;
#2868 = EDGE_CURVE ( 'NONE', #19993, #12997, #5359, .T. ) ;
#2869 = CARTESIAN_POINT ( 'NONE',  ( -42.47544563604516554, 214.8429017333602360, 4.673758765035156415 ) ) ;
#2870 = CARTESIAN_POINT ( 'NONE',  ( 15.24356964374999990, 249.7468750006145228, 0.000000000000000000 ) ) ;
#2871 = CARTESIAN_POINT ( 'NONE',  ( -27.03767660310608889, 194.9999999999999432, 1.836876173757454378 ) ) ;
#2872 = CARTESIAN_POINT ( 'NONE',  ( -58.70461230271184405, 208.6787018382582346, -4.469044688360757966 ) ) ;
#2873 = CARTESIAN_POINT ( 'NONE',  ( -38.92038769728823411, 208.1428034533959703, 6.469044688360770401 ) ) ;
#2874 = CARTESIAN_POINT ( 'NONE',  ( 31.43662783238875136, 7.209453229046475009, 169.2912019886672681 ) ) ;
#2875 = ORIENTED_EDGE ( 'NONE', *, *, #11274, .F. ) ;
#2876 = FACE_OUTER_BOUND ( 'NONE', #16775, .T. ) ;
#2877 = CARTESIAN_POINT ( 'NONE',  ( 15.00000000000000000, 0.000000000000000000, -0.3937499987709536242 ) ) ;
#2878 = CARTESIAN_POINT ( 'NONE',  ( -11.08355503943118592, 26.03981371789855714, -10.83675517735179383 ) ) ;
#2879 = CARTESIAN_POINT ( 'NONE',  ( -56.73288769728824832, 201.5309553116392181, -2.393094931466246855 ) ) ;
#2880 = PRODUCT ( 'rivet 1', 'rivet 1', '', ( #17586 ) ) ;
#2881 = CARTESIAN_POINT ( 'NONE',  ( -10.49813415415989581, 4.372686282101440725, -7.228626920339068285 ) ) ;
#2882 = CARTESIAN_POINT ( 'NONE',  ( 0.1745138560725515708, 51.81018628210144783, -12.50000000000000355 ) ) ;
#2883 = CARTESIAN_POINT ( 'NONE',  ( 22.56230152254412147, 3.464101615137759271, -5.137500000000033928 ) ) ;
#2884 = ORIENTED_EDGE ( 'NONE', *, *, #37146, .F. ) ;
#2885 = CARTESIAN_POINT ( 'NONE',  ( -47.82663769728823411, 204.3130714775002730, 3.149950860017883603 ) ) ;
#2886 = CARTESIAN_POINT ( 'NONE',  ( 13.50000000000001421, 195.2000000000000171, 23.38268590217984055 ) ) ;
#2887 = ADVANCED_FACE ( 'NONE', ( #13726 ), #36826, .T. ) ;
#2888 = CARTESIAN_POINT ( 'NONE',  ( 27.24356964375000700, 196.4468750006145115, 15.72908226750537075 ) ) ;
#2889 = DIRECTION ( 'NONE',  ( 1.000000000000000000, 0.000000000000000000, 0.000000000000000000 ) ) ;
#2890 = CARTESIAN_POINT ( 'NONE',  ( 7.234628195640363302, 196.3799038117967086, -26.99999999999996803 ) ) ;
#2891 = CARTESIAN_POINT ( 'NONE',  ( 20.99999999999999645, 185.0294372515228645, 0.000000000000000000 ) ) ;
#2892 = CARTESIAN_POINT ( 'NONE',  ( 16.56230152254410726, 0.000000000000000000, -10.00000000000000000 ) ) ;
#2893 = CARTESIAN_POINT ( 'NONE',  ( 15.24356964375000167, 246.2968750006145626, 3.323476615752272600 ) ) ;
#2894 = CARTESIAN_POINT ( 'NONE',  ( -8.843639120294245259, 89.86481371789855643, -3.474262827703533230 ) ) ;
#2895 = CARTESIAN_POINT ( 'NONE',  ( 26.75643035624999655, 240.5968750006145456, 3.323476615752267271 ) ) ;
#2896 = VECTOR ( 'NONE', #4173, 1000.000000000000000 ) ;
#2897 = ORIENTED_EDGE ( 'NONE', *, *, #6855, .F. ) ;
#2898 = CARTESIAN_POINT ( 'NONE',  ( -58.11830436395490551, 209.8844732041982581, 6.500000000000000888 ) ) ;
#2899 = CARTESIAN_POINT ( 'NONE',  ( 37.11555996377781952, 3.464101615137954671, 165.3594138002608531 ) ) ;
#2900 = CARTESIAN_POINT ( 'NONE',  ( 15.00000000000000178, 246.9437500012290343, 3.464101615137757051 ) ) ;
#2901 = EDGE_LOOP ( 'NONE', ( #23388, #29483, #13738, #17865, #4823, #28867 ) ) ;
#2902 = CARTESIAN_POINT ( 'NONE',  ( 4.944772684328420986, 95.61481371789857064, 11.48171059495408208 ) ) ;
#2903 = ADVANCED_FACE ( 'NONE', ( #26909 ), #32593, .F. ) ;
#2904 = CARTESIAN_POINT ( 'NONE',  ( 10.31873187879410914, 0.000000000000000000, -1.996874999385528371 ) ) ;
#2905 = CARTESIAN_POINT ( 'NONE',  ( 27.55866236128991176, -5.407089921784859143, 160.7843176865825967 ) ) ;
#2906 = CARTESIAN_POINT ( 'NONE',  ( 26.75643035624999655, -3.323476615752267715, -3.215624999385490401 ) ) ;
#2907 = CARTESIAN_POINT ( 'NONE',  ( -12.46528703574811558, 70.60231371789856780, 2.660918448318003726 ) ) ;
#2908 = CARTESIAN_POINT ( 'NONE',  ( -27.00000000000000355, 195.5000000000000000, 0.000000000000000000 ) ) ;
#2909 = VERTEX_POINT ( 'NONE', #15165 ) ;
#2910 = ORIENTED_EDGE ( 'NONE', *, *, #10356, .F. ) ;
#2911 = ORIENTED_EDGE ( 'NONE', *, *, #35826, .T. ) ;
#2912 = CARTESIAN_POINT ( 'NONE',  ( 26.99999999999999645, 3.464101615137755275, -7.331249998770939413 ) ) ;
#2913 = CARTESIAN_POINT ( 'NONE',  ( 23.87821517812499650, 4.985214923628404904, -3.440624999385466509 ) ) ;
#2914 = CARTESIAN_POINT ( 'NONE',  ( 27.00000000000015632, 3.464101615137663348, -6.487500000000022915 ) ) ;
#2915 = CARTESIAN_POINT ( 'NONE',  ( 26.75643035624999655, 247.7218750006145171, -7.049594010296217766E-16 ) ) ;
#2916 = EDGE_CURVE ( 'NONE', #24650, #4030, #22848, .T. ) ;
#2917 = CARTESIAN_POINT ( 'NONE',  ( 2.311890736173175753, 46.92268628210145209, 12.53471296425194836 ) ) ;
#2918 = CARTESIAN_POINT ( 'NONE',  ( -54.94419563604517265, 203.5000000000000000, 0.1155267958017914542 ) ) ;
#2919 = SURFACE_STYLE_FILL_AREA ( #20559 ) ;
#2920 = VECTOR ( 'NONE', #26806, 1000.000000000000000 ) ;
#2921 = CARTESIAN_POINT ( 'NONE',  ( -38.71502896937850124, 213.8393509191290889, -2.350049139982142155 ) ) ;
#2922 = CARTESIAN_POINT ( 'NONE',  ( 36.83775103377001869, 7.347880794884117764E-16, 162.1840432000934129 ) ) ;
#2923 = CARTESIAN_POINT ( 'NONE',  ( -12.50000000000000355, 98.48981371789855643, 0.1745138560722786503 ) ) ;
#2924 = CARTESIAN_POINT ( 'NONE',  ( -56.53497103062156270, 206.1606490808709111, -2.350049139982163027 ) ) ;
#2925 = CARTESIAN_POINT ( 'NONE',  ( -46.63913769728824121, 205.8500491399820760, -7.418979330068584233 ) ) ;
#2926 = EDGE_CURVE ( 'NONE', #4785, #26168, #26714, .T. ) ;
#2927 = CARTESIAN_POINT ( 'NONE',  ( 18.12178482187499640, 4.985214923628404904, -5.278124999385486404 ) ) ;
#2928 = CARTESIAN_POINT ( 'NONE',  ( 15.00000000000027711, 3.464101615137910706, -0.4874999999999961586 ) ) ;
#2929 = CARTESIAN_POINT ( 'NONE',  ( 13.23911966647199812, 85.55231371789855643, 8.632099005475788900 ) ) ;
#2930 = CARTESIAN_POINT ( 'NONE',  ( -54.74627896937850835, 201.4690446883607251, -2.162041339862721845 ) ) ;
#2931 = ORIENTED_EDGE ( 'NONE', *, *, #14124, .T. ) ;
#2932 = DIRECTION ( 'NONE',  ( -1.000000000000000000, 0.000000000000000000, 1.636531581110199847E-16 ) ) ;
#2933 = CARTESIAN_POINT ( 'NONE',  ( -4.622313124798576922, 106.4351862821014549, -11.61527771782819762 ) ) ;
#2934 = CARTESIAN_POINT ( 'NONE',  ( 14.25334919248782661, 54.68518628210145494, 6.092822981423971385 ) ) ;
#2935 = CARTESIAN_POINT ( 'NONE',  ( 15.00000000000000000, 243.2500000000000000, 0.000000000000000000 ) ) ;
#2936 = CARTESIAN_POINT ( 'NONE',  ( 27.61912665782109499, 5.407089921784862696, 161.4754277583837734 ) ) ;
#2937 = CARTESIAN_POINT ( 'NONE',  ( -14.25334919248782306, 68.48518628210145209, -6.092822981423979378 ) ) ;
#2938 = CARTESIAN_POINT ( 'NONE',  ( 26.99999999999999645, 247.1687500012290286, -3.464101615137755275 ) ) ;
#2939 = EDGE_CURVE ( 'NONE', #15590, #31540, #34457, .T. ) ;
#2940 = CARTESIAN_POINT ( 'NONE',  ( 16.56230152254410726, -7.209453229046475009, -8.578124999385506655 ) ) ;
#2941 = CARTESIAN_POINT ( 'NONE',  ( 26.99999999999999645, 7.347880794884117764E-16, -4.275000000000001243 ) ) ;
#2942 = CARTESIAN_POINT ( 'NONE',  ( -46.04538769728823411, 211.8571965466039444, -6.469044688360768625 ) ) ;
#2943 = CARTESIAN_POINT ( 'NONE',  ( 25.40308077269482112, 0.000000000000000000, 169.1697229992128939 ) ) ;
#2944 = CARTESIAN_POINT ( 'NONE',  ( 10.49813415415989581, 45.77268628210144641, 7.228626920339068285 ) ) ;
#2945 = CARTESIAN_POINT ( 'NONE',  ( 27.00000000000000355, 196.6250000000000284, -3.306546357697854128E-15 ) ) ;
#2946 = CARTESIAN_POINT ( 'NONE',  ( 20.99999999999998579, 247.9187500012290002, 5.999999999999998224 ) ) ;
#2947 = CARTESIAN_POINT ( 'NONE',  ( -1.715153634034442431, 142.4773137178985678, 9.534712964251900402 ) ) ;
#2948 = CARTESIAN_POINT ( 'NONE',  ( 18.12178482187499640, 247.9843750006145342, -4.985214923628404904 ) ) ;
#2949 = ORIENTED_EDGE ( 'NONE', *, *, #16877, .F. ) ;
#2950 = CARTESIAN_POINT ( 'NONE',  ( 15.00000000000000178, -3.464101615137757051, -4.462499999999992362 ) ) ;
#2951 = CARTESIAN_POINT ( 'NONE',  ( 22.60769515458672885, 243.5674038105676686, -5.999999999999998224 ) ) ;
#2952 = CARTESIAN_POINT ( 'NONE',  ( 33.89492370443730351, 5.196152422706631135, 162.9685126448345329 ) ) ;
#2953 = CARTESIAN_POINT ( 'NONE',  ( 19.68408634441910721, -5.407089921784855591, -4.940624999385550886 ) ) ;
#2954 = CARTESIAN_POINT ( 'NONE',  ( 34.53019161875872101, -5.407089921784855591, 168.8323340079261925 ) ) ;
#2955 =( BOUNDED_CURVE ( )  B_SPLINE_CURVE ( 2, ( #21166, #28596, #15279, #32514, #20981, #11545, #25761 ),
 .UNSPECIFIED., .F., .F. ) 
 B_SPLINE_CURVE_WITH_KNOTS ( ( 3, 2, 2, 3 ),
 ( 0.1521739130434802134, 0.1594202898550745040, 0.1666666666666688501, 0.1739130434782631685 ),
 .UNSPECIFIED. ) 
 CURVE ( )  GEOMETRIC_REPRESENTATION_ITEM ( )  RATIONAL_B_SPLINE_CURVE ( ( 0.9999999999999640288, 0.8660254037844746788, 1.000000000000000000, 0.8660254037844387076, 1.000000000000000000, 0.8660254037843960750, 1.000000000000042633 ) ) 
 REPRESENTATION_ITEM ( '' )  );
#2956 = CARTESIAN_POINT ( 'NONE',  ( 26.99999999999999645, 241.6750000000000114, -7.347880794884117764E-16 ) ) ;
#2957 = CARTESIAN_POINT ( 'NONE',  ( -13.50000000000000533, 196.4375000012290400, -23.38268590217984411 ) ) ;
#2958 = CARTESIAN_POINT ( 'NONE',  ( -12.53471296425194659, 76.82268628210145778, 2.311890736173176641 ) ) ;
#2959 = EDGE_LOOP ( 'NONE', ( #12802, #33780 ) ) ;
#2960 = ORIENTED_EDGE ( 'NONE', *, *, #36329, .F. ) ;
#2961 = CARTESIAN_POINT ( 'NONE',  ( 20.99999999999999289, 245.8374999999999773, -5.999999999999997335 ) ) ;
#2962 = EDGE_CURVE ( 'NONE', #18271, #22884, #7403, .T. ) ;
#2963 = CARTESIAN_POINT ( 'NONE',  ( 13.49999999999999645, 195.0125000012290570, -23.38268590217984766 ) ) ;
#2964 = CARTESIAN_POINT ( 'NONE',  ( 36.74950584413092258, 7.347880794884125653E-16, 161.1753960670511674 ) ) ;
#2965 = CARTESIAN_POINT ( 'NONE',  ( 15.24356964374999990, 0.000000000000000000, -6.440624999385469174 ) ) ;
#2966 = CARTESIAN_POINT ( 'NONE',  ( -15.53471296425188442, 34.37731371789854506, -2.908627838312459080 ) ) ;
#2967 = DIRECTION ( 'NONE',  ( -0.5887012860850802110, 0.8083506638593009885, 0.000000000000000000 ) ) ;
#2968 = CARTESIAN_POINT ( 'NONE',  ( 25.20698035151260896, 0.000000000000000000, 166.9282849285064856 ) ) ;
#2969 = CARTESIAN_POINT ( 'NONE',  ( -39.31622103062156981, 211.0902445701382533, 4.530955311639240257 ) ) ;
#2970 = LINE ( 'NONE', #28558, #1004 ) ;
#2971 = CARTESIAN_POINT ( 'NONE',  ( 30.64732363713033081, 7.209453229046482114, 160.2694137540738950 ) ) ;
#2972 = CARTESIAN_POINT ( 'NONE',  ( 8.710071997420211432, 28.91481371789854649, -3.796722387233181895 ) ) ;
#2973 = CARTESIAN_POINT ( 'NONE',  ( -62.67038769728823411, 208.1428034533959703, 6.469044688360770401 ) ) ;
#2974 =( BOUNDED_CURVE ( )  B_SPLINE_CURVE ( 2, ( #13003, #16223, #10152, #12806, #15662, #10338, #36478, #25112, #10519 ),
 .UNSPECIFIED., .F., .F. ) 
 B_SPLINE_CURVE_WITH_KNOTS ( ( 3, 2, 2, 2, 3 ),
 ( 0.06250000000000000000, 0.06944444444444444753, 0.08333333333333332871, 0.09722222222222222376, 0.1041666666666666713 ),
 .UNSPECIFIED. ) 
 CURVE ( )  GEOMETRIC_REPRESENTATION_ITEM ( )  RATIONAL_B_SPLINE_CURVE ( ( 0.9330127018922194093, 0.9330127018922194093, 1.000000000000000000, 0.8660254037844387076, 1.000000000000000000, 0.8660254037844387076, 1.000000000000000000, 0.9330127018922192983, 0.9330127018922194093 ) ) 
 REPRESENTATION_ITEM ( '' )  );
#2975 = CARTESIAN_POINT ( 'NONE',  ( 0.000000000000000000, 0.000000000000000000, 0.000000000000000000 ) ) ;
#2976 = CARTESIAN_POINT ( 'NONE',  ( 26.08383412631443932, 195.0000000000000284, 7.525172168543629247 ) ) ;
#2977 = CARTESIAN_POINT ( 'NONE',  ( 13.62178482187501416, 195.0593750006145513, 23.59362340125806767 ) ) ;
#2978 = CARTESIAN_POINT ( 'NONE',  ( 13.04141134922778988, 129.8273137178985905, -8.927990412390371944 ) ) ;
#2979 = EDGE_CURVE ( 'NONE', #31631, #35079, #36888, .T. ) ;
#2980 = VERTEX_POINT ( 'NONE', #6817 ) ;
#2981 = EDGE_CURVE ( 'NONE', #11333, #2407, #9779, .T. ) ;
#2982 = CARTESIAN_POINT ( 'NONE',  ( -10.69584247140444866, 39.44768628210145067, 6.932735513423972762 ) ) ;
#2983 = CARTESIAN_POINT ( 'NONE',  ( 20.99999999999999645, 210.0000000000000284, -8.000000000000000000 ) ) ;
#2984 = CARTESIAN_POINT ( 'NONE',  ( 26.60793733450167053, 1.299049382686714882, -8.000000000000000000 ) ) ;
#2985 = CARTESIAN_POINT ( 'NONE',  ( 27.51944227705346790, -5.407089921784859143, 160.3360300724413321 ) ) ;
#2986 = CARTESIAN_POINT ( 'NONE',  ( 26.99999999999999645, 7.347880794884117764E-16, -1.968749998770946696 ) ) ;
#2987 = CARTESIAN_POINT ( 'NONE',  ( 16.56230152254411436, -7.209453229046482114, -9.534374999385541116 ) ) ;
#2988 = DIRECTION ( 'NONE',  ( -0.5887012860850802110, 0.8083506638593008775, 2.465190328815661618E-32 ) ) ;
#2989 = CARTESIAN_POINT ( 'NONE',  ( -5.233372021372430183, 69.34768628210143504, -8.152565276336710909 ) ) ;
#2990 = CARTESIAN_POINT ( 'NONE',  ( 6.000000000000000000, -30.00000000000000000, 20.00000000000000000 ) ) ;
#2991 = DIRECTION ( 'NONE',  ( 1.000000000000000000, 0.000000000000000000, 0.000000000000000000 ) ) ;
#2992 = EDGE_CURVE ( 'NONE', #29774, #30702, #21427, .T. ) ;
#2993 = CARTESIAN_POINT ( 'NONE',  ( -12.46528703574805697, 86.59768628210144925, -2.660918448318280838 ) ) ;
#2994 = CARTESIAN_POINT ( 'NONE',  ( 30.66448242393021673, 6.928203230275514990, 160.4655395846485533 ) ) ;
#2995 = ORIENTED_EDGE ( 'NONE', *, *, #23969, .F. ) ;
#2996 = CARTESIAN_POINT ( 'NONE',  ( 30.73066631613276556, 7.209453229046475009, 161.2220249341241356 ) ) ;
#2997 = CARTESIAN_POINT ( 'NONE',  ( 15.24356964374999990, 0.000000000000000000, -7.790624999385459049 ) ) ;
#2998 = CARTESIAN_POINT ( 'NONE',  ( 13.62178482187499640, 196.1093750006145342, -23.59362340125807123 ) ) ;
#2999 = CARTESIAN_POINT ( 'NONE',  ( 34.42070221693199272, 5.407089921784862696, 167.5808644184484706 ) ) ;
#3000 = CARTESIAN_POINT ( 'NONE',  ( 31.25278368747686741, 6.928203230275514990, 167.1898537967678351 ) ) ;
#3001 = CARTESIAN_POINT ( 'NONE',  ( 26.97716818855048260, 0.000000000000000000, 49.47706554351410801 ) ) ;
#3002 = CARTESIAN_POINT ( 'NONE',  ( 23.99999999999999645, 248.5000000000000000, -5.196152422706631135 ) ) ;
#3003 = CARTESIAN_POINT ( 'NONE',  ( -27.24356964375000345, 197.9656250006145797, -15.72908226750537786 ) ) ;
#3004 = CARTESIAN_POINT ( 'NONE',  ( 8.962234695871567070, 113.4398137178985593, 8.715434833792127023 ) ) ;
#3005 = APPLICATION_CONTEXT ( 'automotive_design' ) ;
#3006 = CARTESIAN_POINT ( 'NONE',  ( 6.932735513423970097, 129.1476862821014890, 10.69584247140445044 ) ) ;
#3008 = VERTEX_POINT ( 'NONE', #7021 ) ;
#3007 = ORIENTED_EDGE ( 'NONE', *, *, #16185, .T. ) ;
#3009 = CARTESIAN_POINT ( 'NONE',  ( -13.62178482187500528, 198.8281250006145342, -23.59362340125807123 ) ) ;
#3010 = CARTESIAN_POINT ( 'NONE',  ( 18.12178482187499640, 242.4718750006145171, -4.985214923628404904 ) ) ;
#3011 = CARTESIAN_POINT ( 'NONE',  ( 3.257655550456945548, 95.90231371789855075, 15.46528703574811736 ) ) ;
#3012 = CARTESIAN_POINT ( 'NONE',  ( 15.24356964374999990, 0.000000000000000000, -4.303124999385482319 ) ) ;
#3013 = CARTESIAN_POINT ( 'NONE',  ( 18.12178482187500350, 248.1343750006145399, 4.985214923628407568 ) ) ;
#3014 = VECTOR ( 'NONE', #30318, 1000.000000000000000 ) ;
#3015 = CARTESIAN_POINT ( 'NONE',  ( 27.00000000000001066, 197.6000000012290627, 15.58845726811988897 ) ) ;
#3016 = CARTESIAN_POINT ( 'NONE',  ( 8.152565276336593669, 76.35231371789853938, 5.233372021372610483 ) ) ;
#3017 = CARTESIAN_POINT ( 'NONE',  ( 13.44051670066911441, -5.407089921784859143, -1.865624999385528948 ) ) ;
#3018 = CARTESIAN_POINT ( 'NONE',  ( 23.87821517812500005, 243.1468750006145285, 4.985214923628404016 ) ) ;
#3019 = CARTESIAN_POINT ( 'NONE',  ( -2.660918448318004614, 45.30231371789855643, -12.46528703574811558 ) ) ;
#3020 = CARTESIAN_POINT ( 'NONE',  ( 36.98482634954957859, 7.347880794884125653E-16, 163.8651217518988688 ) ) ;
#3021 = VECTOR ( 'NONE', #31303, 1000.000000000000000 ) ;
#3022 = CARTESIAN_POINT ( 'NONE',  ( -4.944772684328673229, 93.78518628210144925, 11.48171059495397728 ) ) ;
#3023 = CARTESIAN_POINT ( 'NONE',  ( 19.56230152254411436, -5.196152422706629359, -4.687499998771022192 ) ) ;
#3024 = CARTESIAN_POINT ( 'NONE',  ( -66.82663769728823411, 206.0451222850691408, 2.149950860017832532 ) ) ;
#3025 = FACE_OUTER_BOUND ( 'NONE', #7069, .T. ) ;
#3026 = PLANE ( 'NONE',  #24465 ) ;
#3027 = CARTESIAN_POINT ( 'NONE',  ( -0.1745138560725817967, 93.21018628210146062, 15.50000000000000533 ) ) ;
#3028 = CARTESIAN_POINT ( 'NONE',  ( 7.228626920339069173, 6.672686282101436106, -10.49813415415989404 ) ) ;
#3029 = DIRECTION ( 'NONE',  ( -0.000000000000000000, -1.000000000000000000, -0.000000000000000000 ) ) ;
#3030 = CARTESIAN_POINT ( 'NONE',  ( 24.00000000000000000, 244.3562500012290286, 5.196152422706629359 ) ) ;
#3031 = CARTESIAN_POINT ( 'NONE',  ( -5.529263428287477744, 130.8726862821014834, 7.954856959092191815 ) ) ;
#3032 = CARTESIAN_POINT ( 'NONE',  ( 36.84101937412247452, 3.464101615138092782, 162.2214005012719156 ) ) ;
#3033 = CARTESIAN_POINT ( 'NONE',  ( 23.87821517812500005, 242.6968750006145115, 4.985214923628404016 ) ) ;
#3035 = ORIENTED_EDGE ( 'NONE', *, *, #24256, .T. ) ;
#3034 = AXIS2_PLACEMENT_3D ( 'NONE', #30127, #4159, #1495 ) ;
#3036 = CARTESIAN_POINT ( 'NONE',  ( 22.56230152254278210, -3.464101615138517332, -4.649999998770996790 ) ) ;
#3037 = CARTESIAN_POINT ( 'NONE',  ( 3.474262827703335166, 55.83518628210145351, 8.843639120294326972 ) ) ;
#3038 = CARTESIAN_POINT ( 'NONE',  ( 18.12178482187499640, 4.985214923628404904, -1.115624999385472771 ) ) ;
#3039 = CARTESIAN_POINT ( 'NONE',  ( -27.24356964375000345, 194.8531250006145115, 0.000000000000000000 ) ) ;
#3040 = DIRECTION ( 'NONE',  ( 0.000000000000000000, -0.9932091452657081376, -0.1163425707149433747 ) ) ;
#3041 = CARTESIAN_POINT ( 'NONE',  ( 27.24356964375000700, 196.4468750006145115, 15.72908226750537075 ) ) ;
#3042 = CARTESIAN_POINT ( 'NONE',  ( 30.96843807686977001, -6.928203230275506996, 163.9397685954678536 ) ) ;
#3043 = LINE ( 'NONE', #5509, #7882 ) ;
#3044 = ADVANCED_FACE ( 'NONE', ( #18589 ), #33162, .F. ) ;
#3045 = CARTESIAN_POINT ( 'NONE',  ( 3.474262827703532341, 46.16481371789854649, -8.843639120294245259 ) ) ;
#3046 = ORIENTED_EDGE ( 'NONE', *, *, #24454, .T. ) ;
#3047 = ORIENTED_EDGE ( 'NONE', *, *, #8210, .T. ) ;
#3048 = CARTESIAN_POINT ( 'NONE',  ( 26.75643035624999655, 248.2093750006145285, -3.323476615752271712 ) ) ;
#3049 = VECTOR ( 'NONE', #10113, 1000.000000000000000 ) ;
#3050 = CARTESIAN_POINT ( 'NONE',  ( -2.660918448318005058, 36.10231371789854649, -12.46528703574811558 ) ) ;
#3051 = CARTESIAN_POINT ( 'NONE',  ( 22.80587116629411781, -3.604726614523238837, -8.559374999385489957 ) ) ;
#3052 = CARTESIAN_POINT ( 'NONE',  ( 21.00000000000000000, -6.646953231504538984, -10.04062499938548392 ) ) ;
#3053 = CARTESIAN_POINT ( 'NONE',  ( -0.1745138560722763466, 17.98981371789853867, -12.50000000000000355 ) ) ;
#3054 = ORIENTED_EDGE ( 'NONE', *, *, #7744, .T. ) ;
#3055 = CARTESIAN_POINT ( 'NONE',  ( 22.80587116629412492, -3.604726614523238837, -3.159374999385510474 ) ) ;
#3056 = CARTESIAN_POINT ( 'NONE',  ( 13.62178482187499640, 198.3031250006145285, -23.59362340125807123 ) ) ;
#3057 = CARTESIAN_POINT ( 'NONE',  ( 25.02888728581879718, -3.604726614523244610, 167.6873201206046815 ) ) ;
#3058 = VECTOR ( 'NONE', #11865, 1000.000000000000000 ) ;
#3059 = CARTESIAN_POINT ( 'NONE',  ( -33.76711230271183695, 216.4690446883607535, -1.857196546604089393 ) ) ;
#3060 = CARTESIAN_POINT ( 'NONE',  ( 23.87821517812500005, 249.4468750006145115, 4.985214923628404016 ) ) ;
#3061 = SHAPE_REPRESENTATION_RELATIONSHIP ( 'NONE' , 'NONE' ,  #6520, #19224 ) ;
#3062 = CARTESIAN_POINT ( 'NONE',  ( -27.10924108586912951, 194.9999999999999716, 0.1804593864224422750 ) ) ;
#3063 = CARTESIAN_POINT ( 'NONE',  ( -53.95461230271185116, 208.6787018382582346, -4.469044688360757966 ) ) ;
#3064 = CARTESIAN_POINT ( 'NONE',  ( -34.96205436395488420, 214.6737587650352168, 4.842901733360204908 ) ) ;
#3065 = CARTESIAN_POINT ( 'NONE',  ( 34.41253136604939300, -5.407089921784855591, 167.4874711655023418 ) ) ;
#3066 = ORIENTED_EDGE ( 'NONE', *, *, #18177, .T. ) ;
#3067 = CARTESIAN_POINT ( 'NONE',  ( -13.50000000000000533, 197.7875000012290627, -23.38268590217984411 ) ) ;
#3068 = CARTESIAN_POINT ( 'NONE',  ( 15.00000000000000000, 0.000000000000000000, -1.293749998770965526 ) ) ;
#3069 = CARTESIAN_POINT ( 'NONE',  ( -0.1745138560722442889, 17.98981371789853867, -15.50000000000000533 ) ) ;
#3070 = CARTESIAN_POINT ( 'NONE',  ( -65.04538769728823411, 212.3930949314662371, -8.469044688360781947 ) ) ;
#3071 = CARTESIAN_POINT ( 'NONE',  ( 0.1745138560725515708, 5.810186282101447830, -12.50000000000000355 ) ) ;
#3072 = CARTESIAN_POINT ( 'NONE',  ( 8.715434833791931624, 46.06018628210144072, 8.962234695871760692 ) ) ;
#3073 = CARTESIAN_POINT ( 'NONE',  ( 13.56230152254411969, -5.196152422706638241, -3.525000000000083844 ) ) ;
#3074 =( BOUNDED_CURVE ( )  B_SPLINE_CURVE ( 2, ( #2369, #22106, #7509, #33655, #37044, #16605, #13379, #13568, #11091 ),
 .UNSPECIFIED., .F., .F. ) 
 B_SPLINE_CURVE_WITH_KNOTS ( ( 3, 2, 2, 2, 3 ),
 ( 0.5208333333333333703, 0.5277777777777777901, 0.5416666666666666297, 0.5555555555555555802, 0.5625000000000000000 ),
 .UNSPECIFIED. ) 
 CURVE ( )  GEOMETRIC_REPRESENTATION_ITEM ( )  RATIONAL_B_SPLINE_CURVE ( ( 0.9330127018922192983, 0.9330127018922198534, 1.000000000000000000, 0.8660254037844387076, 1.000000000000000000, 0.8660254037844387076, 1.000000000000000000, 0.9330127018922194093, 0.9330127018922194093 ) ) 
 REPRESENTATION_ITEM ( '' )  );
#3075 = VERTEX_POINT ( 'NONE', #29563 ) ;
#3076 = CARTESIAN_POINT ( 'NONE',  ( -41.29538769728821990, 211.8571965466040012, -6.469044688360769513 ) ) ;
#3077 = CARTESIAN_POINT ( 'NONE',  ( 13.49999999999999645, 195.3500000000000227, -23.38268590217984766 ) ) ;
#3078 = CARTESIAN_POINT ( 'NONE',  ( -27.24356964375000345, 195.3593750006145342, 0.000000000000000000 ) ) ;
#3079 = DIRECTION ( 'NONE',  ( -1.000000000000000000, 2.775557561562892929E-15, 0.000000000000000000 ) ) ;
#3080 = CARTESIAN_POINT ( 'NONE',  ( 1.120210788295102201E-13, 196.4000000012290741, -27.00000000000000711 ) ) ;
#3081 = CYLINDRICAL_SURFACE ( 'NONE', #6138, 5.999999999999999112 ) ;
#3082 = PLANE ( 'NONE',  #1204 ) ;
#3083 = CARTESIAN_POINT ( 'NONE',  ( 15.24356964374999990, 245.8093750006145228, 0.000000000000000000 ) ) ;
#3084 = CARTESIAN_POINT ( 'NONE',  ( -8.152565276336593669, 90.15231371789855075, -5.233372021372610483 ) ) ;
#3085 = CARTESIAN_POINT ( 'NONE',  ( 36.78545758801501364, -3.464101615137356927, 161.5863263800139293 ) ) ;
#3086 = CIRCLE ( 'NONE', #4905, 4.000000000000003553 ) ;
#3087 = ORIENTED_EDGE ( 'NONE', *, *, #21957, .T. ) ;
#3088 = CARTESIAN_POINT ( 'NONE',  ( -53.76413769728823411, 213.1499508600178672, 5.686928522499718142 ) ) ;
#3089 = CARTESIAN_POINT ( 'NONE',  ( 13.50000000000001421, 197.1125000012290513, 23.38268590217984055 ) ) ;
#3090 = CARTESIAN_POINT ( 'NONE',  ( 24.00000000000000000, 245.7062500012290513, 5.196152422706629359 ) ) ;
#3091 = CARTESIAN_POINT ( 'NONE',  ( 12.53471296425189330, 103.3773137178985593, 2.311890736173451533 ) ) ;
#3092 = CARTESIAN_POINT ( 'NONE',  ( 19.68408634441911431, -5.407089921784861808, -0.9468749993855329894 ) ) ;
#3093 = CARTESIAN_POINT ( 'NONE',  ( 5.438367727407757144E-14, 198.2000000012290002, -27.00000000000000000 ) ) ;
#3094 = CARTESIAN_POINT ( 'NONE',  ( 23.87821517812500005, -4.985214923628404016, -1.903124999385497063 ) ) ;
#3095 = CARTESIAN_POINT ( 'NONE',  ( 8.715434833792128799, 74.33981371789855075, -8.962234695871567070 ) ) ;
#3096 = CARTESIAN_POINT ( 'NONE',  ( -13.62178482187498396, 198.1343750006145399, 23.59362340125808188 ) ) ;
#3097 = ORIENTED_EDGE ( 'NONE', *, *, #28113, .T. ) ;
#3098 = ORIENTED_EDGE ( 'NONE', *, *, #260, .T. ) ;
#3099 = ORIENTED_EDGE ( 'NONE', *, *, #7158, .T. ) ;
#3100 = CARTESIAN_POINT ( 'NONE',  ( 23.87821517812500005, -4.985214923628404016, -4.490624999385461891 ) ) ;
#3101 = DIRECTION ( 'NONE',  ( 1.000000000000000000, 6.123233995736766036E-17, -0.000000000000000000 ) ) ;
#3102 = CARTESIAN_POINT ( 'NONE',  ( 18.12178482187500350, 247.1218750006145228, 4.985214923628407568 ) ) ;
#3103 = CARTESIAN_POINT ( 'NONE',  ( 12.50000000000000355, 44.91018628210144215, 0.1745138560725507937 ) ) ;
#3104 = EDGE_CURVE ( 'NONE', #9049, #11398, #1499, .T. ) ;
#3105 = CARTESIAN_POINT ( 'NONE',  ( -48.01711230271182984, 216.4690446883607535, -1.857196546604089393 ) ) ;
#3106 = DIRECTION ( 'NONE',  ( 0.1219804832088915436, 0.9925324990730154395, 0.000000000000000000 ) ) ;
#3107 = CARTESIAN_POINT ( 'NONE',  ( -30.40252896937850124, 207.6499508600178387, -3.839350919129087547 ) ) ;
#3108 = PRESENTATION_STYLE_ASSIGNMENT (( #5764 ) ) ;
#3109 = CARTESIAN_POINT ( 'NONE',  ( 24.86053627419781265, 3.464101615137752166, 162.9684110048161187 ) ) ;
#3110 = VECTOR ( 'NONE', #6108, 1000.000000000000000 ) ;
#3111 = CARTESIAN_POINT ( 'NONE',  ( -8.715434833792127023, 106.5398137178985536, 8.962234695871568846 ) ) ;
#3112 = CARTESIAN_POINT ( 'NONE',  ( -64.45163769728823411, 213.9548777149308592, -2.149950860017830756 ) ) ;
#3113 = CARTESIAN_POINT ( 'NONE',  ( -38.92038769728823411, 207.6069050685337913, 8.469044688360781947 ) ) ;
#3114 = CARTESIAN_POINT ( 'NONE',  ( 20.99999999999999645, 6.646953231504538984, -4.415624999385457272 ) ) ;
#3115 = DIRECTION ( 'NONE',  ( -1.000000000000000000, 0.000000000000000000, 0.000000000000000000 ) ) ;
#3116 = CARTESIAN_POINT ( 'NONE',  ( 15.46528703574811736, 84.40231371789855075, -3.257655550456947768 ) ) ;
#3117 = CARTESIAN_POINT ( 'NONE',  ( -63.45461230271184405, 207.6069050685336492, -8.469044688360751749 ) ) ;
#3118 = ORIENTED_EDGE ( 'NONE', *, *, #23504, .F. ) ;
#3119 = PLANE ( 'NONE',  #34362 ) ;
#3120 = CARTESIAN_POINT ( 'NONE',  ( -8.962234695871760692, 103.5601862821014549, 8.715434833791933400 ) ) ;
#3121 = CARTESIAN_POINT ( 'NONE',  ( 10.83675517735155225, 55.26018628210144357, 11.08355503943142573 ) ) ;
#3122 = CYLINDRICAL_SURFACE ( 'NONE', #484, 5.999999999999994671 ) ;
#3123 = CARTESIAN_POINT ( 'NONE',  ( 24.63668644345436931, -3.604726614523244610, 163.2044439791918080 ) ) ;
#3124 = CARTESIAN_POINT ( 'NONE',  ( 6.092822981423978490, 70.78518628210143504, -14.25334919248782306 ) ) ;
#3125 = CARTESIAN_POINT ( 'NONE',  ( -27.24356964375000345, 198.8656250006145285, -15.72908226750537786 ) ) ;
#3126 = EDGE_CURVE ( 'NONE', #32537, #21538, #16483, .T. ) ;
#3127 = CARTESIAN_POINT ( 'NONE',  ( 16.56230152254411081, -7.209453229046475009, -8.128124999385510918 ) ) ;
#3128 = CARTESIAN_POINT ( 'NONE',  ( 13.56230152254410726, 5.196152422706636465, -8.625000000000021316 ) ) ;
#3129 = CARTESIAN_POINT ( 'NONE',  ( -49.21205436395490551, 214.6737587650352168, 4.842901733360204908 ) ) ;
#3130 = CARTESIAN_POINT ( 'NONE',  ( 1.120210788295102201E-13, 195.8375000000000057, -27.00000000000000711 ) ) ;
#3131 = CARTESIAN_POINT ( 'NONE',  ( 8.715434833791931624, 36.86018628210144499, 8.962234695871760692 ) ) ;
#3132 = CARTESIAN_POINT ( 'NONE',  ( 26.99999999999999645, 195.3125000000000284, -15.58845726811990495 ) ) ;
#3133 = CARTESIAN_POINT ( 'NONE',  ( 18.00000000000000355, 240.1750000000000114, 5.196152422706632912 ) ) ;
#3134 = CARTESIAN_POINT ( 'NONE',  ( 0.1745138560725194299, 15.01018628210143291, -9.500000000000005329 ) ) ;
#3135 = CARTESIAN_POINT ( 'NONE',  ( 23.87821517812500005, 246.4093750006145171, 4.985214923628404016 ) ) ;
#3136 = VERTEX_POINT ( 'NONE', #22541 ) ;
#3137 = CARTESIAN_POINT ( 'NONE',  ( 15.00000000000000178, -3.464101615137757051, -5.812500000000012434 ) ) ;
#3138 = AXIS2_PLACEMENT_3D ( 'NONE', #4717, #16110, #19522 ) ;
#3139 = DIRECTION ( 'NONE',  ( 0.08715574274765150453, 0.000000000000000000, 0.9961946980917461003 ) ) ;
#3140 = CARTESIAN_POINT ( 'NONE',  ( 5.649999999999991473, 244.5000000000000000, -5.000000000000001776 ) ) ;
#3141 = CARTESIAN_POINT ( 'NONE',  ( 19.68408634441910721, -5.407089921784855591, -4.490624999385572913 ) ) ;
#3142 = CARTESIAN_POINT ( 'NONE',  ( 37.49302179100721588, 3.604726614523238837, 166.8791739800475113 ) ) ;
#3143 = CARTESIAN_POINT ( 'NONE',  ( 18.00000000000000000, 241.8250000000000171, -5.196152422706630247 ) ) ;
#3144 = CARTESIAN_POINT ( 'NONE',  ( -7.234628195640263826, 196.4200961906613543, -27.00000000000003553 ) ) ;
#3145 = CARTESIAN_POINT ( 'NONE',  ( -8.962234695871760692, 75.96018628210144641, 8.715434833791933400 ) ) ;
#3146 = VERTEX_POINT ( 'NONE', #36552 ) ;
#3147 = VERTEX_POINT ( 'NONE', #13825 ) ;
#3148 = LINE ( 'NONE', #28737, #19432 ) ;
#3149 = CARTESIAN_POINT ( 'NONE',  ( -69.00000000000002842, 210.0000000000000000, 0.000000000000000000 ) ) ;
#3150 = CARTESIAN_POINT ( 'NONE',  ( 24.78536444607796341, 0.000000000000000000, 162.1091930777120069 ) ) ;
#3151 = CARTESIAN_POINT ( 'NONE',  ( 21.00000000000000000, -6.646953231504538984, -5.878124999385467397 ) ) ;
#3152 = PRODUCT_DEFINITION_CONTEXT ( 'detailed design', #6891, 'design' ) ;
#3153 = CARTESIAN_POINT ( 'NONE',  ( -15.50000000000000533, 34.08981371789853654, 0.1745138560722471477 ) ) ;
#3154 = CARTESIAN_POINT ( 'NONE',  ( 0.000000000000000000, 148.0000000000000000, -5.000000000000000888 ) ) ;
#3155 = CARTESIAN_POINT ( 'NONE',  ( 31.17434351900397971, 6.928203230275514990, 166.2932785684852490 ) ) ;
#3156 = CARTESIAN_POINT ( 'NONE',  ( -40.89955436395489841, 213.3788001182225003, -3.209657149897400252 ) ) ;
#3157 = DIRECTION ( 'NONE',  ( 0.000000000000000000, 0.000000000000000000, 1.000000000000000000 ) ) ;
#3158 = CARTESIAN_POINT ( 'NONE',  ( 31.38024896135242159, 6.928203230275506996, 168.6467885439513452 ) ) ;
#3159 = CARTESIAN_POINT ( 'NONE',  ( 6.840914352311949109, 21.43981371789854506, 6.594114490232462877 ) ) ;
#3160 = CARTESIAN_POINT ( 'NONE',  ( -60.88913769728823411, 206.8500491399821044, -5.686928522499717253 ) ) ;
#3161 = CARTESIAN_POINT ( 'NONE',  ( -36.34002896937849414, 202.6965474657332038, 4.350049139982197666 ) ) ;
#3162 = DIRECTION ( 'NONE',  ( 0.9873505073845697533, 0.1585527532634883052, 0.000000000000000000 ) ) ;
#3163 = CARTESIAN_POINT ( 'NONE',  ( 5.778771075727756162E-15, 195.4718750006145456, 31.45816453501075927 ) ) ;
#3164 = CARTESIAN_POINT ( 'NONE',  ( 3.257655550456945548, 132.7023137178985337, 15.46528703574811736 ) ) ;
#3165 = ORIENTED_EDGE ( 'NONE', *, *, #32431, .T. ) ;
#3166 = CARTESIAN_POINT ( 'NONE',  ( 4.944772684328679446, 52.38518628210145067, -11.48171059495397373 ) ) ;
#3167 = FACE_OUTER_BOUND ( 'NONE', #12620, .T. ) ;
#3168 = DIRECTION ( 'NONE',  ( 0.000000000000000000, 0.000000000000000000, 1.000000000000000000 ) ) ;
#3169 = CARTESIAN_POINT ( 'NONE',  ( 34.53836246964132073, 5.407089921784862696, 168.9257272608723213 ) ) ;
#3170 = CARTESIAN_POINT ( 'NONE',  ( 15.00000000000000000, 3.464101615137752166, -2.681249998770962151 ) ) ;
#3171 = CARTESIAN_POINT ( 'NONE',  ( 22.80587116629412847, 3.604726614523243278, -9.834374999385516958 ) ) ;
#3172 =( BOUNDED_CURVE ( )  B_SPLINE_CURVE ( 2, ( #15702, #26489, #1276, #3372, #29711, #20828, #17981, #12847, #521 ),
 .UNSPECIFIED., .F., .F. ) 
 B_SPLINE_CURVE_WITH_KNOTS ( ( 3, 2, 2, 2, 3 ),
 ( 0.7291666666666667407, 0.7361111111111111605, 0.7500000000000000000, 0.7638888888888888395, 0.7708333333333333703 ),
 .UNSPECIFIED. ) 
 CURVE ( )  GEOMETRIC_REPRESENTATION_ITEM ( )  RATIONAL_B_SPLINE_CURVE ( ( 0.9330127018922192983, 0.9330127018922198534, 1.000000000000000000, 0.8660254037844387076, 1.000000000000000000, 0.8660254037844387076, 1.000000000000000000, 0.9330127018922187432, 0.9330127018922192983 ) ) 
 REPRESENTATION_ITEM ( '' )  );
#3173 = CARTESIAN_POINT ( 'NONE',  ( 5.529263428287477744, 61.87268628210144783, -7.954856959092191815 ) ) ;
#3174 = LINE ( 'NONE', #11895, #3762 ) ;
#3175 = FACE_OUTER_BOUND ( 'NONE', #34338, .T. ) ;
#3176 = CARTESIAN_POINT ( 'NONE',  ( 12.53471296425194836, 90.62268628210146915, -2.311890736173178418 ) ) ;
#3177 = DIRECTION ( 'NONE',  ( 1.000000000000000000, 0.000000000000000000, 0.000000000000000000 ) ) ;
#3178 = CYLINDRICAL_SURFACE ( 'NONE', #35316, 5.999999999999994671 ) ;
#3179 = ORIENTED_EDGE ( 'NONE', *, *, #27550, .T. ) ;
#3180 = CARTESIAN_POINT ( 'NONE',  ( 24.59910052939444824, 0.000000000000000000, 162.7748350156397521 ) ) ;
#3181 = CARTESIAN_POINT ( 'NONE',  ( 26.75643035624999655, -3.323476615752267715, -8.503124999385478944 ) ) ;
#3182 = CARTESIAN_POINT ( 'NONE',  ( 7.234628195640309123, 196.2674038105676573, -27.00000000000000711 ) ) ;
#3183 = CARTESIAN_POINT ( 'NONE',  ( 31.00030439525832193, 7.209453229046482114, 164.3040022813454755 ) ) ;
#3184 = CARTESIAN_POINT ( 'NONE',  ( 37.02404643378602600, 7.347880794884125653E-16, 164.3134093660401618 ) ) ;
#3185 = CARTESIAN_POINT ( 'NONE',  ( -27.00000000000000355, 198.2000000000000171, 0.000000000000000000 ) ) ;
#3186 = CARTESIAN_POINT ( 'NONE',  ( 21.00000000000000000, 247.8625000000000114, 6.928203230275506996 ) ) ;
#3187 = CARTESIAN_POINT ( 'NONE',  ( -13.62178482187498396, 198.0781250006145342, 23.59362340125808188 ) ) ;
#3188 = CARTESIAN_POINT ( 'NONE',  ( 2.660918448318002838, 114.3023137178985564, 12.46528703574811558 ) ) ;
#3189 = CARTESIAN_POINT ( 'NONE',  ( 4.944772684328679446, 116.7851862821014635, -11.48171059495397373 ) ) ;
#3191 = ORIENTED_EDGE ( 'NONE', *, *, #13578, .T. ) ;
#3190 = EDGE_LOOP ( 'NONE', ( #2250, #8751, #30136, #10651 ) ) ;
#3192 = CARTESIAN_POINT ( 'NONE',  ( -27.24356964374999990, 198.8656250006145569, -15.72908226750537786 ) ) ;
#3193 = CARTESIAN_POINT ( 'NONE',  ( 21.00000000000000000, 241.9843750006145058, -6.646953231504538984 ) ) ;
#3194 = CARTESIAN_POINT ( 'NONE',  ( 0.1745138560722461762, 86.98981371789857064, 15.50000000000000533 ) ) ;
#3195 = CIRCLE ( 'NONE', #34074, 2.649999999999992806 ) ;
#3196 = CARTESIAN_POINT ( 'NONE',  ( 23.87821517812499650, 4.985214923628404904, -5.353124999385477700 ) ) ;
#3197 = CARTESIAN_POINT ( 'NONE',  ( 23.87821517812500005, 248.2093750006145285, 4.985214923628404016 ) ) ;
#3198 = PRODUCT ( 'MAS-158', 'MAS-158', '', ( #32475 ) ) ;
#3199 = CARTESIAN_POINT ( 'NONE',  ( -27.00000000000000355, 196.0625000012290400, 0.000000000000000000 ) ) ;
#3200 = EDGE_CURVE ( 'NONE', #9774, #8415, #9802, .T. ) ;
#3201 = CARTESIAN_POINT ( 'NONE',  ( -5.233372021372612259, 78.65231371789856496, 8.152565276336593669 ) ) ;
#3202 = CARTESIAN_POINT ( 'NONE',  ( 19.68408634441910365, -5.407089921784855591, -5.390624999385557281 ) ) ;
#3203 = EDGE_CURVE ( 'NONE', #9264, #35280, #34242, .T. ) ;
#3204 = CARTESIAN_POINT ( 'NONE',  ( 18.12178482187500350, 243.0718750006145399, 4.985214923628407568 ) ) ;
#3205 = CARTESIAN_POINT ( 'NONE',  ( -11.48171059495408208, 42.71481371789855075, 4.944772684328421875 ) ) ;
#3206 = MECHANICAL_DESIGN_GEOMETRIC_PRESENTATION_REPRESENTATION (  '', ( #5694 ), #13523 ) ;
#3207 = DIRECTION ( 'NONE',  ( 0.000000000000000000, 0.000000000000000000, 1.000000000000000000 ) ) ;
#3208 = CIRCLE ( 'NONE', #26199, 2.649999999999990585 ) ;
#3209 = CARTESIAN_POINT ( 'NONE',  ( 6.932735513423970097, 92.34768628210144925, 10.69584247140445044 ) ) ;
#3210 = CARTESIAN_POINT ( 'NONE',  ( 19.56230152254410370, 5.196152422706631135, -4.087499998771032317 ) ) ;
#3211 = EDGE_CURVE ( 'NONE', #24650, #1318, #22173, .T. ) ;
#3212 = CARTESIAN_POINT ( 'NONE',  ( -63.85788769728821990, 214.4690446883608104, 1.321298161741840893 ) ) ;
#3213 = DIRECTION ( 'NONE',  ( -0.000000000000000000, -1.000000000000000000, -0.000000000000000000 ) ) ;
#3214 = CARTESIAN_POINT ( 'NONE',  ( 25.41288579386105440, 0.000000000000000000, 169.2817949039725818 ) ) ;
#3215 = CARTESIAN_POINT ( 'NONE',  ( 8.632099005475504683, 92.34768628210142083, 13.23911966647218996 ) ) ;
#3216 = CARTESIAN_POINT ( 'NONE',  ( -74.35000000000002274, 210.0000000000000000, 5.000000000000000000 ) ) ;
#3217 = DIRECTION ( 'NONE',  ( 1.000000000000000000, 0.000000000000000000, 0.000000000000000000 ) ) ;
#3218 = CARTESIAN_POINT ( 'NONE',  ( -5.233372021372430183, 115.3476862821014493, -8.152565276336710909 ) ) ;
#3219 = DIRECTION ( 'NONE',  ( 1.000000000000000000, 0.000000000000000000, 0.000000000000000000 ) ) ;
#3220 = CARTESIAN_POINT ( 'NONE',  ( -0.1745138560725817967, 19.61018628210144144, 15.50000000000000533 ) ) ;
#3221 = CARTESIAN_POINT ( 'NONE',  ( 13.62178482187501416, 195.0593750006145513, 23.59362340125806767 ) ) ;
#3222 = CARTESIAN_POINT ( 'NONE',  ( 26.75643035624999655, 241.8343750006145001, 3.323476615752267715 ) ) ;
#3223 = ORIENTED_EDGE ( 'NONE', *, *, #14047, .F. ) ;
#3224 = CARTESIAN_POINT ( 'NONE',  ( 16.56230152254411081, -6.928203230275506996, -4.724999998771005849 ) ) ;
#3225 = CARTESIAN_POINT ( 'NONE',  ( -7.954856959092191815, 68.77268628210143220, -5.529263428287477744 ) ) ;
#3226 = CARTESIAN_POINT ( 'NONE',  ( 18.12178482187500350, -4.985214923628407568, -0.9656249993854615354 ) ) ;
#3227 = CARTESIAN_POINT ( 'NONE',  ( 22.60769515458672885, 241.7674038105676573, -5.999999999999998224 ) ) ;
#3228 = FACE_OUTER_BOUND ( 'NONE', #7592, .T. ) ;
#3229 = CARTESIAN_POINT ( 'NONE',  ( 20.99999999999999645, 202.0000000000000000, 5.999999999999999112 ) ) ;
#3230 = CARTESIAN_POINT ( 'NONE',  ( 24.98473320761364036, -3.464101615138001744, 164.3879884495968042 ) ) ;
#3231 = CARTESIAN_POINT ( 'NONE',  ( -13.50000000000000533, 196.8875000012290286, -23.38268590217984411 ) ) ;
#3232 = CARTESIAN_POINT ( 'NONE',  ( 6.840914352311949109, 39.83981371789855075, 6.594114490232462877 ) ) ;
#3233 = CARTESIAN_POINT ( 'NONE',  ( -1.926257025242585782E-15, 199.2968750006145342, -31.45816453501076637 ) ) ;
#3234 = ORIENTED_EDGE ( 'NONE', *, *, #32163, .F. ) ;
#3235 =( BOUNDED_CURVE ( )  B_SPLINE_CURVE ( 2, ( #35009, #3357, #21004, #24208, #27048, #9052, #24025 ),
 .UNSPECIFIED., .F., .F. ) 
 B_SPLINE_CURVE_WITH_KNOTS ( ( 3, 2, 2, 3 ),
 ( 0.5869565217391301548, 0.5942028985507243899, 0.6014492753623187360, 0.6086956521739130821 ),
 .UNSPECIFIED. ) 
 CURVE ( )  GEOMETRIC_REPRESENTATION_ITEM ( )  RATIONAL_B_SPLINE_CURVE ( ( 1.000000000000006217, 0.8660254037844326014, 1.000000000000000000, 0.8660254037844387076, 1.000000000000000000, 0.8660254037844387076, 1.000000000000000000 ) ) 
 REPRESENTATION_ITEM ( '' )  );
#3236 = CARTESIAN_POINT ( 'NONE',  ( 18.91622474583366653, 239.6197971919061160, -5.725135026351895640 ) ) ;
#3237 = CARTESIAN_POINT ( 'NONE',  ( 12.50000000000000355, 47.88981371789854791, -0.1745138560722771515 ) ) ;
#3238 = CARTESIAN_POINT ( 'NONE',  ( 10.31873187879410558, 0.000000000000000000, -9.196874999385512339 ) ) ;
#3239 = CARTESIAN_POINT ( 'NONE',  ( 15.24356964375000167, -3.323476615752272600, -8.315624999385494931 ) ) ;
#3240 = CARTESIAN_POINT ( 'NONE',  ( 11.48171059495408208, 19.71481371789854364, -4.944772684328420986 ) ) ;
#3241 = VECTOR ( 'NONE', #12985, 1000.000000000000000 ) ;
#3242 = FACE_OUTER_BOUND ( 'NONE', #33221, .T. ) ;
#3243 = ORIENTED_EDGE ( 'NONE', *, *, #2916, .F. ) ;
#3244 = CARTESIAN_POINT ( 'NONE',  ( 13.44051670066911086, 5.407089921784862696, -3.871874999385516158 ) ) ;
#3245 = CARTESIAN_POINT ( 'NONE',  ( -27.24356964374999990, 199.7656250006145342, -15.72908226750537786 ) ) ;
#3246 = CARTESIAN_POINT ( 'NONE',  ( 37.44236251553515871, -3.604726614523238837, 166.3001358117817006 ) ) ;
#3247 = CARTESIAN_POINT ( 'NONE',  ( -34.36086230271183695, 213.1499508600178387, -5.686928522499747451 ) ) ;
#3248 = CARTESIAN_POINT ( 'NONE',  ( 23.87821517812500005, 248.5468750006145058, 4.985214923628404016 ) ) ;
#3249 = SURFACE_STYLE_FILL_AREA ( #23539 ) ;
#3250 = CARTESIAN_POINT ( 'NONE',  ( -26.01826704599283246, 194.9999999999999716, -7.493920110828625525 ) ) ;
#3251 = CARTESIAN_POINT ( 'NONE',  ( -60.88169563604516554, 210.1155267958017703, 4.499999999999996447 ) ) ;
#3252 = CARTESIAN_POINT ( 'NONE',  ( 37.03385145495223441, 7.347880794884117764E-16, 164.4254812707998497 ) ) ;
#3253 = CARTESIAN_POINT ( 'NONE',  ( 34.53019161875872101, -5.407089921784855591, 168.8323340079261925 ) ) ;
#3254 = ORIENTED_EDGE ( 'NONE', *, *, #14770, .T. ) ;
#3255 = CARTESIAN_POINT ( 'NONE',  ( 22.60769515458673240, 247.9388461906613372, 6.000000000000000000 ) ) ;
#3256 = CARTESIAN_POINT ( 'NONE',  ( -15.50000000000000533, 15.68981371789854329, 0.1745138560722471477 ) ) ;
#3257 =( GEOMETRIC_REPRESENTATION_CONTEXT ( 3 ) GLOBAL_UNCERTAINTY_ASSIGNED_CONTEXT ( ( #1914 ) ) GLOBAL_UNIT_ASSIGNED_CONTEXT ( ( #7486, #36656, #30615 ) ) REPRESENTATION_CONTEXT ( 'NONE', 'WORKASPACE' ) );
#3258 = CARTESIAN_POINT ( 'NONE',  ( -59.30580436395490551, 218.5000000000000000, 0.1155267958017064944 ) ) ;
#3259 = CARTESIAN_POINT ( 'NONE',  ( -69.00000000000002842, 206.0000000000000000, 2.500000000000002220 ) ) ;
#3260 = CARTESIAN_POINT ( 'NONE',  ( -3.796722387233375073, 130.5851862821014606, 8.710071997420127943 ) ) ;
#3261 = CARTESIAN_POINT ( 'NONE',  ( -11.48171059495397373, 40.88518628210144357, -4.944772684328680334 ) ) ;
#3262 = PRESENTATION_LAYER_ASSIGNMENT (  '', '', ( #12361 ) ) ;
#3263 = CARTESIAN_POINT ( 'NONE',  ( 13.56230152254410548, 5.196152422706636465, -5.025000000000029665 ) ) ;
#3264 = ORIENTED_EDGE ( 'NONE', *, *, #2916, .T. ) ;
#3265 = CARTESIAN_POINT ( 'NONE',  ( -45.45163769728822700, 215.6869285224996986, -3.149950860017881382 ) ) ;
#3266 = CARTESIAN_POINT ( 'NONE',  ( -3.253724281355068545E-15, 195.9500000012290002, -27.00000000000000000 ) ) ;
#3267 = CARTESIAN_POINT ( 'NONE',  ( -8.152565276336710909, 30.24768628210144783, 5.233372021372435512 ) ) ;
#3268 = CARTESIAN_POINT ( 'NONE',  ( 27.24356964375000345, 195.5843750006145285, -3.336375036156643733E-15 ) ) ;
#3269 = CARTESIAN_POINT ( 'NONE',  ( 5.999999999999999112, -20.00000000000000000, -19.99999999999999289 ) ) ;
#3270 = CARTESIAN_POINT ( 'NONE',  ( 26.99999999999981171, 3.464101615137862300, -4.181249998770934617 ) ) ;
#3271 = DIRECTION ( 'NONE',  ( 0.000000000000000000, 0.000000000000000000, 1.000000000000000000 ) ) ;
#3272 = CARTESIAN_POINT ( 'NONE',  ( 18.12178482187500350, 245.4343750006145228, 4.985214923628407568 ) ) ;
#3273 = CARTESIAN_POINT ( 'NONE',  ( 6.594114490232462877, 92.73981371789854222, -6.840914352311949109 ) ) ;
#3274 = CARTESIAN_POINT ( 'NONE',  ( 15.02283181144952628, 7.347880794884122694E-16, 50.52293445648592751 ) ) ;
#3275 = ORIENTED_EDGE ( 'NONE', *, *, #16803, .F. ) ;
#3276 = CARTESIAN_POINT ( 'NONE',  ( -57.32663769728823411, 204.3130714775002730, 3.149950860017883603 ) ) ;
#3277 = CARTESIAN_POINT ( 'NONE',  ( 15.00000000000000000, 245.5187500012290513, -3.464101615137752166 ) ) ;
#3278 = CARTESIAN_POINT ( 'NONE',  ( 11.48171059495408208, 93.31481371789855928, -4.944772684328420986 ) ) ;
#3279 = CARTESIAN_POINT ( 'NONE',  ( 13.44051670066911086, -5.407089921784865361, -0.5718749993855187785 ) ) ;
#3280 = CARTESIAN_POINT ( 'NONE',  ( 26.99999999999999645, 198.1250000012290400, -15.58845726811990495 ) ) ;
#3281 =( BOUNDED_CURVE ( )  B_SPLINE_CURVE ( 2, ( #18782, #2434, #5458, #16859, #34091, #20072, #28396, #25559, #34281 ),
 .UNSPECIFIED., .F., .F. ) 
 B_SPLINE_CURVE_WITH_KNOTS ( ( 3, 2, 2, 2, 3 ),
 ( 0.09782608695652174335, 0.1014492753623188470, 0.1086956521739130405, 0.1159420289855072478, 0.1195652173913043653 ),
 .UNSPECIFIED. ) 
 CURVE ( )  GEOMETRIC_REPRESENTATION_ITEM ( )  RATIONAL_B_SPLINE_CURVE ( ( 0.9330127018922194093, 0.9330127018922194093, 1.000000000000000000, 0.8660254037844387076, 1.000000000000000000, 0.8660254037844387076, 1.000000000000000000, 0.9330127018922190762, 0.9330127018922194093 ) ) 
 REPRESENTATION_ITEM ( '' )  );
#3282 = CARTESIAN_POINT ( 'NONE',  ( 23.87821517812499650, 4.985214923628404904, -1.303124999385479876 ) ) ;
#3283 = CARTESIAN_POINT ( 'NONE',  ( 12.50000000000000355, 66.28981371789855359, -0.1745138560722771515 ) ) ;
#3284 = CARTESIAN_POINT ( 'NONE',  ( 5.778771075727756162E-15, 198.1718750006145342, 31.45816453501075927 ) ) ;
#3285 = ORIENTED_EDGE ( 'NONE', *, *, #31093, .F. ) ;
#3286 = ORIENTED_EDGE ( 'NONE', *, *, #8631, .F. ) ;
#3288 = MECHANICAL_DESIGN_GEOMETRIC_PRESENTATION_REPRESENTATION (  '', ( #23270 ), #32860 ) ;
#3287 = CARTESIAN_POINT ( 'NONE',  ( 23.87821517812500005, -4.985214923628404016, -4.040624999385455496 ) ) ;
#3289 = LINE ( 'NONE', #29442, #15484 ) ;
#3290 = CARTESIAN_POINT ( 'NONE',  ( 18.12178482187500350, 246.2218750006145171, 4.985214923628407568 ) ) ;
#3291 = CARTESIAN_POINT ( 'NONE',  ( -0.1745138560725500443, 47.21018628210143930, 12.50000000000000355 ) ) ;
#3292 = CARTESIAN_POINT ( 'NONE',  ( -46.43377896937850124, 208.3738570449995109, 6.530955311639247363 ) ) ;
#3293 = CARTESIAN_POINT ( 'NONE',  ( 17.52409618573022954, 213.4759038142404677, -5.188047882447234471 ) ) ;
#3294 = CARTESIAN_POINT ( 'NONE',  ( -65.43377896937850835, 208.3738570449995109, 6.530955311639247363 ) ) ;
#3295 = CARTESIAN_POINT ( 'NONE',  ( 27.88507211235645400, 5.196152422706630247, 163.1178740895360306 ) ) ;
#3296 = CARTESIAN_POINT ( 'NONE',  ( 8.715434833792128799, 101.9398137178985593, -8.962234695871567070 ) ) ;
#3297 = CARTESIAN_POINT ( 'NONE',  ( -65.63913769728821990, 207.8500491399821613, -3.954877714930864485 ) ) ;
#3298 = CARTESIAN_POINT ( 'NONE',  ( -37.93080436395490551, 201.5000000000000000, -0.1155267958017054536 ) ) ;
#3299 =( BOUNDED_CURVE ( )  B_SPLINE_CURVE ( 2, ( #8475, #19868, #31773, #37452, #17573, #8846, #31961, #22887, #5993 ),
 .UNSPECIFIED., .F., .T. ) 
 B_SPLINE_CURVE_WITH_KNOTS ( ( 3, 2, 2, 2, 3 ),
 ( 0.5625000000000000000, 0.5694444444444444198, 0.5833333333333333703, 0.5972222222222222099, 0.6041666666666667407 ),
 .UNSPECIFIED. ) 
 CURVE ( )  GEOMETRIC_REPRESENTATION_ITEM ( )  RATIONAL_B_SPLINE_CURVE ( ( 0.9330127018922194093, 0.9330127018922194093, 1.000000000000000000, 0.8660254037844387076, 1.000000000000000000, 0.8660254037844387076, 1.000000000000000000, 0.9330127018922187432, 0.9330127018922192983 ) ) 
 REPRESENTATION_ITEM ( '' )  );
#3300 = CARTESIAN_POINT ( 'NONE',  ( 18.12178482187499640, 4.985214923628404904, -3.478124999385490135 ) ) ;
#3301 = DIRECTION ( 'NONE',  ( 0.000000000000000000, 0.000000000000000000, -1.000000000000000000 ) ) ;
#3302 = CARTESIAN_POINT ( 'NONE',  ( -0.1745138560722442889, 73.18981371789854506, -15.50000000000000533 ) ) ;
#3303 = CARTESIAN_POINT ( 'NONE',  ( -56.13169563604517265, 210.1155267958018271, 8.500000000000003553 ) ) ;
#3304 = ORIENTED_EDGE ( 'NONE', *, *, #22225, .T. ) ;
#3305 = CARTESIAN_POINT ( 'NONE',  ( 21.00000000000000000, 240.6624999999999943, 5.999999999999998224 ) ) ;
#3306 = CARTESIAN_POINT ( 'NONE',  ( 2.660918448318279950, 98.09768628210146346, -12.46528703574805697 ) ) ;
#3307 = CARTESIAN_POINT ( 'NONE',  ( -5.770363421893818234, 42.03518628210144925, -14.38691631536207005 ) ) ;
#3308 = CARTESIAN_POINT ( 'NONE',  ( 14.99999999999946709, 3.464101615137446188, -5.831249998770957177 ) ) ;
#3309 = LINE ( 'NONE', #27184, #33714 ) ;
#3310 = CARTESIAN_POINT ( 'NONE',  ( 10.83675517735155225, 64.46018628210146062, 11.08355503943142573 ) ) ;
#3311 = CARTESIAN_POINT ( 'NONE',  ( -13.62178482187500528, 198.8281250006145342, -23.59362340125807123 ) ) ;
#3312 = CARTESIAN_POINT ( 'NONE',  ( 22.80587116629410360, 7.646167579472015790E-16, -8.015624999385517313 ) ) ;
#3313 = CARTESIAN_POINT ( 'NONE',  ( 15.00000000000000000, 0.000000000000000000, -1.293749998770965526 ) ) ;
#3314 = CARTESIAN_POINT ( 'NONE',  ( -49.40997103062156981, 215.5714017266979852, 3.350049139982118618 ) ) ;
#3315 = ADVANCED_FACE ( 'NONE', ( #19149 ), #27843, .T. ) ;
#3316 = DIRECTION ( 'NONE',  ( -0.000000000000000000, -1.000000000000000000, -0.000000000000000000 ) ) ;
#3317 = CARTESIAN_POINT ( 'NONE',  ( 11.61527771782819940, 35.13518628210143646, -4.622313124798573369 ) ) ;
#3318 = CARTESIAN_POINT ( 'NONE',  ( -27.24356964375000345, 199.8593750006145342, 0.000000000000000000 ) ) ;
#3319 = CARTESIAN_POINT ( 'NONE',  ( 16.56230152254410726, 0.000000000000000000, 2.535898384862258492 ) ) ;
#3320 = CARTESIAN_POINT ( 'NONE',  ( 1.715153634034233487, 10.12268628210144428, 9.534712964251941258 ) ) ;
#3321 = CARTESIAN_POINT ( 'NONE',  ( 18.12178482187500350, 247.6843750006145228, 4.985214923628407568 ) ) ;
#3322 = ORIENTED_EDGE ( 'NONE', *, *, #16398, .T. ) ;
#3323 = CARTESIAN_POINT ( 'NONE',  ( 18.00000000000000355, -5.196152422706632912, -6.674999999999986500 ) ) ;
#3324 = FACE_OUTER_BOUND ( 'NONE', #20908, .T. ) ;
#3325 = DIRECTION ( 'NONE',  ( 1.000000000000000000, 0.000000000000000000, 0.000000000000000000 ) ) ;
#3326 = CARTESIAN_POINT ( 'NONE',  ( 13.44051670066911619, -5.407089921784859143, -4.565624999385536675 ) ) ;
#3327 = CARTESIAN_POINT ( 'NONE',  ( 28.01623001071507701, 5.407089921784856479, 166.0143398515642730 ) ) ;
#3328 = CARTESIAN_POINT ( 'NONE',  ( 23.99999999999999645, 242.1999999999999886, -5.196152422706631135 ) ) ;
#3329 = CARTESIAN_POINT ( 'NONE',  ( 5.727106289114498080E-15, 199.6625000000000227, 31.17691453623979214 ) ) ;
#3330 = CARTESIAN_POINT ( 'NONE',  ( 6.932735513423970097, 46.34768628210144925, 10.69584247140445044 ) ) ;
#3331 = ORIENTED_EDGE ( 'NONE', *, *, #24454, .F. ) ;
#3332 = ORIENTED_EDGE ( 'NONE', *, *, #6641, .T. ) ;
#3333 = CARTESIAN_POINT ( 'NONE',  ( 29.54925929127992745, 5.908847637349538218, 159.6727443940304738 ) ) ;
#3334 = CARTESIAN_POINT ( 'NONE',  ( -27.00000000000000355, 194.6888594429640591, -9.827195528215911580 ) ) ;
#3335 = CARTESIAN_POINT ( 'NONE',  ( 1.069080835302379631E-14, 198.4250000012290229, 27.00000000000000000 ) ) ;
#3336 = CARTESIAN_POINT ( 'NONE',  ( 18.12178482187499640, 4.985214923628404904, -6.515624999385460470 ) ) ;
#3337 = CARTESIAN_POINT ( 'NONE',  ( -12.50000000000000355, 86.31018628210145494, -0.1745138560725492671 ) ) ;
#3338 = CARTESIAN_POINT ( 'NONE',  ( -11.08355503943118592, 26.03981371789855714, -10.83675517735179383 ) ) ;
#3339 = CARTESIAN_POINT ( 'NONE',  ( 16.56230152254410726, 0.000000000000000000, -10.00000000000000000 ) ) ;
#3340 = EDGE_CURVE ( 'NONE', #18271, #21289, #36364, .T. ) ;
#3341 = CARTESIAN_POINT ( 'NONE',  ( 22.56230152254411792, 7.347880794884125653E-16, -0.2250000000000584865 ) ) ;
#3342 = CARTESIAN_POINT ( 'NONE',  ( -32.38913769728823411, 207.8500491399821613, -3.954877714930864485 ) ) ;
#3343 = ADVANCED_FACE ( 'NONE', ( #2432 ), #22730, .T. ) ;
#3344 = DIRECTION ( 'NONE',  ( 1.000000000000000000, 0.000000000000000000, 0.000000000000000000 ) ) ;
#3345 = CARTESIAN_POINT ( 'NONE',  ( 27.47531968228746990, -5.407089921784865361, 159.8317065065323845 ) ) ;
#3346 = CARTESIAN_POINT ( 'NONE',  ( 5.233372021372610483, 18.85231371789855359, -8.152565276336593669 ) ) ;
#3347 = CARTESIAN_POINT ( 'NONE',  ( -60.69122103062155560, 208.3738570449993404, -6.530955311639226935 ) ) ;
#3348 = CARTESIAN_POINT ( 'NONE',  ( -30.60044563604516199, 203.6929966515019430, -6.137860380172892150 ) ) ;
#3349 = EDGE_CURVE ( 'NONE', #18726, #12557, #28030, .T. ) ;
#3350 = AXIS2_PLACEMENT_3D ( 'NONE', #33502, #24964, #10381 ) ;
#3351 = CARTESIAN_POINT ( 'NONE',  ( 20.71295208575482505, 194.9999999999999716, -17.38774714927576071 ) ) ;
#3352 = CARTESIAN_POINT ( 'NONE',  ( 27.24356964375000345, 195.1343750006145399, -3.336375036156643733E-15 ) ) ;
#3353 = CARTESIAN_POINT ( 'NONE',  ( 14.38691631536194393, 140.4648137178985507, 5.770363421894124656 ) ) ;
#3354 = CARTESIAN_POINT ( 'NONE',  ( -55.53794563604516554, 205.3262412349647832, 4.842901733360250205 ) ) ;
#3355 = ORIENTED_EDGE ( 'NONE', *, *, #23085, .F. ) ;
#3356 = CARTESIAN_POINT ( 'NONE',  ( -4.622313124798576922, 51.23518628210143788, -11.61527771782819762 ) ) ;
#3357 = CARTESIAN_POINT ( 'NONE',  ( 27.00000000000015632, -3.464101615137659351, -6.112499999999985612 ) ) ;
#3358 = CARTESIAN_POINT ( 'NONE',  ( 15.00000000000000000, 247.2999999999999829, 0.000000000000000000 ) ) ;
#3359 = CARTESIAN_POINT ( 'NONE',  ( 25.02561894546576582, 0.000000000000000000, 167.6499628194262357 ) ) ;
#3360 = CARTESIAN_POINT ( 'NONE',  ( 15.00000000000000000, 3.464101615137752166, -3.131249998770958332 ) ) ;
#3361 = ORIENTED_EDGE ( 'NONE', *, *, #26146, .F. ) ;
#3362 = CARTESIAN_POINT ( 'NONE',  ( 22.80587116629410716, 7.646167579472015790E-16, -1.265624999385539518 ) ) ;
#3363 = CARTESIAN_POINT ( 'NONE',  ( -6.594114490232312775, 50.66018628210144925, -6.840914352312096547 ) ) ;
#3364 = PLANE ( 'NONE',  #6170 ) ;
#3365 = CARTESIAN_POINT ( 'NONE',  ( 26.99999999999999645, 244.8249999999999886, -7.347880794884117764E-16 ) ) ;
#3366 = CARTESIAN_POINT ( 'NONE',  ( 11.61527771782819940, 90.33518628210144641, -4.622313124798573369 ) ) ;
#3367 = CARTESIAN_POINT ( 'NONE',  ( 26.97716818855048260, 0.000000000000000000, 49.47706554351410801 ) ) ;
#3368 = ORIENTED_EDGE ( 'NONE', *, *, #25804, .F. ) ;
#3369 = CARTESIAN_POINT ( 'NONE',  ( 26.99999999999999645, 244.8812500012290343, -7.347880794884117764E-16 ) ) ;
#3370 = AXIS2_PLACEMENT_3D ( 'NONE', #21253, #9114, #3040 ) ;
#3371 = CARTESIAN_POINT ( 'NONE',  ( 18.00000000000000355, -5.196152422706632912, -0.3749999999999864553 ) ) ;
#3373 = ADVANCED_FACE ( 'NONE', ( #22355 ), #1874, .F. ) ;
#3372 = CARTESIAN_POINT ( 'NONE',  ( -26.99999999999999645, 195.6500000012290457, 15.58845726811991561 ) ) ;
#3374 = CARTESIAN_POINT ( 'NONE',  ( 37.32797060317886917, 7.646167579472024665E-16, 164.9926302705362957 ) ) ;
#3375 = CARTESIAN_POINT ( 'NONE',  ( 25.05336835491987557, -3.464101615137761048, 165.1724917731197593 ) ) ;
#3376 = CARTESIAN_POINT ( 'NONE',  ( 13.50000000000001421, 196.5500000000000114, 23.38268590217984055 ) ) ;
#3377 = CARTESIAN_POINT ( 'NONE',  ( 23.99999999999999645, 247.5999999999999943, -5.196152422706631135 ) ) ;
#3378 = CARTESIAN_POINT ( 'NONE',  ( 13.62178482187501416, 195.0031250006145456, 23.59362340125806767 ) ) ;
#3379 = AXIS2_PLACEMENT_3D ( 'NONE', #7264, #18463, #30385 ) ;
#3380 = CARTESIAN_POINT ( 'NONE',  ( 0.1745138560722779009, 105.3898137178985621, 12.50000000000000355 ) ) ;
#3381 = CARTESIAN_POINT ( 'NONE',  ( -10.49813415415989404, 114.7726862821014606, -7.228626920339069173 ) ) ;
#3383 = VERTEX_POINT ( 'NONE', #33905 ) ;
#3382 = ORIENTED_EDGE ( 'NONE', *, *, #2381, .T. ) ;
#3384 = CARTESIAN_POINT ( 'NONE',  ( -27.24356964375001056, 194.8294844423495533, -9.915847621322177119 ) ) ;
#3385 = CARTESIAN_POINT ( 'NONE',  ( 30.94882803475154986, 6.928203230275506996, 163.7156247883972071 ) ) ;
#3386 = ADVANCED_FACE ( 'NONE', ( #28394 ), #5091, .T. ) ;
#3387 = CARTESIAN_POINT ( 'NONE',  ( 8.632099005475788900, 83.25231371789854506, -13.23911966647199812 ) ) ;
#3388 = CARTESIAN_POINT ( 'NONE',  ( 26.75643035624999655, -3.323476615752267715, -4.565624999385477167 ) ) ;
#3389 = CARTESIAN_POINT ( 'NONE',  ( 15.24356964375000167, 247.1968750006145115, 3.323476615752272600 ) ) ;
#3390 = CARTESIAN_POINT ( 'NONE',  ( -5.529263428287477744, 103.2726862821014322, 7.954856959092191815 ) ) ;
#3391 = EDGE_CURVE ( 'NONE', #15520, #17083, #7946, .T. ) ;
#3392 = CARTESIAN_POINT ( 'NONE',  ( 26.99999999999999645, 195.4250000012290229, -15.58845726811990495 ) ) ;
#3393 = CARTESIAN_POINT ( 'NONE',  ( 1.715153634034445762, 82.67731371789852801, -9.534712964251895073 ) ) ;
#3394 = CARTESIAN_POINT ( 'NONE',  ( 19.68408634441910721, 5.407089921784857367, -6.590624999385563676 ) ) ;
#3395 = CARTESIAN_POINT ( 'NONE',  ( 15.24356964374999990, 242.0593750006145228, -3.323476615752268604 ) ) ;
#3396 = CARTESIAN_POINT ( 'NONE',  ( -2.311890736173448424, 50.47731371789855359, 12.53471296425189330 ) ) ;
#3397 = DIRECTION ( 'NONE',  ( -0.000000000000000000, -0.000000000000000000, 1.000000000000000000 ) ) ;
#3398 = CARTESIAN_POINT ( 'NONE',  ( -0.1745138560725500443, 102.4101862821014493, 12.50000000000000355 ) ) ;
#3399 = CARTESIAN_POINT ( 'NONE',  ( 16.56230152254410726, 6.928203230275506996, -6.749999998770969789 ) ) ;
#3400 = AXIS2_PLACEMENT_3D ( 'NONE', #30928, #4582, #28263 ) ;
#3401 = CARTESIAN_POINT ( 'NONE',  ( -33.97247103062156270, 206.6499508600178672, 5.571401726697986057 ) ) ;
#3402 = FACE_OUTER_BOUND ( 'NONE', #33356, .T. ) ;
#3403 = CARTESIAN_POINT ( 'NONE',  ( 24.73633934067528983, 0.000000000000000000, 161.5488335588110544 ) ) ;
#3404 = CARTESIAN_POINT ( 'NONE',  ( 13.04141134922759804, 82.57268628210144357, 8.927990412390657937 ) ) ;
#3405 = CARTESIAN_POINT ( 'NONE',  ( 5.649999999999985256, 244.5000000000000000, 5.000000000000000888 ) ) ;
#3406 = CARTESIAN_POINT ( 'NONE',  ( 20.99999999999999289, 244.0374999999999943, -5.999999999999997335 ) ) ;
#3407 = CARTESIAN_POINT ( 'NONE',  ( 1.715153634034233487, 111.3226862821014578, 9.534712964251941258 ) ) ;
#3408 = CARTESIAN_POINT ( 'NONE',  ( 1.069080835302379631E-14, 198.8750000012290400, 27.00000000000000000 ) ) ;
#3409 = CARTESIAN_POINT ( 'NONE',  ( 8.927990412390657937, 15.87268628210144605, -13.04141134922759804 ) ) ;
#3410 = CARTESIAN_POINT ( 'NONE',  ( 27.24356964375000700, 196.4468750006145115, 15.72908226750537075 ) ) ;
#3411 = CARTESIAN_POINT ( 'NONE',  ( 21.00000000000000000, 241.3093750006145228, 6.646953231504538984 ) ) ;
#3412 = EDGE_LOOP ( 'NONE', ( #13119, #17010, #21267, #27489 ) ) ;
#3413 = CARTESIAN_POINT ( 'NONE',  ( 24.91612954363902688, -3.604726614523240613, 166.3984932299484569 ) ) ;
#3414 = CARTESIAN_POINT ( 'NONE',  ( 26.75643035624999655, 3.323476615752271712, -1.678124999385453897 ) ) ;
#3415 = ADVANCED_FACE ( 'NONE', ( #7387 ), #7759, .T. ) ;
#3416 = CARTESIAN_POINT ( 'NONE',  ( 20.99999999999999645, 0.000000000000000000, -8.000000000000000000 ) ) ;
#3417 = DIRECTION ( 'NONE',  ( 1.000000000000000000, 0.000000000000000000, 0.000000000000000000 ) ) ;
#3418 = DIRECTION ( 'NONE',  ( 0.08715574274765150453, 0.000000000000000000, 0.9961946980917461003 ) ) ;
#3419 = CARTESIAN_POINT ( 'NONE',  ( 20.99999999999997868, 210.0000000000000000, 5.999999999999999112 ) ) ;
#3420 = CARTESIAN_POINT ( 'NONE',  ( 19.68408634441910721, 5.407089921784857367, -0.2906249993855358760 ) ) ;
#3421 = CARTESIAN_POINT ( 'NONE',  ( -6.594114490232462877, 14.53981371789855892, 6.840914352311949109 ) ) ;
#3422 = CARTESIAN_POINT ( 'NONE',  ( -27.24356964374999279, 198.9968750006145513, 15.72908226750539384 ) ) ;
#3423 = ORIENTED_EDGE ( 'NONE', *, *, #25829, .F. ) ;
#3424 = CARTESIAN_POINT ( 'NONE',  ( 18.00000000000000355, 240.2312500012290570, 5.196152422706632912 ) ) ;
#3425 = CARTESIAN_POINT ( 'NONE',  ( -10.49813415416004858, 51.62731371789855217, 7.228626920338840023 ) ) ;
#3426 = CARTESIAN_POINT ( 'NONE',  ( 15.24356964374999990, 0.000000000000000000, -1.040624999385481031 ) ) ;
#3427 = CARTESIAN_POINT ( 'NONE',  ( -4.944772684328424539, 8.214813717898532985, -11.48171059495408031 ) ) ;
#3428 = CARTESIAN_POINT ( 'NONE',  ( 19.56230152254412502, -5.196152422706635576, -1.200000000000062128 ) ) ;
#3429 = VERTEX_POINT ( 'NONE', #25189 ) ;
#3430 = CARTESIAN_POINT ( 'NONE',  ( 16.56230152254411436, -7.209453229046482114, -4.134374999385496352 ) ) ;
#3431 = ORIENTED_EDGE ( 'NONE', *, *, #30942, .T. ) ;
#3432 = CARTESIAN_POINT ( 'NONE',  ( -27.24356964375000345, 198.0031250006145456, 0.000000000000000000 ) ) ;
#3433 = CARTESIAN_POINT ( 'NONE',  ( 24.78703009969406779, 3.604726614523240613, 164.9228798334000601 ) ) ;
#3434 = CARTESIAN_POINT ( 'NONE',  ( -30.40252896937849769, 206.6499508600178387, -5.571401726697954970 ) ) ;
#3435 = DIRECTION ( 'NONE',  ( -0.000000000000000000, -1.000000000000000000, -0.000000000000000000 ) ) ;
#3436 = AXIS2_PLACEMENT_3D ( 'NONE', #21969, #13622, #10578 ) ;
#3437 = CARTESIAN_POINT ( 'NONE',  ( -26.52865046747503186, 195.0000000000000568, 5.702742731586317504 ) ) ;
#3438 = CARTESIAN_POINT ( 'NONE',  ( -59.10044563604517265, 206.6211998817775566, -3.209657149897419348 ) ) ;
#3439 = CARTESIAN_POINT ( 'NONE',  ( -37.93080436395489841, 203.5000000000000000, -0.1155267958017335561 ) ) ;
#3440 = CARTESIAN_POINT ( 'NONE',  ( 34.21643094486717729, -5.407089921784855591, 165.2460330947959051 ) ) ;
#3441 = ORIENTED_EDGE ( 'NONE', *, *, #11948, .T. ) ;
#3442 = CARTESIAN_POINT ( 'NONE',  ( -27.89350125246770418, 208.9432337700812354, 7.934313662097031816 ) ) ;
#3443 = CARTESIAN_POINT ( 'NONE',  ( 15.46528703574804986, 137.1976862821014436, 3.257655550457285720 ) ) ;
#3444 = CARTESIAN_POINT ( 'NONE',  ( -65.63913769728821990, 205.8500491399820760, -7.418979330068584233 ) ) ;
#3445 = CARTESIAN_POINT ( 'NONE',  ( -6.840914352312096547, 121.9601862821014606, 6.594114490232313663 ) ) ;
#3446 = ADVANCED_FACE ( 'NONE', ( #16857 ), #11157, .F. ) ;
#3447 = CARTESIAN_POINT ( 'NONE',  ( 2.660918448318279950, 24.49768628210144783, -12.46528703574805697 ) ) ;
#3448 = CARTESIAN_POINT ( 'NONE',  ( 22.56230152254411436, 3.464101615137759271, -6.037500000000025402 ) ) ;
#3449 = ORIENTED_EDGE ( 'NONE', *, *, #26598, .T. ) ;
#3450 = CARTESIAN_POINT ( 'NONE',  ( -35.95163769728823411, 215.6869285224996986, -3.149950860017881382 ) ) ;
#3451 = EDGE_CURVE ( 'NONE', #34986, #25827, #27661, .T. ) ;
#3452 = CARTESIAN_POINT ( 'NONE',  ( 11.08355503943142750, 126.5601862821014834, -10.83675517735155225 ) ) ;
#3453 =( BOUNDED_CURVE ( )  B_SPLINE_CURVE ( 2, ( #12781, #30602, #22258, #36451, #21517, #36082, #10679, #7847, #4619 ),
 .UNSPECIFIED., .F., .F. ) 
 B_SPLINE_CURVE_WITH_KNOTS ( ( 3, 2, 2, 2, 3 ),
 ( 0.5108695652173913526, 0.5144927536231883591, 0.5217391304347825942, 0.5289855072463768293, 0.5326086956521739468 ),
 .UNSPECIFIED. ) 
 CURVE ( )  GEOMETRIC_REPRESENTATION_ITEM ( )  RATIONAL_B_SPLINE_CURVE ( ( 0.9330127018922192983, 0.9330127018922202975, 1.000000000000000000, 0.8660254037844387076, 1.000000000000000000, 0.8660254037844387076, 1.000000000000000000, 0.9330127018922194093, 0.9330127018922194093 ) ) 
 REPRESENTATION_ITEM ( '' )  );
#3454 = CARTESIAN_POINT ( 'NONE',  ( -7.234628195640316228, 198.6700961906613543, -27.00000000000000000 ) ) ;
#3455 = CARTESIAN_POINT ( 'NONE',  ( 0.1745138560725194299, 5.810186282101448718, -9.500000000000005329 ) ) ;
#3456 = CARTESIAN_POINT ( 'NONE',  ( 27.24356964375000700, 195.0968750006145456, 15.72908226750537075 ) ) ;
#3457 = CARTESIAN_POINT ( 'NONE',  ( -3.253724281355068545E-15, 195.9500000012290002, -27.00000000000000000 ) ) ;
#3458 = DIRECTION ( 'NONE',  ( -0.000000000000000000, -1.000000000000000000, -0.000000000000000000 ) ) ;
#3459 = EDGE_CURVE ( 'NONE', #4369, #32041, #34461, .T. ) ;
#3460 = CARTESIAN_POINT ( 'NONE',  ( -77.00000000000002842, 206.0000000000000000, 2.500000000000002220 ) ) ;
#3461 = CARTESIAN_POINT ( 'NONE',  ( 18.12178482187500350, 241.8343750006145285, 4.985214923628407568 ) ) ;
#3462 = CARTESIAN_POINT ( 'NONE',  ( -1.715153634034442431, 87.27731371789855075, 9.534712964251900402 ) ) ;
#3463 = DIRECTION ( 'NONE',  ( 0.08715574274765150453, 0.000000000000000000, 0.9961946980917461003 ) ) ;
#3464 = ORIENTED_EDGE ( 'NONE', *, *, #11515, .T. ) ;
#3465 = CARTESIAN_POINT ( 'NONE',  ( -55.34747103062156981, 213.3500491399821328, -5.571401726697985168 ) ) ;
#3466 = PRODUCT_RELATED_PRODUCT_CATEGORY ( 'part', '', ( #3512 ) ) ;
#3467 = VECTOR ( 'NONE', #11039, 1000.000000000000000 ) ;
#3468 = CARTESIAN_POINT ( 'NONE',  ( 26.99999999999999645, 246.6437500012290513, 3.464101615137751278 ) ) ;
#3469 = CARTESIAN_POINT ( 'NONE',  ( -4.944772684328424539, 100.2148137178985650, -11.48171059495408031 ) ) ;
#3470 = CARTESIAN_POINT ( 'NONE',  ( 19.68408634441912142, -5.407089921784861808, -1.396874999385538940 ) ) ;
#3471 = CARTESIAN_POINT ( 'NONE',  ( 24.40626844856526745, -3.604726614523240613, 160.5707542461117612 ) ) ;
#3472 = CARTESIAN_POINT ( 'NONE',  ( 21.00000000000000000, 6.646953231504538984, -1.265624999385487115 ) ) ;
#3473 = CARTESIAN_POINT ( 'NONE',  ( -2.311890736173448424, 59.67731371789855643, 12.53471296425189330 ) ) ;
#3474 = CARTESIAN_POINT ( 'NONE',  ( -27.24356964374999635, 197.6468750006145285, 15.72908226750539384 ) ) ;
#3475 = ORIENTED_EDGE ( 'NONE', *, *, #28590, .T. ) ;
#3476 = ORIENTED_EDGE ( 'NONE', *, *, #22471, .T. ) ;
#3477 = CARTESIAN_POINT ( 'NONE',  ( 23.87821517812499650, 4.985214923628404904, -4.340624999385478411 ) ) ;
#3478 = CARTESIAN_POINT ( 'NONE',  ( 27.63994658577156827, 5.196152422706636465, 160.3160764999286698 ) ) ;
#3479 = CARTESIAN_POINT ( 'NONE',  ( 18.12178482187500350, 245.7718750006145001, 4.985214923628407568 ) ) ;
#3480 = CARTESIAN_POINT ( 'NONE',  ( 10.69584247140445221, 34.84768628210143504, -6.932735513423970097 ) ) ;
#3481 = CARTESIAN_POINT ( 'NONE',  ( -56.72544563604516554, 214.8429017333602360, 4.673758765035156415 ) ) ;
#3482 = FACE_OUTER_BOUND ( 'NONE', #24373, .T. ) ;
#3483 = CARTESIAN_POINT ( 'NONE',  ( -30.00669563604516554, 209.8844732041982297, -4.499999999999996447 ) ) ;
#3484 = CARTESIAN_POINT ( 'NONE',  ( 24.86380461455084756, 0.000000000000000000, 163.0057683059945930 ) ) ;
#3485 = CARTESIAN_POINT ( 'NONE',  ( -11.61527771782809282, 89.86481371789855643, -4.622313124798832717 ) ) ;
#3486 = CARTESIAN_POINT ( 'NONE',  ( -61.87872103062156981, 205.4690446883607535, 1.090244570138264368 ) ) ;
#3487 = CARTESIAN_POINT ( 'NONE',  ( -64.05580436395490551, 216.5000000000000000, 0.1155267958017343610 ) ) ;
#3488 = CARTESIAN_POINT ( 'NONE',  ( 18.12178482187499640, 4.985214923628404904, -5.728124999385491911 ) ) ;
#3489 = FACE_OUTER_BOUND ( 'NONE', #993, .T. ) ;
#3490 = CARTESIAN_POINT ( 'NONE',  ( 10.83675517735179206, 74.33981371789855075, -11.08355503943118769 ) ) ;
#3491 = CARTESIAN_POINT ( 'NONE',  ( -63.25669563604515844, 209.8844732041981729, -8.500000000000003553 ) ) ;
#3492 = CARTESIAN_POINT ( 'NONE',  ( 18.00000000000000355, -5.196152422706632912, -0.7687499987709400795 ) ) ;
#3493 = CARTESIAN_POINT ( 'NONE',  ( 2.660918448318279950, 79.69768628210144357, -12.46528703574805697 ) ) ;
#3494 = CARTESIAN_POINT ( 'NONE',  ( 15.50000000000000533, 44.91018628210144215, 0.1745138560725827404 ) ) ;
#3495 = LINE ( 'NONE', #20761, #21688 ) ;
#3496 = APPLICATION_CONTEXT ( 'automotive_design' ) ;
#3497 = CARTESIAN_POINT ( 'NONE',  ( 33.75396078491245078, 5.407089921784862696, 159.9599749780466027 ) ) ;
#3498 = VECTOR ( 'NONE', #5141, 1000.000000000000000 ) ;
#3499 = CARTESIAN_POINT ( 'NONE',  ( 15.50000000000000533, 54.11018628210144499, 0.1745138560725827404 ) ) ;
#3500 = CARTESIAN_POINT ( 'NONE',  ( -27.24356964375000345, 199.3531250006145399, 0.000000000000000000 ) ) ;
#3501 = CARTESIAN_POINT ( 'NONE',  ( 22.80587116629411071, -3.604726614523235284, -9.403124999385536142 ) ) ;
#3502 =( BOUNDED_CURVE ( )  B_SPLINE_CURVE ( 2, ( #28574, #14557, #25554, #31432, #5640, #7943, #28762, #11523, #28951 ),
 .UNSPECIFIED., .F., .F. ) 
 B_SPLINE_CURVE_WITH_KNOTS ( ( 3, 2, 2, 2, 3 ),
 ( 0.4375000000000000000, 0.4444444444444444198, 0.4583333333333333148, 0.4722222222222222099, 0.4791666666666666852 ),
 .UNSPECIFIED. ) 
 CURVE ( )  GEOMETRIC_REPRESENTATION_ITEM ( )  RATIONAL_B_SPLINE_CURVE ( ( 0.9330127018922194093, 0.9330127018922194093, 1.000000000000000000, 0.8660254037844387076, 1.000000000000000000, 0.8660254037844387076, 1.000000000000000000, 0.9330127018922190762, 0.9330127018922194093 ) ) 
 REPRESENTATION_ITEM ( '' )  );
#3503 = CARTESIAN_POINT ( 'NONE',  ( 24.00000000000000000, -5.196152422706629359, -2.043749998770966414 ) ) ;
#3504 = CARTESIAN_POINT ( 'NONE',  ( -50.20163769728823411, 215.6869285224996986, -3.149950860017881382 ) ) ;
#3505 = CARTESIAN_POINT ( 'NONE',  ( 19.39230484541326049, 249.0075961894323484, -5.999999999999997335 ) ) ;
#3506 = CARTESIAN_POINT ( 'NONE',  ( -11.48171059495397373, 31.68518628210144428, -4.944772684328680334 ) ) ;
#3507 = CARTESIAN_POINT ( 'NONE',  ( 37.03385145495223441, 7.347880794884117764E-16, 164.4254812707998497 ) ) ;
#3508 = CARTESIAN_POINT ( 'NONE',  ( -9.465287035748106703, 144.2023137178985905, 2.064181346179061460 ) ) ;
#3509 = CARTESIAN_POINT ( 'NONE',  ( 15.24356964374999990, 246.2218750006145456, -3.323476615752268604 ) ) ;
#3510 = ORIENTED_EDGE ( 'NONE', *, *, #36113, .F. ) ;
#3511 = CARTESIAN_POINT ( 'NONE',  ( 15.00000000000000000, 3.464101615137752166, -7.687499999999988454 ) ) ;
#3513 = CARTESIAN_POINT ( 'NONE',  ( 26.99999999999999645, 7.347880794884117764E-16, -3.374999999999989342 ) ) ;
#3512 = PRODUCT ( 'follower plate', 'follower plate', '', ( #4473 ) ) ;
#3514 = CARTESIAN_POINT ( 'NONE',  ( 6.000769315822030740E-16, -20.00000000000000000, -4.899999999999999467 ) ) ;
#3515 = CARTESIAN_POINT ( 'NONE',  ( 22.80587116629411071, -3.604726614523235284, -5.353124999385542537 ) ) ;
#3516 = CARTESIAN_POINT ( 'NONE',  ( 25.06647319987872535, 3.604726614523236616, 168.1169290841567090 ) ) ;
#3517 = CARTESIAN_POINT ( 'NONE',  ( 21.00000000000000000, 242.0125000000000171, 6.928203230275506996 ) ) ;
#3518 = CARTESIAN_POINT ( 'NONE',  ( -5.732297079746171420, 222.9518338469886203, 2.500000000000000000 ) ) ;
#3519 = ADVANCED_FACE ( 'NONE', ( #8684 ), #14560, .T. ) ;
#3520 = CARTESIAN_POINT ( 'NONE',  ( -12.50000000000000355, 58.71018628210145351, -0.1745138560725492671 ) ) ;
#3521 = ORIENTED_EDGE ( 'NONE', *, *, #18712, .T. ) ;
#3522 = VECTOR ( 'NONE', #2849, 1000.000000000000000 ) ;
#3523 = EDGE_LOOP ( 'NONE', ( #30051, #36717 ) ) ;
#3524 = DIRECTION ( 'NONE',  ( 0.000000000000000000, 0.000000000000000000, 1.000000000000000000 ) ) ;
#3525 = CARTESIAN_POINT ( 'NONE',  ( 18.00000000000000355, 243.7750000000000057, 5.196152422706632912 ) ) ;
#3526 = CARTESIAN_POINT ( 'NONE',  ( 24.00000000000000000, -5.196152422706629359, -3.393749998770956289 ) ) ;
#3527 = DIRECTION ( 'NONE',  ( 0.08715574274765150453, 0.000000000000000000, 0.9961946980917461003 ) ) ;
#3528 = CARTESIAN_POINT ( 'NONE',  ( 26.75643035624999655, 7.049594010296217766E-16, -6.665624999385472371 ) ) ;
#3529 = CARTESIAN_POINT ( 'NONE',  ( 11.61527771782819940, 99.53518628210144925, -4.622313124798573369 ) ) ;
#3530 = CARTESIAN_POINT ( 'NONE',  ( 13.04141134922778988, 28.62731371789854506, -8.927990412390371944 ) ) ;
#3531 = CARTESIAN_POINT ( 'NONE',  ( 16.56230152254410726, 0.000000000000000000, -10.00000000000000000 ) ) ;
#3532 =( BOUNDED_CURVE ( )  B_SPLINE_CURVE ( 2, ( #34643, #20262, #20450, #31992, #17788, #6021, #334 ),
 .UNSPECIFIED., .F., .F. ) 
 B_SPLINE_CURVE_WITH_KNOTS ( ( 3, 2, 2, 3 ),
 ( 0.8958333333333333703, 0.9027777777777777901, 0.9166666666666666297, 0.9257860730087129619 ),
 .UNSPECIFIED. ) 
 CURVE ( )  GEOMETRIC_REPRESENTATION_ITEM ( )  RATIONAL_B_SPLINE_CURVE ( ( 0.9330127018922192983, 0.9330127018922198534, 1.000000000000000000, 0.8660254037844387076, 1.000000000000000000, 0.9120326476671077875, 0.9395835397633095498 ) ) 
 REPRESENTATION_ITEM ( '' )  );
#3533 = AXIS2_PLACEMENT_3D ( 'NONE', #32188, #12284, #905 ) ;
#3534 = CARTESIAN_POINT ( 'NONE',  ( -37.13913769728823411, 207.8500491399821613, -3.954877714930864485 ) ) ;
#3535 = CARTESIAN_POINT ( 'NONE',  ( 26.97716818855048260, 0.000000000000000000, 49.47706554351410801 ) ) ;
#3536 = CARTESIAN_POINT ( 'NONE',  ( 29.48996426250578295, 6.148716598298411107, 159.4803050314378368 ) ) ;
#3537 = CARTESIAN_POINT ( 'NONE',  ( -4.622313124798826500, 142.7648137178985621, 11.61527771782809637 ) ) ;
#3538 = CARTESIAN_POINT ( 'NONE',  ( -60.09747103062156981, 213.3500491399821328, -5.571401726697985168 ) ) ;
#3539 = ADVANCED_FACE ( 'NONE', ( #330 ), #8320, .T. ) ;
#3540 = CARTESIAN_POINT ( 'NONE',  ( -69.20163769728823411, 217.4189793300686233, -4.149950860017907139 ) ) ;
#3541 = DIRECTION ( 'NONE',  ( 0.000000000000000000, 1.000000000000000000, 0.000000000000000000 ) ) ;
#3542 = CARTESIAN_POINT ( 'NONE',  ( 24.81151116879471630, 3.464101615137512358, 162.4080514859152231 ) ) ;
#3543 = EDGE_CURVE ( 'NONE', #22652, #25991, #3174, .T. ) ;
#3544 = CARTESIAN_POINT ( 'NONE',  ( 27.24356964374999635, 199.1656250006145399, -15.72908226750539029 ) ) ;
#3545 = CARTESIAN_POINT ( 'NONE',  ( 15.46528703574811736, 139.6023137178985394, -3.257655550456947768 ) ) ;
#3546 = CARTESIAN_POINT ( 'NONE',  ( -59.49627896937850124, 203.4690446883607535, -1.626142955000504209 ) ) ;
#3547 = ORIENTED_EDGE ( 'NONE', *, *, #27779, .F. ) ;
#3548 = CARTESIAN_POINT ( 'NONE',  ( 12.46528703574805874, 54.39768628210146062, 2.660918448318279950 ) ) ;
#3549 = CARTESIAN_POINT ( 'NONE',  ( 26.99999999999999645, 245.2937500012290570, 3.464101615137751278 ) ) ;
#3550 = CARTESIAN_POINT ( 'NONE',  ( 26.09447537722126498, 2.706287405489508746, -7.999999999999998224 ) ) ;
#3551 = AXIS2_PLACEMENT_3D ( 'NONE', #7751, #19885, #2425 ) ;
#3552 = CARTESIAN_POINT ( 'NONE',  ( 25.06483902970220967, 0.000000000000000000, 168.0982504335675287 ) ) ;
#3553 = CARTESIAN_POINT ( 'NONE',  ( 15.53471296425195369, 109.0226862821014606, -2.908627838312120684 ) ) ;
#3554 = CARTESIAN_POINT ( 'NONE',  ( -67.02455436395489130, 205.1570982666397640, 4.673758765035199048 ) ) ;
#3555 = CARTESIAN_POINT ( 'NONE',  ( 10.31873187879411091, 3.604726614523236616, -0.6281249993855065883 ) ) ;
#3556 = CARTESIAN_POINT ( 'NONE',  ( -7.954856959092191815, 50.37268628210144783, -5.529263428287477744 ) ) ;
#3557 = DIRECTION ( 'NONE',  ( 0.000000000000000000, -0.000000000000000000, -1.000000000000000000 ) ) ;
#3558 = LINE ( 'NONE', #29135, #34671 ) ;
#3559 = EDGE_CURVE ( 'NONE', #17126, #2909, #8345, .T. ) ;
#3560 = CARTESIAN_POINT ( 'NONE',  ( 12.50000000000000355, 100.1101862821014521, 0.1745138560725507937 ) ) ;
#3561 = CARTESIAN_POINT ( 'NONE',  ( 33.97336387291019122, 5.196152422706631135, 163.8650878731170906 ) ) ;
#3562 = DIRECTION ( 'NONE',  ( -0.000000000000000000, 1.000000000000000000, -0.000000000000000000 ) ) ;
#3563 = ORIENTED_EDGE ( 'NONE', *, *, #11960, .T. ) ;
#3564 = CARTESIAN_POINT ( 'NONE',  ( 26.99999999999999645, 3.464101615137755275, -0.1875000000000169031 ) ) ;
#3565 = LINE ( 'NONE', #15128, #12722 ) ;
#3566 = CARTESIAN_POINT ( 'NONE',  ( 34.18538171151332961, 5.407089921784862696, 164.8911387336007408 ) ) ;
#3567 = UNCERTAINTY_MEASURE_WITH_UNIT (LENGTH_MEASURE( 1.000000000000000082E-05 ), #34263, 'distance_accuracy_value', 'NONE');
#3568 = CARTESIAN_POINT ( 'NONE',  ( 24.97492818644699142, -3.464101615137761048, 164.2759165448372016 ) ) ;
#3569 = CARTESIAN_POINT ( 'NONE',  ( -4.694659320240884604E-14, 197.0750000012290570, 27.00000000000000000 ) ) ;
#3570 = CARTESIAN_POINT ( 'NONE',  ( 18.00000000000000000, 249.0250000000000057, -5.196152422706630247 ) ) ;
#3571 = CARTESIAN_POINT ( 'NONE',  ( -27.24356964375000345, 196.1656250006145399, -15.72908226750537786 ) ) ;
#3572 = EDGE_CURVE ( 'NONE', #1351, #25827, #28567, .T. ) ;
#3573 = CARTESIAN_POINT ( 'NONE',  ( 2.660918448318002838, 95.90231371789856496, 12.46528703574811558 ) ) ;
#3574 = CARTESIAN_POINT ( 'NONE',  ( -11.61527771782819940, 113.3351862821014606, 4.622313124798574258 ) ) ;
#3575 = ORIENTED_EDGE ( 'NONE', *, *, #31144, .F. ) ;
#3576 = CARTESIAN_POINT ( 'NONE',  ( 27.24356964374999635, 195.5656250006145171, -15.72908226750539029 ) ) ;
#3577 = CARTESIAN_POINT ( 'NONE',  ( 23.87821517812499650, 240.5968750006145171, -4.985214923628404904 ) ) ;
#3578 = CARTESIAN_POINT ( 'NONE',  ( -14.38691631536193860, 80.66481371789856780, -5.770363421894132649 ) ) ;
#3579 = CARTESIAN_POINT ( 'NONE',  ( 15.24356964374999990, 0.000000000000000000, -4.753124999385488714 ) ) ;
#3580 = CARTESIAN_POINT ( 'NONE',  ( 18.12178482187499640, 247.9843750006145342, -4.985214923628404904 ) ) ;
#3581 = CARTESIAN_POINT ( 'NONE',  ( -6.594114490232312775, 105.8601862821014379, -6.840914352312096547 ) ) ;
#3582 = CARTESIAN_POINT ( 'NONE',  ( 0.000000000000000000, 210.0000000000000284, 0.000000000000000000 ) ) ;
#3583 = CARTESIAN_POINT ( 'NONE',  ( -3.796722387233185003, 72.61481371789855643, -8.710071997420207879 ) ) ;
#3584 = CARTESIAN_POINT ( 'NONE',  ( 16.56230152254411081, 7.209453229046475009, -6.103124999385545202 ) ) ;
#3585 = ADVANCED_FACE ( 'NONE', ( #34639 ), #144, .F. ) ;
#3586 = CARTESIAN_POINT ( 'NONE',  ( -9.534712964251895073, 107.9773137178985394, -1.715153634034446428 ) ) ;
#3587 = CARTESIAN_POINT ( 'NONE',  ( 15.24356964374999990, 242.0968750006145171, 0.000000000000000000 ) ) ;
#3588 = CARTESIAN_POINT ( 'NONE',  ( -11.61527771782809282, 53.06481371789854506, -4.622313124798832717 ) ) ;
#3589 = CARTESIAN_POINT ( 'NONE',  ( 26.99999999999999645, 7.347880794884117764E-16, -0.6187499987709565996 ) ) ;
#3590 = CARTESIAN_POINT ( 'NONE',  ( 12.46528703574805874, 100.3976862821014464, 2.660918448318279950 ) ) ;
#3591 = CARTESIAN_POINT ( 'NONE',  ( 16.56230152254411081, 6.928203230275506996, -5.849999998771011178 ) ) ;
#3592 = CARTESIAN_POINT ( 'NONE',  ( -64.84747103062156270, 212.3500491399821613, -3.839350919129076445 ) ) ;
#3593 = CARTESIAN_POINT ( 'NONE',  ( -11.61527771782819940, 140.9351862821014834, 4.622313124798574258 ) ) ;
#3594 = CARTESIAN_POINT ( 'NONE',  ( 27.82012958953286130, 5.407089921784856479, 163.7729017808578362 ) ) ;
#3595 = CARTESIAN_POINT ( 'NONE',  ( -10.83675517735155047, 87.46018628210146062, -11.08355503943142750 ) ) ;
#3596 = CARTESIAN_POINT ( 'NONE',  ( 22.80587116629412847, 3.604726614523243278, -4.884374999385531879 ) ) ;
#3597 = DIRECTION ( 'NONE',  ( 1.000000000000000000, 0.000000000000000000, 0.000000000000000000 ) ) ;
#3598 = CARTESIAN_POINT ( 'NONE',  ( -70.80918835584510873, 215.2843023367891249, 7.500000000000000000 ) ) ;
#3599 = CARTESIAN_POINT ( 'NONE',  ( 7.954856959092191815, 110.1726862821014663, 5.529263428287477744 ) ) ;
#3600 = CARTESIAN_POINT ( 'NONE',  ( 15.00000000000000000, 0.000000000000000000, -4.443749998770951670 ) ) ;
#3601 = CARTESIAN_POINT ( 'NONE',  ( -3.257655550457281723, 10.69768628210143646, 15.46528703574804986 ) ) ;
#3602 = CARTESIAN_POINT ( 'NONE',  ( 27.24356964375000345, 195.1343750006145399, -3.336375036156643733E-15 ) ) ;
#3603 = CARTESIAN_POINT ( 'NONE',  ( 18.12178482187499640, 241.1218750006145228, -4.985214923628404904 ) ) ;
#3604 = ORIENTED_EDGE ( 'NONE', *, *, #6147, .F. ) ;
#3605 = CARTESIAN_POINT ( 'NONE',  ( 34.30794447475221176, 5.407089921784857367, 166.2920375277922460 ) ) ;
#3606 = CARTESIAN_POINT ( 'NONE',  ( 15.24356964374999990, 3.323476615752268604, -3.328124999385480898 ) ) ;
#3607 = EDGE_CURVE ( 'NONE', #28581, #26637, #20070, .T. ) ;
#3608 = CARTESIAN_POINT ( 'NONE',  ( -13.62178482187498396, 199.4843750006145626, 23.59362340125808188 ) ) ;
#3609 = CARTESIAN_POINT ( 'NONE',  ( 20.99999999999999645, 6.928203230275506996, -3.712500000000020339 ) ) ;
#3610 = CARTESIAN_POINT ( 'NONE',  ( -30.00669563604516910, 209.8844732041982013, -6.500000000000000888 ) ) ;
#3611 = CARTESIAN_POINT ( 'NONE',  ( 24.00000000000000000, -5.196152422706629359, -7.443749998770954335 ) ) ;
#3612 = CYLINDRICAL_SURFACE ( 'NONE', #31490, 27.00000000000000355 ) ;
#3613 = CARTESIAN_POINT ( 'NONE',  ( 0.1745138560723095977, 22.58981371789854364, 9.500000000000005329 ) ) ;
#3614 = CARTESIAN_POINT ( 'NONE',  ( -27.24356964375000345, 197.5718750006145115, -15.72908226750537786 ) ) ;
#3616 = ORIENTED_EDGE ( 'NONE', *, *, #4742, .F. ) ;
#3615 = ORIENTED_EDGE ( 'NONE', *, *, #16784, .F. ) ;
#3617 = CARTESIAN_POINT ( 'NONE',  ( 23.87821517812500005, 248.0968750006144887, 4.985214923628404016 ) ) ;
#3618 = CARTESIAN_POINT ( 'NONE',  ( 0.1745138560722779009, 22.58981371789854720, 12.50000000000000355 ) ) ;
#3619 = CARTESIAN_POINT ( 'NONE',  ( 26.75643035624999655, -3.323476615752267715, -2.203124999385475569 ) ) ;
#3620 = CARTESIAN_POINT ( 'NONE',  ( 8.927990412390371944, 132.1273137178985735, 13.04141134922778811 ) ) ;
#3621 = CARTESIAN_POINT ( 'NONE',  ( 23.99999999999999645, 5.196152422706631135, -7.743749998770948828 ) ) ;
#3622 = VERTEX_POINT ( 'NONE', #2615 ) ;
#3623 = CARTESIAN_POINT ( 'NONE',  ( 13.44051670066910908, 5.407089921784862696, -4.321874999385522109 ) ) ;
#3624 = CARTESIAN_POINT ( 'NONE',  ( -13.62178482187500528, 197.9281250006145569, -23.59362340125807123 ) ) ;
#3625 = CARTESIAN_POINT ( 'NONE',  ( 30.90225418466721408, -7.209453229046482114, 163.1832832459922713 ) ) ;
#3626 = CARTESIAN_POINT ( 'NONE',  ( -63.65252896937850124, 205.6499508600178103, -7.303452534266820173 ) ) ;
#3627 = DIRECTION ( 'NONE',  ( 0.000000000000000000, -1.000000000000000000, 0.000000000000000000 ) ) ;
#3628 = SURFACE_STYLE_FILL_AREA ( #29208 ) ;
#3629 = DIRECTION ( 'NONE',  ( 0.000000000000000000, 0.000000000000000000, 1.000000000000000000 ) ) ;
#3630 = EDGE_CURVE ( 'NONE', #34798, #17216, #32174, .T. ) ;
#3631 = CARTESIAN_POINT ( 'NONE',  ( -43.06919563604516554, 214.5000000000000284, -0.1155267958017627827 ) ) ;
#3632 = CARTESIAN_POINT ( 'NONE',  ( 13.50000000000001421, 197.0000000000000000, 23.38268590217984055 ) ) ;
#3633 = CARTESIAN_POINT ( 'NONE',  ( 24.95208128752243226, 0.000000000000000000, 166.8094235429113041 ) ) ;
#3634 = ORIENTED_EDGE ( 'NONE', *, *, #27555, .T. ) ;
#3635 = AXIS2_PLACEMENT_3D ( 'NONE', #17497, #20911, #5918 ) ;
#3636 = CARTESIAN_POINT ( 'NONE',  ( 11.08355503943142750, 135.7601862821014720, -10.83675517735155225 ) ) ;
#3637 = CARTESIAN_POINT ( 'NONE',  ( -66.82663769728823411, 202.5810206699313767, 4.149950860017909804 ) ) ;
#3638 = CARTESIAN_POINT ( 'NONE',  ( 9.534712964251941258, 127.4226862821014521, -1.715153634034235708 ) ) ;
#3639 = CARTESIAN_POINT ( 'NONE',  ( 18.00000000000000000, 249.0812500012290513, -5.196152422706630247 ) ) ;
#3640 = CARTESIAN_POINT ( 'NONE',  ( -10.69584247140444866, 30.24768628210144783, 6.932735513423972762 ) ) ;
#3641 = CARTESIAN_POINT ( 'NONE',  ( 10.56230152254410726, 0.000000000000000000, -5.850000000000049383 ) ) ;
#3642 = ORIENTED_EDGE ( 'NONE', *, *, #9417, .T. ) ;
#3643 = CARTESIAN_POINT ( 'NONE',  ( -36.14955436395489841, 214.8429017333601792, -4.673758765035197271 ) ) ;
#3644 = CARTESIAN_POINT ( 'NONE',  ( 2.908627838312118019, 120.5226862821014322, 15.53471296425195369 ) ) ;
#3645 = LINE ( 'NONE', #6873, #19995 ) ;
#3646 = CARTESIAN_POINT ( 'NONE',  ( -8.843639120294326972, 12.13518628210144712, 3.474262827703335166 ) ) ;
#3647 = AXIS2_PLACEMENT_3D ( 'NONE', #15808, #1388, #36069 ) ;
#3648 = CARTESIAN_POINT ( 'NONE',  ( -27.24356964375000345, 198.0031250006145456, 0.000000000000000000 ) ) ;
#3649 = DIRECTION ( 'NONE',  ( 0.000000000000000000, 0.000000000000000000, 1.000000000000000000 ) ) ;
#3650 = CARTESIAN_POINT ( 'NONE',  ( 16.56230152254411436, 6.928203230275506996, -1.349999998771021614 ) ) ;
#3651 = CARTESIAN_POINT ( 'NONE',  ( 1.255007937094097924E-14, 199.1000000012290627, -27.00000000000000355 ) ) ;
#3652 = CARTESIAN_POINT ( 'NONE',  ( 5.233372021372610483, 83.25231371789854506, -8.152565276336593669 ) ) ;
#3653 = DIRECTION ( 'NONE',  ( -0.000000000000000000, -1.000000000000000000, -0.000000000000000000 ) ) ;
#3654 = ORIENTED_EDGE ( 'NONE', *, *, #12852, .T. ) ;
#3655 = CARTESIAN_POINT ( 'NONE',  ( 15.00000000000000178, 242.8937500012290513, 3.464101615137757051 ) ) ;
#3656 = CARTESIAN_POINT ( 'NONE',  ( 11.61527771782809637, 103.6648137178985678, 4.622313124798827388 ) ) ;
#3657 = CARTESIAN_POINT ( 'NONE',  ( 16.56230152254411436, -7.209453229046482114, -4.134374999385496352 ) ) ;
#3658 = CARTESIAN_POINT ( 'NONE',  ( 24.39973176785919406, 3.604726614523236616, 160.4960396437548411 ) ) ;
#3659 = CARTESIAN_POINT ( 'NONE',  ( 15.24356964374999990, 3.323476615752268604, -5.690624999385482496 ) ) ;
#3660 = CARTESIAN_POINT ( 'NONE',  ( 7.228626920338837358, 40.12731371789853796, 10.49813415416005036 ) ) ;
#3661 = CARTESIAN_POINT ( 'NONE',  ( -1.926257025242585782E-15, 197.0468750006145626, -31.45816453501075927 ) ) ;
#3662 = ORIENTED_EDGE ( 'NONE', *, *, #5683, .T. ) ;
#3663 = AXIS2_PLACEMENT_3D ( 'NONE', #29610, #21659, #33212 ) ;
#3664 = EDGE_LOOP ( 'NONE', ( #7038, #31958 ) ) ;
#3665 = CARTESIAN_POINT ( 'NONE',  ( 26.75643035624999655, -3.323476615752267271, -5.803124999385441463 ) ) ;
#3666 = CARTESIAN_POINT ( 'NONE',  ( 36.59589384753738273, 3.464101615138219348, 159.4196029116645548 ) ) ;
#3667 = CARTESIAN_POINT ( 'NONE',  ( 15.24356964374999990, 246.1093750006145342, -3.323476615752268604 ) ) ;
#3668 = CARTESIAN_POINT ( 'NONE',  ( -11.48171059495397373, 31.68518628210144428, -4.944772684328680334 ) ) ;
#3669 = EDGE_CURVE ( 'NONE', #3622, #7868, #13664, .T. ) ;
#3670 = CARTESIAN_POINT ( 'NONE',  ( -33.37127896937850124, 216.5309553116392181, 1.626142955000506429 ) ) ;
#3671 = CARTESIAN_POINT ( 'NONE',  ( 10.31873187879411091, 3.604726614523236616, -0.6281249993855065883 ) ) ;
#3672 = CARTESIAN_POINT ( 'NONE',  ( -31.59002896937850124, 206.1606490808709111, 2.350049139982143931 ) ) ;
#3673 = CARTESIAN_POINT ( 'NONE',  ( 24.58599568454271278, 3.464101615137752166, 159.8303977058271244 ) ) ;
#3674 = CARTESIAN_POINT ( 'NONE',  ( -12.50000000000000355, 80.08981371789855075, 0.1745138560722786503 ) ) ;
#3675 = ADVANCED_FACE ( 'NONE', ( #17226, #34277 ), #3364, .T. ) ;
#3676 = CARTESIAN_POINT ( 'NONE',  ( -61.48288769728824121, 205.5309553116392465, -1.321298161741839117 ) ) ;
#3678 = EDGE_CURVE ( 'NONE', #35499, #36556, #26294, .T. ) ;
#3677 = CARTESIAN_POINT ( 'NONE',  ( -33.18080436395489841, 201.5000000000000000, -0.1155267958017054536 ) ) ;
#3679 = CARTESIAN_POINT ( 'NONE',  ( 18.12178482187499640, 4.985214923628404904, -6.628124999385476279 ) ) ;
#3680 = CARTESIAN_POINT ( 'NONE',  ( 22.56230152254322263, 3.464101615138280632, -0.6375000000000334843 ) ) ;
#3681 = CARTESIAN_POINT ( 'NONE',  ( -2.908627838312453306, 59.67731371789855643, 15.53471296425188797 ) ) ;
#3682 = CARTESIAN_POINT ( 'NONE',  ( -61.27752896937849414, 214.3500491399821897, 7.303452534266821949 ) ) ;
#3683 = CARTESIAN_POINT ( 'NONE',  ( 20.99999999999999645, 185.0294372515228645, -5.999999999999999112 ) ) ;
#3684 = CARTESIAN_POINT ( 'NONE',  ( -0.1745138560725500443, 93.21018628210146062, 12.50000000000000355 ) ) ;
#3685 = CARTESIAN_POINT ( 'NONE',  ( 13.04141134922759804, 27.37268628210144428, 8.927990412390657937 ) ) ;
#3686 = CYLINDRICAL_SURFACE ( 'NONE', #28947, 5.999999999999998224 ) ;
#3687 = DIRECTION ( 'NONE',  ( -0.000000000000000000, 1.000000000000000000, -0.000000000000000000 ) ) ;
#3688 = CIRCLE ( 'NONE', #5491, 2.649999999999992806 ) ;
#3689 = CARTESIAN_POINT ( 'NONE',  ( -8.927990412390661490, 48.07268628210143646, 13.04141134922759804 ) ) ;
#3690 = CARTESIAN_POINT ( 'NONE',  ( 16.56230152254410726, 0.000000000000000000, -10.00000000000000000 ) ) ;
#3691 = LINE ( 'NONE', #12410, #22908 ) ;
#3692 = CARTESIAN_POINT ( 'NONE',  ( -36.54538769728823411, 211.8571965466039444, -6.469044688360768625 ) ) ;
#3693 = CARTESIAN_POINT ( 'NONE',  ( 27.00000000000001421, 195.6875000000000000, 15.58845726811988897 ) ) ;
#3694 = CARTESIAN_POINT ( 'NONE',  ( 0.1745138560725515708, 15.01018628210143468, -12.50000000000000355 ) ) ;
#3695 = CARTESIAN_POINT ( 'NONE',  ( 15.24356964374999990, 249.4093750006145171, 0.000000000000000000 ) ) ;
#3696 = CARTESIAN_POINT ( 'NONE',  ( 5.529263428287300108, 122.9273137178985422, 7.954856959092309943 ) ) ;
#3697 = CARTESIAN_POINT ( 'NONE',  ( 15.24356964375000167, 245.3968750006145285, 3.323476615752272600 ) ) ;
#3698 = VERTEX_POINT ( 'NONE', #29326 ) ;
#3699 = CARTESIAN_POINT ( 'NONE',  ( 23.99999999999999645, 5.196152422706631135, -6.899999999999989697 ) ) ;
#3700 = DIRECTION ( 'NONE',  ( -1.000000000000000000, -4.130293990420971855E-17, 0.000000000000000000 ) ) ;
#3701 = DIRECTION ( 'NONE',  ( -0.000000000000000000, 1.000000000000000000, -0.000000000000000000 ) ) ;
#3702 = CARTESIAN_POINT ( 'NONE',  ( 16.56230152254411081, 7.209453229046475009, -7.453124999385500438 ) ) ;
#3703 = CARTESIAN_POINT ( 'NONE',  ( 24.95208128752243226, 0.000000000000000000, 166.8094235429113041 ) ) ;
#3704 = PLANE ( 'NONE',  #32296 ) ;
#3705 = CARTESIAN_POINT ( 'NONE',  ( -12.53471296425194659, 49.22268628210144215, 2.311890736173176641 ) ) ;
#3706 = EDGE_LOOP ( 'NONE', ( #7520, #19620, #27501, #25106 ) ) ;
#3707 = ORIENTED_EDGE ( 'NONE', *, *, #21878, .T. ) ;
#3708 = DIRECTION ( 'NONE',  ( -1.000000000000000000, -6.123233995736766036E-17, -0.000000000000000000 ) ) ;
#3709 = CARTESIAN_POINT ( 'NONE',  ( 22.56230152254411792, 7.347880794884125653E-16, -2.025000000000027001 ) ) ;
#3710 = CARTESIAN_POINT ( 'NONE',  ( -47.00000000000000711, 237.0000000000000000, -5.000000000000000000 ) ) ;
#3711 = CARTESIAN_POINT ( 'NONE',  ( 20.99999999999995381, 242.9124999999999943, 5.999999999999998224 ) ) ;
#3712 = CARTESIAN_POINT ( 'NONE',  ( 18.12178482187499640, 4.985214923628404904, -7.415624999385473259 ) ) ;
#3713 = CARTESIAN_POINT ( 'NONE',  ( -6.932735513423968321, 87.74768628210145494, -10.69584247140445221 ) ) ;
#3714 = CARTESIAN_POINT ( 'NONE',  ( 15.46528703574811736, 20.00231371789855217, -3.257655550456947768 ) ) ;
#3715 = LINE ( 'NONE', #27030, #1238 ) ;
#3716 = DIRECTION ( 'NONE',  ( -1.000000000000000000, -0.000000000000000000, 5.782411586589356653E-16 ) ) ;
#3717 = CARTESIAN_POINT ( 'NONE',  ( -67.61086230271183695, 212.1499508600178387, -3.954877714930852495 ) ) ;
#3718 = CARTESIAN_POINT ( 'NONE',  ( -47.00000000000000711, 244.5000000000000000, 5.000000000000000000 ) ) ;
#3719 = CARTESIAN_POINT ( 'NONE',  ( 37.34761212884377812, 7.347880794884117764E-16, 168.0117821839301087 ) ) ;
#3720 = CARTESIAN_POINT ( 'NONE',  ( 7.228626920338837358, 132.1273137178986019, 10.49813415416005036 ) ) ;
#3721 = CARTESIAN_POINT ( 'NONE',  ( -54.95163769728823411, 215.6869285224996986, -3.149950860017881382 ) ) ;
#3722 = CARTESIAN_POINT ( 'NONE',  ( -34.16294563604517265, 216.1378603801729241, -6.307003348498026796 ) ) ;
#3723 = CARTESIAN_POINT ( 'NONE',  ( 23.87821517812499650, 4.985214923628404904, -0.4031249993854957303 ) ) ;
#3724 = CARTESIAN_POINT ( 'NONE',  ( -13.62178482187498396, 197.6281250006145171, 23.59362340125808188 ) ) ;
#3725 = CARTESIAN_POINT ( 'NONE',  ( 13.04141134922778988, 111.4273137178985422, -8.927990412390371944 ) ) ;
#3726 = CARTESIAN_POINT ( 'NONE',  ( -58.50669563604516554, 209.8844732041982013, -6.500000000000000888 ) ) ;
#3727 = ORIENTED_EDGE ( 'NONE', *, *, #35816, .T. ) ;
#3728 =( BOUNDED_CURVE ( )  B_SPLINE_CURVE ( 2, ( #23495, #35044, #6244, #25587, #34307, #8351, #5484 ),
 .UNSPECIFIED., .F., .F. ) 
 B_SPLINE_CURVE_WITH_KNOTS ( ( 3, 2, 2, 3 ),
 ( 0.1086956521739144144, 0.1159420289855087466, 0.1231884057971030788, 0.1304347826086973972 ),
 .UNSPECIFIED. ) 
 CURVE ( )  GEOMETRIC_REPRESENTATION_ITEM ( )  RATIONAL_B_SPLINE_CURVE ( ( 0.9999999999999745759, 0.8660254037844641317, 1.000000000000000000, 0.8660254037844387076, 1.000000000000000000, 0.8660254037844064001, 1.000000000000032419 ) ) 
 REPRESENTATION_ITEM ( '' )  );
#3729 = CARTESIAN_POINT ( 'NONE',  ( 2.311890736173175753, 28.52268628210144641, 12.53471296425194836 ) ) ;
#3730 = CARTESIAN_POINT ( 'NONE',  ( 15.00000000000000000, 0.000000000000000000, -7.649999999999989697 ) ) ;
#3731 = CARTESIAN_POINT ( 'NONE',  ( 31.42927406654086298, -6.928203230275514990, 169.2071480604035685 ) ) ;
#3732 = CARTESIAN_POINT ( 'NONE',  ( 25.02888728581879718, -3.604726614523244610, 167.6873201206046815 ) ) ;
#3733 = CARTESIAN_POINT ( 'NONE',  ( -3.257655550457281723, 102.6976862821014294, 15.46528703574804986 ) ) ;
#3734 = CARTESIAN_POINT ( 'NONE',  ( -69.59747103062156270, 213.3500491399821328, -5.571401726697985168 ) ) ;
#3735 = CARTESIAN_POINT ( 'NONE',  ( 19.68408634441910721, 5.407089921784857367, -2.090624999385559679 ) ) ;
#3736 = CARTESIAN_POINT ( 'NONE',  ( 9.465287035748067623, 54.39768628210144641, 2.064181346179272847 ) ) ;
#3737 = CARTESIAN_POINT ( 'NONE',  ( 2.999999999999997335, 244.5000000000000000, -2.499999999999999556 ) ) ;
#3738 = DIRECTION ( 'NONE',  ( 0.000000000000000000, 0.000000000000000000, 1.000000000000000000 ) ) ;
#3739 = CARTESIAN_POINT ( 'NONE',  ( -8.962234695871760692, 75.96018628210144641, 8.715434833791933400 ) ) ;
#3740 = CARTESIAN_POINT ( 'NONE',  ( 30.98804811898798661, 6.928203230275506996, 164.1639124025385001 ) ) ;
#3741 = CARTESIAN_POINT ( 'NONE',  ( 20.99999999999999645, 185.0294372515228645, 5.999999999999999112 ) ) ;
#3742 = EDGE_LOOP ( 'NONE', ( #1930, #7681, #28289, #18409 ) ) ;
#3743 = CARTESIAN_POINT ( 'NONE',  ( 20.99999999999997513, 244.9937500012290457, -5.999999999999999112 ) ) ;
#3744 = CARTESIAN_POINT ( 'NONE',  ( 15.24356964374999990, 3.323476615752268604, -9.628124999385486049 ) ) ;
#3745 = CARTESIAN_POINT ( 'NONE',  ( -7.234628195640302017, 198.4049038117967143, 27.00000000000000711 ) ) ;
#3746 = CARTESIAN_POINT ( 'NONE',  ( 37.28875051894242887, 7.646167579472024665E-16, 164.5443426563950027 ) ) ;
#3747 = CARTESIAN_POINT ( 'NONE',  ( 27.96678062107526941, -5.196152422706638241, 164.0518066177726553 ) ) ;
#3748 = CARTESIAN_POINT ( 'NONE',  ( 31.13512343476753585, 6.928203230275514990, 165.8449909543439560 ) ) ;
#3749 = CARTESIAN_POINT ( 'NONE',  ( 21.00000000000000000, 247.6374999999999886, -6.928203230275506996 ) ) ;
#3750 = CARTESIAN_POINT ( 'NONE',  ( -27.24356964375000345, 195.7531250006145456, 0.000000000000000000 ) ) ;
#3751 =( BOUNDED_CURVE ( )  B_SPLINE_CURVE ( 2, ( #28843, #8764, #5721, #34168, #14636, #17302, #19788 ),
 .UNSPECIFIED., .F., .F. ) 
 B_SPLINE_CURVE_WITH_KNOTS ( ( 3, 2, 2, 3 ),
 ( 0.1304347826086947326, 0.1376811594202889955, 0.1449275362318832860, 0.1521739130434775489 ),
 .UNSPECIFIED. ) 
 CURVE ( )  GEOMETRIC_REPRESENTATION_ITEM ( )  RATIONAL_B_SPLINE_CURVE ( ( 1.000000000000016875, 0.8660254037844218322, 1.000000000000000000, 0.8660254037844387076, 1.000000000000000000, 0.8660254037844520303, 0.9999999999999866773 ) ) 
 REPRESENTATION_ITEM ( '' )  );
#3752 = CARTESIAN_POINT ( 'NONE',  ( 4.622313124798831829, 101.3648137178985564, -11.61527771782809282 ) ) ;
#3753 = CARTESIAN_POINT ( 'NONE',  ( -4.622313124798576922, 106.4351862821014549, -11.61527771782819762 ) ) ;
#3754 = EDGE_LOOP ( 'NONE', ( #7663, #26831, #26253, #20177 ) ) ;
#3755 = ORIENTED_EDGE ( 'NONE', *, *, #23969, .T. ) ;
#3756 = CARTESIAN_POINT ( 'NONE',  ( -27.00000000000000355, 199.6250000012290684, -15.58845726811989429 ) ) ;
#3757 = CARTESIAN_POINT ( 'NONE',  ( 15.24356964375000167, 240.3343750006145001, 3.323476615752272600 ) ) ;
#3758 = CARTESIAN_POINT ( 'NONE',  ( 10.83675517735179206, 74.33981371789855075, -11.08355503943118769 ) ) ;
#3759 = CARTESIAN_POINT ( 'NONE',  ( 15.24356964374999990, 0.000000000000000000, -3.403124999385470417 ) ) ;
#3760 = CARTESIAN_POINT ( 'NONE',  ( 15.24356964374999990, 247.6093750006145342, 0.000000000000000000 ) ) ;
#3761 = CARTESIAN_POINT ( 'NONE',  ( 9.534712964251941258, 90.62268628210145494, -1.715153634034235708 ) ) ;
#3762 = VECTOR ( 'NONE', #35017, 1000.000000000000000 ) ;
#3763 = DIRECTION ( 'NONE',  ( 0.000000000000000000, 0.000000000000000000, -1.000000000000000000 ) ) ;
#3764 = CARTESIAN_POINT ( 'NONE',  ( -5.529263428287297444, 63.12731371789852375, -7.954856959092311719 ) ) ;
#3765 = CARTESIAN_POINT ( 'NONE',  ( 10.31873187879410736, 3.604726614523236616, -5.128124999385527794 ) ) ;
#3766 = CARTESIAN_POINT ( 'NONE',  ( 3.474262827703532341, 119.7648137178985905, -8.843639120294245259 ) ) ;
#3767 = CARTESIAN_POINT ( 'NONE',  ( 18.12178482187499640, 240.2218750006145171, -4.985214923628404904 ) ) ;
#3768 = CARTESIAN_POINT ( 'NONE',  ( -11.61527771782809282, 43.86481371789854933, -4.622313124798832717 ) ) ;
#3769 = CYLINDRICAL_SURFACE ( 'NONE', #32755, 5.999999999999998224 ) ;
#3770 = CARTESIAN_POINT ( 'NONE',  ( -6.932735513423968321, 96.94768628210145778, -10.69584247140445221 ) ) ;
#3771 = CARTESIAN_POINT ( 'NONE',  ( 22.56230152254411436, -3.464101615137751278, -5.099999998771006737 ) ) ;
#3772 = CARTESIAN_POINT ( 'NONE',  ( -68.40997103062156270, 213.8393509191290889, 2.350049139982164359 ) ) ;
#3773 = CYLINDRICAL_SURFACE ( 'NONE', #31872, 6.000000000000001776 ) ;
#3774 = CARTESIAN_POINT ( 'NONE',  ( 37.21848120135211957, 3.604726614523238837, 163.7411606810585170 ) ) ;
#3775 = CARTESIAN_POINT ( 'NONE',  ( 2.908627838312118019, 83.72268628210143504, 15.53471296425195369 ) ) ;
#3776 = CARTESIAN_POINT ( 'NONE',  ( 22.80587116629412847, 3.604726614523243278, -3.984374999385507987 ) ) ;
#3777 = DIRECTION ( 'NONE',  ( -0.000000000000000000, 1.000000000000000000, -0.000000000000000000 ) ) ;
#3778 = DIRECTION ( 'NONE',  ( -1.000000000000000000, 0.000000000000000000, -0.000000000000000000 ) ) ;
#3779 = CARTESIAN_POINT ( 'NONE',  ( -8.710071997420127943, 114.4851862821014663, -3.796722387233380402 ) ) ;
#3780 = CARTESIAN_POINT ( 'NONE',  ( 27.00000000000018474, -3.464101615137644696, -4.256249998770928578 ) ) ;
#3781 = CARTESIAN_POINT ( 'NONE',  ( -15.50000000000000533, 3.510186282101451560, -0.1745138560725808530 ) ) ;
#3782 = CARTESIAN_POINT ( 'NONE',  ( 27.24356964375000700, 196.8968750006145285, 15.72908226750537075 ) ) ;
#3783 = CARTESIAN_POINT ( 'NONE',  ( 26.75643035624999655, 242.2843750006145171, 3.323476615752267715 ) ) ;
#3784 = ORIENTED_EDGE ( 'NONE', *, *, #36113, .T. ) ;
#3785 = CARTESIAN_POINT ( 'NONE',  ( 25.06974154023176382, 0.000000000000000000, 168.1542863853351548 ) ) ;
#3786 = CARTESIAN_POINT ( 'NONE',  ( 15.24356964374999990, 0.000000000000000000, -1.940624999385465177 ) ) ;
#3787 = CARTESIAN_POINT ( 'NONE',  ( 19.96869161633227208, 239.9653672772770392, -5.848880403311082610 ) ) ;
#3788 = DIRECTION ( 'NONE',  ( -0.000000000000000000, 1.000000000000000000, -0.000000000000000000 ) ) ;
#3789 = CARTESIAN_POINT ( 'NONE',  ( 20.99999999999999645, 185.0294372515228645, 5.999999999999999112 ) ) ;
#3790 = ADVANCED_FACE ( 'NONE', ( #17412 ), #34826, .F. ) ;
#3791 = DIRECTION ( 'NONE',  ( 0.08715574274765150453, 0.000000000000000000, 0.9961946980917461003 ) ) ;
#3792 = CARTESIAN_POINT ( 'NONE',  ( 7.954856959092311719, 19.42731371789854933, -5.529263428287300108 ) ) ;
#3793 = CARTESIAN_POINT ( 'NONE',  ( -13.62178482187500528, 197.0843750006145285, -23.59362340125807123 ) ) ;
#3795 = ORIENTED_EDGE ( 'NONE', *, *, #10580, .F. ) ;
#3794 = ORIENTED_EDGE ( 'NONE', *, *, #27314, .F. ) ;
#3796 = CARTESIAN_POINT ( 'NONE',  ( 23.87821517812499650, 246.4468750006145115, -4.985214923628404904 ) ) ;
#3797 = CARTESIAN_POINT ( 'NONE',  ( 11.61527771782809637, 20.86481371789854222, 4.622313124798827388 ) ) ;
#3798 = CARTESIAN_POINT ( 'NONE',  ( 23.87821517812499650, 4.985214923628404904, -2.090624999385476634 ) ) ;
#3799 = CARTESIAN_POINT ( 'NONE',  ( 14.25334919248795451, 139.3148137178985451, -6.092822981423661410 ) ) ;
#3800 = CARTESIAN_POINT ( 'NONE',  ( 23.99999999999999645, 5.196152422706631135, -8.193749998770954335 ) ) ;
#3801 = EDGE_CURVE ( 'NONE', #23017, #36288, #12273, .T. ) ;
#3802 = CARTESIAN_POINT ( 'NONE',  ( 13.56230152254410370, 5.196152422706630247, -8.062499998771011533 ) ) ;
#3803 = ORIENTED_EDGE ( 'NONE', *, *, #2165, .T. ) ;
#3804 = CARTESIAN_POINT ( 'NONE',  ( 22.80587116629411426, -3.604726614523238837, -6.309374999385513050 ) ) ;
#3805 = AXIS2_PLACEMENT_3D ( 'NONE', #2409, #25905, #5616 ) ;
#3806 = CARTESIAN_POINT ( 'NONE',  ( -1.926257025242585782E-15, 196.9906250006145569, -31.45816453501075927 ) ) ;
#3807 = CARTESIAN_POINT ( 'NONE',  ( -12.46528703574805697, 132.5976862821014777, -2.660918448318280838 ) ) ;
#3808 = CARTESIAN_POINT ( 'NONE',  ( 37.24953043470598146, 7.646167579472024665E-16, 164.0960550422537096 ) ) ;
#3809 = CARTESIAN_POINT ( 'NONE',  ( -31.98586230271182984, 206.8500491399821328, 5.686928522499748340 ) ) ;
#3810 = CARTESIAN_POINT ( 'NONE',  ( 26.75643035624999655, 245.9593750006145285, -3.323476615752271268 ) ) ;
#3811 =( NAMED_UNIT ( * ) SI_UNIT ( $, .STERADIAN. ) SOLID_ANGLE_UNIT ( ) );
#3812 = EDGE_CURVE ( 'NONE', #27158, #34283, #15876, .T. ) ;
#3813 = DIRECTION ( 'NONE',  ( 0.08715574274765150453, 0.000000000000000000, 0.9961946980917461003 ) ) ;
#3814 = CARTESIAN_POINT ( 'NONE',  ( -45.64211230271183695, 205.5309553116392465, 1.321298161741817356 ) ) ;
#3815 = LINE ( 'NONE', #32062, #11502 ) ;
#3816 = CARTESIAN_POINT ( 'NONE',  ( 31.22091736908830839, -7.209453229046475009, 166.8256201108902133 ) ) ;
#3817 = VERTEX_POINT ( 'NONE', #32924 ) ;
#3818 = CARTESIAN_POINT ( 'NONE',  ( 26.99999999999999645, 241.7312500012290570, -7.347880794884117764E-16 ) ) ;
#3819 = CARTESIAN_POINT ( 'NONE',  ( -14.38691631536193860, 7.064813717898548617, -5.770363421894132649 ) ) ;
#3820 = CARTESIAN_POINT ( 'NONE',  ( -49.40997103062157692, 217.3034525342668815, 4.350049139982096413 ) ) ;
#3821 = ADVANCED_BREP_SHAPE_REPRESENTATION ( '', ( #33058, #17215 ), #19008 ) ;
#3822 = CIRCLE ( 'NONE', #29851, 2.649999999999999467 ) ;
#3823 = CARTESIAN_POINT ( 'NONE',  ( -0.1745138560725182642, 130.0101862821014436, 9.500000000000005329 ) ) ;
#3824 = CARTESIAN_POINT ( 'NONE',  ( 10.56230152254411081, 0.000000000000000000, -0.1687499993855146041 ) ) ;
#3825 = CARTESIAN_POINT ( 'NONE',  ( -0.1745138560725500443, 38.01018628210144357, 12.50000000000000355 ) ) ;
#3826 = CARTESIAN_POINT ( 'NONE',  ( 10.56230152254410726, 3.464101615137757051, -6.787500000000028955 ) ) ;
#3827 = VERTEX_POINT ( 'NONE', #6976 ) ;
#3828 = CARTESIAN_POINT ( 'NONE',  ( -31.99330436395490196, 210.1155267958017134, -6.500000000000000888 ) ) ;
#3829 = CARTESIAN_POINT ( 'NONE',  ( -13.23911966647218463, 122.2476862821014691, 8.632099005475506459 ) ) ;
#3830 =( GEOMETRIC_REPRESENTATION_CONTEXT ( 3 ) GLOBAL_UNCERTAINTY_ASSIGNED_CONTEXT ( ( #10847 ) ) GLOBAL_UNIT_ASSIGNED_CONTEXT ( ( #27171, #6708, #30204 ) ) REPRESENTATION_CONTEXT ( 'NONE', 'WORKASPACE' ) );
#3831 = LINE ( 'NONE', #18826, #25418 ) ;
#3832 = CARTESIAN_POINT ( 'NONE',  ( 0.1745138560723095977, 142.1898137178985451, 9.500000000000005329 ) ) ;
#3833 = CARTESIAN_POINT ( 'NONE',  ( -13.62178482187500528, 197.4781250006145399, -23.59362340125807123 ) ) ;
#3834 = CARTESIAN_POINT ( 'NONE',  ( 27.00000000000000355, 198.0875000012290457, -3.306546357697854128E-15 ) ) ;
#3835 = DIRECTION ( 'NONE',  ( 0.000000000000000000, 0.000000000000000000, 1.000000000000000000 ) ) ;
#3836 = CARTESIAN_POINT ( 'NONE',  ( 15.70715912503073142, 2.547338863122542651, -8.000000000000005329 ) ) ;
#3837 = LINE ( 'NONE', #27341, #5454 ) ;
#3838 = CARTESIAN_POINT ( 'NONE',  ( 6.840914352311949109, 67.43981371789855928, 6.594114490232462877 ) ) ;
#3839 = CARTESIAN_POINT ( 'NONE',  ( 23.87821517812499650, 240.2593750006145399, -4.985214923628404904 ) ) ;
#3840 = ORIENTED_EDGE ( 'NONE', *, *, #24664, .F. ) ;
#3841 = CARTESIAN_POINT ( 'NONE',  ( 18.00000000000000000, 244.1312500012290343, -5.196152422706630247 ) ) ;
#3842 = CARTESIAN_POINT ( 'NONE',  ( 10.49813415416005213, 74.62731371789855928, -7.228626920338837358 ) ) ;
#3843 = EDGE_CURVE ( 'NONE', #34832, #29417, #1457, .T. ) ;
#3844 = CARTESIAN_POINT ( 'NONE',  ( 13.44051670066911619, -5.407089921784865361, -3.721874999385532679 ) ) ;
#3845 = CARTESIAN_POINT ( 'NONE',  ( -29.00000000000002487, 210.0000000000000000, 0.000000000000000000 ) ) ;
#3846 = CARTESIAN_POINT ( 'NONE',  ( 23.87821517812499650, 4.985214923628404904, -4.003124999385487826 ) ) ;
#3847 = CARTESIAN_POINT ( 'NONE',  ( 12.50000000000000355, 57.08981371789855075, -0.1745138560722771515 ) ) ;
#3848 = ORIENTED_EDGE ( 'NONE', *, *, #5518, .T. ) ;
#3849 = AXIS2_PLACEMENT_3D ( 'NONE', #13163, #4809, #19425 ) ;
#3850 = ORIENTED_EDGE ( 'NONE', *, *, #8314, .T. ) ;
#3851 = CARTESIAN_POINT ( 'NONE',  ( 26.75643035624999655, -3.323476615752267271, -7.153124999385460647 ) ) ;
#3852 = CARTESIAN_POINT ( 'NONE',  ( 26.75643035624999655, 245.4343750006145228, 3.323476615752267715 ) ) ;
#3853 = CARTESIAN_POINT ( 'NONE',  ( 10.69584247140445221, 25.64768628210143930, -6.932735513423970097 ) ) ;
#3854 = EDGE_CURVE ( 'NONE', #31979, #9957, #26863, .T. ) ;
#3855 = CARTESIAN_POINT ( 'NONE',  ( -31.78794563604516554, 205.3262412349648116, 4.842901733360249317 ) ) ;
#3856 = CARTESIAN_POINT ( 'NONE',  ( 22.56230152254410370, 0.000000000000000000, -10.00000000000000000 ) ) ;
#3857 = CARTESIAN_POINT ( 'NONE',  ( -33.37127896937850124, 214.5309553116392749, 1.090244570138288127 ) ) ;
#3858 =( LENGTH_UNIT ( ) NAMED_UNIT ( * ) SI_UNIT ( .MILLI., .METRE. ) );
#3859 = MECHANICAL_DESIGN_GEOMETRIC_PRESENTATION_REPRESENTATION (  '', ( #825 ), #27462 ) ;
#3860 = CARTESIAN_POINT ( 'NONE',  ( 33.65960319901864040, 5.196152422706631135, 160.2787869599868316 ) ) ;
#3861 = CARTESIAN_POINT ( 'NONE',  ( 10.49813415416005213, 93.02731371789856496, -7.228626920338837358 ) ) ;
#3862 = CARTESIAN_POINT ( 'NONE',  ( -50.79538769728824121, 211.3212981617418222, -4.469044688360751749 ) ) ;
#3863 = AXIS2_PLACEMENT_3D ( 'NONE', #4306, #27809, #31209 ) ;
#3864 = CARTESIAN_POINT ( 'NONE',  ( -69.59747103062156270, 213.3500491399821328, -5.571401726697985168 ) ) ;
#3865 = CARTESIAN_POINT ( 'NONE',  ( 20.99999999999999645, -6.646953231504538984, -6.440624999385486937 ) ) ;
#3866 = DIRECTION ( 'NONE',  ( 1.000000000000000000, 0.000000000000000000, 0.000000000000000000 ) ) ;
#3867 = CARTESIAN_POINT ( 'NONE',  ( -14.38691631536193860, 62.26481371789854791, -5.770363421894132649 ) ) ;
#3868 = CARTESIAN_POINT ( 'NONE',  ( -40.29836230271183695, 202.5810206699313767, -4.149950860017804111 ) ) ;
#3869 = DIRECTION ( 'NONE',  ( 0.000000000000000000, 0.000000000000000000, 1.000000000000000000 ) ) ;
#3870 = CARTESIAN_POINT ( 'NONE',  ( -12.50000000000000355, 86.31018628210145494, -0.1745138560725492671 ) ) ;
#3871 = CARTESIAN_POINT ( 'NONE',  ( 3.257655550457285720, 33.69768628210143646, -15.46528703574804986 ) ) ;
#3872 = CARTESIAN_POINT ( 'NONE',  ( 10.56230152254411259, -3.464101615137761048, -0.8625000000000265787 ) ) ;
#3873 = CARTESIAN_POINT ( 'NONE',  ( 36.89654967657799745, 7.646167579472024665E-16, 160.0614665149821576 ) ) ;
#3874 = CARTESIAN_POINT ( 'NONE',  ( -11.08355503943142573, 57.56018628210145494, 10.83675517735155402 ) ) ;
#3875 = CARTESIAN_POINT ( 'NONE',  ( 27.24356964375000700, 197.2906250006145399, 15.72908226750537075 ) ) ;
#3876 = DIRECTION ( 'NONE',  ( 0.000000000000000000, 1.000000000000000000, 0.000000000000000000 ) ) ;
#3877 = CYLINDRICAL_SURFACE ( 'NONE', #6782, 5.999999999999999112 ) ;
#3878 = CARTESIAN_POINT ( 'NONE',  ( -32.38913769728823411, 206.8500491399821044, -5.686928522499717253 ) ) ;
#3879 = DIRECTION ( 'NONE',  ( -0.9925324990730152175, 0.1219804832088933616, 0.000000000000000000 ) ) ;
#3880 = CARTESIAN_POINT ( 'NONE',  ( 6.932735513423970097, 27.94768628210143646, 10.69584247140445044 ) ) ;
#3881 = CARTESIAN_POINT ( 'NONE',  ( 26.75643035624999655, 249.6343750006145399, -7.049594010296217766E-16 ) ) ;
#3882 = CARTESIAN_POINT ( 'NONE',  ( -0.1745138560723084320, 128.3898137178985621, -9.500000000000005329 ) ) ;
#3883 = CARTESIAN_POINT ( 'NONE',  ( 23.87821517812499650, 246.5593750006145228, -4.985214923628404904 ) ) ;
#3884 = ORIENTED_EDGE ( 'NONE', *, *, #7534, .T. ) ;
#3885 = CARTESIAN_POINT ( 'NONE',  ( 15.00000000000000178, -3.464101615137757051, -7.162499999999998757 ) ) ;
#3886 = STYLED_ITEM ( 'NONE', ( #27509 ), #20554 ) ;
#3887 = CARTESIAN_POINT ( 'NONE',  ( 0.000000000000000000, 200.0000000000000000, 0.000000000000000000 ) ) ;
#3888 = ADVANCED_FACE ( 'NONE', ( #15880 ), #14352, .T. ) ;
#3889 = CARTESIAN_POINT ( 'NONE',  ( -4.622313124798826500, 133.5648137178985735, 11.61527771782809637 ) ) ;
#3890 = CARTESIAN_POINT ( 'NONE',  ( 22.80587116629410716, 7.646167579472015790E-16, -5.765624999385543958 ) ) ;
#3891 = AXIS2_PLACEMENT_3D ( 'NONE', #8061, #2550, #6277 ) ;
#3892 = CARTESIAN_POINT ( 'NONE',  ( 37.17599277676264080, 7.646167579472015790E-16, 163.2555157657388065 ) ) ;
#3893 = DIRECTION ( 'NONE',  ( -0.000000000000000000, -1.000000000000000000, -0.000000000000000000 ) ) ;
#3894 = CARTESIAN_POINT ( 'NONE',  ( 13.50000000000001421, 199.2500000000000000, 23.38268590217984055 ) ) ;
#3895 = CARTESIAN_POINT ( 'NONE',  ( 2.660918448318279950, 52.09768628210144215, -12.46528703574805874 ) ) ;
#3896 = VERTEX_POINT ( 'NONE', #700 ) ;
#3897 = ORIENTED_EDGE ( 'NONE', *, *, #19583, .F. ) ;
#3898 = CARTESIAN_POINT ( 'NONE',  ( 1.120210788295102201E-13, 195.8375000000000057, -27.00000000000000711 ) ) ;
#3899 = CARTESIAN_POINT ( 'NONE',  ( 13.56230152254411792, -5.196152422706638241, -3.975000000000061817 ) ) ;
#3900 = FACE_OUTER_BOUND ( 'NONE', #18753, .T. ) ;
#3901 = CARTESIAN_POINT ( 'NONE',  ( 18.12178482187499640, 4.985214923628404904, -9.215624999385468641 ) ) ;
#3902 = CARTESIAN_POINT ( 'NONE',  ( -11.48171059495397373, 86.88518628210145778, -4.944772684328680334 ) ) ;
#3903 = CARTESIAN_POINT ( 'NONE',  ( 8.927990412390371944, 21.72731371789853938, 13.04141134922778811 ) ) ;
#3904 = CARTESIAN_POINT ( 'NONE',  ( 0.000000000000000000, 210.0000000000000284, 0.000000000000000000 ) ) ;
#3905 = CARTESIAN_POINT ( 'NONE',  ( 24.86380461455084756, 0.000000000000000000, 163.0057683059945930 ) ) ;
#3906 = CARTESIAN_POINT ( 'NONE',  ( -62.86086230271182984, 212.1499508600178387, -3.954877714930852495 ) ) ;
#3907 = CYLINDRICAL_SURFACE ( 'NONE', #14357, 2.649999999999992806 ) ;
#3908 = CARTESIAN_POINT ( 'NONE',  ( 31.26258870864309003, 6.928203230275506996, 167.3019257015274945 ) ) ;
#3909 = CARTESIAN_POINT ( 'NONE',  ( -5.529263428287297444, 7.927313717898536005, -7.954856959092311719 ) ) ;
#3910 = CARTESIAN_POINT ( 'NONE',  ( -49.21205436395490551, 214.6737587650352168, 4.842901733360204908 ) ) ;
#3911 = CARTESIAN_POINT ( 'NONE',  ( -69.00372103062157692, 218.5309553116391896, -2.162041339862839084 ) ) ;
#3912 = CONTEXT_DEPENDENT_SHAPE_REPRESENTATION ( #24330, #13792 ) ;
#3913 = CARTESIAN_POINT ( 'NONE',  ( 20.99999999999999289, 248.8187500012290911, 5.999999999999999112 ) ) ;
#3914 = CARTESIAN_POINT ( 'NONE',  ( 27.24356964374999635, 198.2656250006145058, -15.72908226750539029 ) ) ;
#3915 = CARTESIAN_POINT ( 'NONE',  ( -15.53471296425188442, 107.9773137178985394, -2.908627838312459080 ) ) ;
#3916 = CARTESIAN_POINT ( 'NONE',  ( -61.47544563604515133, 214.8429017333602360, 4.673758765035156415 ) ) ;
#3917 = ORIENTED_EDGE ( 'NONE', *, *, #30423, .T. ) ;
#3918 = CARTESIAN_POINT ( 'NONE',  ( -6.932735513423968321, 32.54768628210144499, -10.69584247140445221 ) ) ;
#3919 = DIRECTION ( 'NONE',  ( 1.000000000000000000, 0.000000000000000000, 0.000000000000000000 ) ) ;
#3920 = LINE ( 'NONE', #36312, #31394 ) ;
#3921 = CARTESIAN_POINT ( 'NONE',  ( 34.38148213269554532, 5.407089921784862696, 167.1325768043071776 ) ) ;
#3922 = CARTESIAN_POINT ( 'NONE',  ( 8.632099005475504683, 101.5476862821014663, 13.23911966647218996 ) ) ;
#3923 = CARTESIAN_POINT ( 'NONE',  ( -62.47247103062156981, 206.6499508600178672, 5.571401726697986057 ) ) ;
#3924 = CARTESIAN_POINT ( 'NONE',  ( 13.44051670066911264, 5.407089921784856479, -3.365624999385530280 ) ) ;
#3925 = CARTESIAN_POINT ( 'NONE',  ( -3.474262827703337830, 51.23518628210143788, -8.843639120294326972 ) ) ;
#3926 = EDGE_CURVE ( 'NONE', #13097, #35545, #6587, .T. ) ;
#3927 = DIRECTION ( 'NONE',  ( -1.000000000000000000, 0.000000000000000000, 0.000000000000000000 ) ) ;
#3928 = CARTESIAN_POINT ( 'NONE',  ( -34.96205436395489841, 216.1378603801730094, 6.307003348497944195 ) ) ;
#3929 = CARTESIAN_POINT ( 'NONE',  ( -14.50000000000000533, 237.0000000000000000, 2.500000000000000000 ) ) ;
#3930 = CARTESIAN_POINT ( 'NONE',  ( 10.49813415415989581, 73.37268628210144072, 7.228626920339068285 ) ) ;
#3931 = CARTESIAN_POINT ( 'NONE',  ( 0.000000000000000000, -20.00000000000000000, 0.000000000000000000 ) ) ;
#3932 = DIRECTION ( 'NONE',  ( 0.9925324990730152175, -0.1219804832088933616, 0.000000000000000000 ) ) ;
#3933 = CARTESIAN_POINT ( 'NONE',  ( 9.534712964251941258, 44.62268628210144783, -1.715153634034235708 ) ) ;
#3934 = CARTESIAN_POINT ( 'NONE',  ( 33.79808337967844523, 5.407089921784857367, 160.4642985439555218 ) ) ;
#3935 = CARTESIAN_POINT ( 'NONE',  ( 21.00000000000000000, -6.646953231504538984, -9.028124999385470417 ) ) ;
#3936 = CARTESIAN_POINT ( 'NONE',  ( -7.234628195640289583, 198.2200961906613372, -27.00000000000001421 ) ) ;
#3937 = CARTESIAN_POINT ( 'NONE',  ( 28.05054758442196672, 5.407089921784862696, 166.4065915139379115 ) ) ;
#3938 = CARTESIAN_POINT ( 'NONE',  ( 24.92917142150447063, 3.464101615137757051, 163.7529143283390169 ) ) ;
#3939 = CARTESIAN_POINT ( 'NONE',  ( 18.00000000000000000, 244.9749999999999943, -5.196152422706630247 ) ) ;
#3940 = CARTESIAN_POINT ( 'NONE',  ( -13.62178482187498396, 195.3781250006145171, 23.59362340125808188 ) ) ;
#3941 = ADVANCED_FACE ( 'NONE', ( #18546 ), #26670, .F. ) ;
#3942 = CARTESIAN_POINT ( 'NONE',  ( 4.944772684328420986, 104.8148137178985593, 11.48171059495408208 ) ) ;
#3943 = CARTESIAN_POINT ( 'NONE',  ( 12.46528703574805874, 109.5976862821014493, 2.660918448318279950 ) ) ;
#3944 = ORIENTED_EDGE ( 'NONE', *, *, #27886, .F. ) ;
#3945 = ORIENTED_EDGE ( 'NONE', *, *, #11087, .F. ) ;
#3946 = CARTESIAN_POINT ( 'NONE',  ( 13.49999999999999645, 199.5125000012290286, -23.38268590217984766 ) ) ;
#3947 = CARTESIAN_POINT ( 'NONE',  ( 26.75643035624999655, 240.5593750006145513, -3.323476615752271712 ) ) ;
#3948 = CARTESIAN_POINT ( 'NONE',  ( 8.927990412390371944, 76.92731371789854222, 13.04141134922778811 ) ) ;
#3949 = CARTESIAN_POINT ( 'NONE',  ( 18.12178482187499640, 4.985214923628404904, -7.078124999385481786 ) ) ;
#3950 = AXIS2_PLACEMENT_3D ( 'NONE', #1501, #4347, #32971 ) ;
#3951 = CARTESIAN_POINT ( 'NONE',  ( 21.00000000000000000, 245.4718750006145456, 6.646953231504538984 ) ) ;
#3952 = CARTESIAN_POINT ( 'NONE',  ( 6.840914352312096547, 98.96018628210144641, -6.594114490232313663 ) ) ;
#3953 = CARTESIAN_POINT ( 'NONE',  ( -27.00000000000000355, 195.1625000012290343, 0.000000000000000000 ) ) ;
#3954 = CARTESIAN_POINT ( 'NONE',  ( 8.710071997420211432, 56.51481371789856212, -3.796722387233181895 ) ) ;
#3955 = CARTESIAN_POINT ( 'NONE',  ( 13.44051670066911264, 5.407089921784856479, -5.615624999385532057 ) ) ;
#3956 =( BOUNDED_CURVE ( )  B_SPLINE_CURVE ( 2, ( #12177, #35290, #9346, #20917, #22226, #10278, #25242 ),
 .UNSPECIFIED., .F., .F. ) 
 B_SPLINE_CURVE_WITH_KNOTS ( ( 3, 2, 2, 3 ),
 ( 0.8478260869565228397, 0.8550724637681171858, 0.8623188405797115319, 0.8695652173913057670 ),
 .UNSPECIFIED. ) 
 CURVE ( )  GEOMETRIC_REPRESENTATION_ITEM ( )  RATIONAL_B_SPLINE_CURVE ( ( 0.9999999999999794609, 0.8660254037844592467, 1.000000000000000000, 0.8660254037844387076, 1.000000000000000000, 0.8660254037844120623, 1.000000000000026645 ) ) 
 REPRESENTATION_ITEM ( '' )  );
#3957 = CARTESIAN_POINT ( 'NONE',  ( -6.840914352311947333, 118.0398137178985536, -6.594114490232462877 ) ) ;
#3958 = CYLINDRICAL_SURFACE ( 'NONE', #2839, 6.000000000000001776 ) ;
#3959 = CARTESIAN_POINT ( 'NONE',  ( -2.311890736173448424, 32.07731371789855501, 12.53471296425189330 ) ) ;
#3960 = CARTESIAN_POINT ( 'NONE',  ( 15.00000000000063771, -3.464101615138124757, -3.112499999999997158 ) ) ;
#3961 = CARTESIAN_POINT ( 'NONE',  ( -7.228626920339069173, 75.67268628210146630, 10.49813415415989581 ) ) ;
#3962 = CARTESIAN_POINT ( 'NONE',  ( 10.56230152254410726, 3.464101615137752166, -5.774999998771017218 ) ) ;
#3963 = FACE_OUTER_BOUND ( 'NONE', #10758, .T. ) ;
#3964 = CARTESIAN_POINT ( 'NONE',  ( 27.91164311941789933, -5.407089921784859143, 164.8189062138541772 ) ) ;
#3965 = CARTESIAN_POINT ( 'NONE',  ( 22.80587116629412137, 7.646167579472024665E-16, -4.471874999385533123 ) ) ;
#3966 = FILL_AREA_STYLE_COLOUR ( '', #25 ) ;
#3967 = DIRECTION ( 'NONE',  ( -0.1219804832088933616, -0.9925324990730152175, 0.000000000000000000 ) ) ;
#3968 = CARTESIAN_POINT ( 'NONE',  ( 1.069080835302379631E-14, 198.3124999999999716, 27.00000000000000000 ) ) ;
#3969 = CARTESIAN_POINT ( 'NONE',  ( -7.954856959092191815, 105.5726862821014294, -5.529263428287477744 ) ) ;
#3970 = CARTESIAN_POINT ( 'NONE',  ( 26.99999999999999645, 199.0250000012290172, -15.58845726811990495 ) ) ;
#3971 =( BOUNDED_SURFACE ( )  B_SPLINE_SURFACE ( 1, 2, ( 
 ( #4071, #21527, #18305, #29845, #30037, #23988, #3881, #15455, #21340, #27007, #29659, #15643, #3695, #18688, #27193, #1218, #24360, #35903, #9946, #33073, #7117, #4255, #15831, #27379, #1409, #34185, #33997, #30790, #16760, #37018, #13541, #22266, #16207, #24908, #10502, #13167, #27938, #4627, #8230, #8041, #11064, #27755, #33819, #4813, #7857, #25094, #22638, #28307, #36651, #10877, #2346, #19429, #36273, #31340, #13735, #21891, #22450, #2154, #36460, #16393, #10688, #19805, #19059, #1599, #30979, #4997, #28124, #19617, #5367, #25283, #10318, #30611, #33440, #36834, #19250, #1785, #16579, #16946, #13918, #31163, #24722, #7481, #33632, #13353, #5186, #22080, #25468, #7671, #1968, #8781, #20162, #25835, #17504, #31895, #28859, #2893, #14652, #17693, #11435, #17317, #11991, #6111, #20539, #5924, #26393, #23190, #14466, #2708, #3083, #11615, #23002, #28488, #23563, #5549, #17134, #9156, #26020, #34551, #3272, #28670, #37203, #14098, #37383, #426, #20353, #14284, #20723, #8591, #31710, #34738, #29039, #5737, #32267, #29232, #35108, #32082, #14845, #48, #26203, #31523, #11804, #240, #6310, #2532, #23374, #34923, #25650, #8967, #11250, #22820, #34369, #8412, #19981, #33544, #16306, #30331, #1511, #32980, #4174, #27295, #29427, #7218, #20918, #13457, #13270, #27853, #7034, #13085, #10046, #24639, #4355, #1886, #7586, #15935, #27671, #19162, #36190, #15031, #10604, #30525, #609, #1697, #18970, #15744, #21623, #27484, #25007, #35291, #17882, #10234, #21809, #7398, #24823, #36563, #4545, #26580, #9347, #12178, #16121, #36008, #18601, #33362, #22184, #30711, #36376, #33732, #23752, #12894, #30144, #10422, #1326, #21997, #4731, #24459, #3461, #33174, #18790, #34291, #11168, #8150, #19722, #31445, #34472, #28229, #34100, #28775, #22927, #37306, #22741, #5654, #2444, #31262, #19532, #19904, #28405, #2258, #7773, #2815, #22368, #33916, #25943, #5288, #13837, #20082, #7958, #16494, #30890, #16682, #17236, #37120, #31080, #37486, #5103, #25384, #14018, #25568, #36934, #11537, #8515, #14385, #11356, #31626, #10980, #8334, #10795, #28588, #16868, #23108, #19351 ),
 ( #36754, #4913, #22551, #5468, #17050, #28042, #2075, #2626, #14202, #13648, #25753, #25201, #26875, #9260, #17424, #6412, #35210, #20458, #343, #20642, #18175, #14572, #34652, #29339, #32189, #23666, #3570, #15324, #20832, #5846, #26124, #28963, #32374, #14761, #156, #6223, #32559, #35397, #17796, #6601, #3002, #29145, #34840, #15131, #17615, #17987, #29530, #31999, #14946, #26306, #6029, #26683, #525, #35028, #9072, #713, #23858, #3186, #23475, #29716, #12285, #9445, #12092, #3749, #3377, #26493, #8880, #21024, #906, #11908, #8696, #12476, #11721, #23295, #20270, #31809, #18559, #36334, #24231, #32750, #9634, #32937, #21955, #15894, #1094, #16268, #12663, #4133, #30290, #4315, #30101, #4686, #13234, #33501, #27630, #10380, #35775, #24600, #27070, #7359, #21585, #1845, #27817, #35966, #10004, #21211, #27439, #7546, #18361, #15705, #24044, #15514, #19118, #18931, #27256, #1660, #30668, #33132, #7175, #9819, #21396, #6991, #35589, #12850, #1279, #6787, #30484, #29910, #24418, #18748, #1471, #13045, #24783, #36150, #3939, #10193, #21769, #33319, #4504, #16081, #36713, #25712, #31405, #10565, #37265, #5424, #2402, #2215, #10940, #25344, #22142, #22880, #13797, #4875, #8468, #20038, #19680, #5248, #22703, #7919, #33877, #8106, #25158, #19493, #31039, #36893, #5061, #28732, #22513, #24963, #19862, #31219, #13977, #16825, #28367, #33688, #31584, #34060, #17005, #17192, #2588, #34247, #19312, #25527, #13415, #37080, #11126, #36521, #7729, #14158, #30850, #11312, #16454, #28184, #10752, #27998, #13609, #34431, #8290, #28546, #2031, #5608, #22325, #16643, #8652, #23249, #31767, #12235, #3328, #14899, #6553, #20975, #34795, #3517, #20595, #29100, #17565, #23063, #3143, #12047, #26259, #20782, #2956, #295, #20221, #17378, #26447, #26081, #11860, #480, #35162, #32136, #5798, #9211, #11494, #20411, #35347, #663, #28921, #18126, #17748, #9400, #14711, #2770, #15084, #8839, #32508, #14343, #25897, #34609, #31953, #37445, #32325, #23617, #29480, #5985, #14525, #6365, #17936, #110, #26634, #11674, #23429, #34981, #23806, #9023, #6176, #29289, #27579 ) ),
 .UNSPECIFIED., .F., .F., .F. ) 
 B_SPLINE_SURFACE_WITH_KNOTS ( ( 2, 2 ),
 ( 3, 2, 2, 2, 2, 2, 2, 2, 2, 2, 2, 2, 2, 2, 2, 2, 2, 2, 2, 2, 2, 2, 2, 2, 2, 2, 2, 2, 2, 2, 2, 2, 2, 2, 2, 2, 2, 2, 2, 2, 2, 2, 2, 2, 2, 2, 2, 2, 2, 2, 2, 2, 2, 2, 2, 2, 2, 2, 2, 2, 2, 2, 2, 2, 2, 2, 2, 2, 2, 2, 2, 2, 2, 2, 2, 2, 2, 2, 2, 2, 2, 2, 2, 2, 2, 2, 2, 2, 2, 2, 2, 2, 2, 2, 2, 2, 2, 2, 2, 2, 2, 2, 2, 2, 2, 2, 2, 2, 2, 2, 2, 2, 2, 2, 2, 2, 2, 2, 2, 2, 2, 2, 2, 2, 2, 2, 2, 2, 2, 2, 2, 2, 2, 2, 3 ),
 ( 0.000000000000000000, 1.000000000000000000 ),
 ( 0.000000000000000000, 0.007246376811594202987, 0.01449275362318840597, 0.02173913043478260809, 0.02898550724637681195, 0.03623188405797101580, 0.04347826086956521618, 0.05072463768115942351, 0.05797101449275362389, 0.06521739130434782428, 0.07246376811594203160, 0.07971014492753622505, 0.08695652173913043237, 0.09420289855072463969, 0.1014492753623188470, 0.1086956521739130405, 0.1159420289855072478, 0.1231884057971014551, 0.1304347826086956486, 0.1376811594202898559, 0.1449275362318840632, 0.1521739130434782705, 0.1594202898550724501, 0.1666666666666666574, 0.1739130434782608647, 0.1811594202898550721, 0.1884057971014492794, 0.1956521739130434867, 0.2028985507246376940, 0.2101449275362318736, 0.2173913043478260809, 0.2246376811594202882, 0.2318840579710144956, 0.2391304347826087029, 0.2463768115942029102, 0.2536231884057971175, 0.2608695652173912971, 0.2681159420289855322, 0.2753623188405797118, 0.2826086956521738913, 0.2898550724637681264, 0.2971014492753623060, 0.3043478260869565410, 0.3115942028985507206, 0.3188405797101449002, 0.3260869565217391353, 0.3333333333333333148, 0.3405797101449275499, 0.3478260869565217295, 0.3550724637681159646, 0.3623188405797101441, 0.3695652173913043237, 0.3768115942028985588, 0.3840579710144927383, 0.3913043478260869734, 0.3985507246376811530, 0.4057971014492753881, 0.4130434782608695676, 0.4202898550724637472, 0.4275362318840579823, 0.4347826086956521618, 0.4420289855072463969, 0.4492753623188405765, 0.4565217391304347561, 0.4637681159420289911, 0.4710144927536231707, 0.4782608695652174058, 0.4855072463768115854, 0.4927536231884058204, 0.5000000000000000000, 0.5072463768115942351, 0.5144927536231883591, 0.5217391304347825942, 0.5289855072463768293, 0.5362318840579710644, 0.5434782608695651884, 0.5507246376811594235, 0.5579710144927536586, 0.5652173913043477826, 0.5724637681159420177, 0.5797101449275362528, 0.5869565217391304879, 0.5942028985507246119, 0.6014492753623188470, 0.6086956521739130821, 0.6159420289855072062, 0.6231884057971014412, 0.6304347826086956763, 0.6376811594202898004, 0.6449275362318840354, 0.6521739130434782705, 0.6594202898550725056, 0.6666666666666666297, 0.6739130434782608647, 0.6811594202898550998, 0.6884057971014492239, 0.6956521739130434590, 0.7028985507246376940, 0.7101449275362319291, 0.7173913043478260532, 0.7246376811594202882, 0.7318840579710145233, 0.7391304347826086474, 0.7463768115942028825, 0.7536231884057971175, 0.7608695652173913526, 0.7681159420289854767, 0.7753623188405797118, 0.7826086956521739468, 0.7898550724637680709, 0.7971014492753623060, 0.8043478260869565410, 0.8115942028985507761, 0.8188405797101449002, 0.8260869565217391353, 0.8333333333333333703, 0.8405797101449274944, 0.8478260869565217295, 0.8550724637681159646, 0.8623188405797101996, 0.8695652173913043237, 0.8768115942028985588, 0.8840579710144927938, 0.8913043478260869179, 0.8985507246376811530, 0.9057971014492753881, 0.9130434782608695121, 0.9202898550724637472, 0.9275362318840579823, 0.9347826086956522174, 0.9420289855072463414, 0.9492753623188405765, 0.9565217391304348116, 0.9637681159420289356, 0.9662082973083874204 ),
 .UNSPECIFIED. ) 
 GEOMETRIC_REPRESENTATION_ITEM ( )  RATIONAL_B_SPLINE_SURFACE ( (
 ( 1.000000000000000000, 0.8660254037844387076, 1.000000000000000000, 0.8660254037844387076, 1.000000000000000000, 0.8660254037844387076, 1.000000000000000000, 0.8660254037844387076, 1.000000000000000000, 0.8660254037844387076, 1.000000000000000000, 0.8660254037844387076, 1.000000000000000000, 0.8660254037844387076, 1.000000000000000000, 0.8660254037844387076, 1.000000000000000000, 0.8660254037844387076, 1.000000000000000000, 0.8660254037844387076, 1.000000000000000000, 0.8660254037844387076, 1.000000000000000000, 0.8660254037844387076, 1.000000000000000000, 0.8660254037844387076, 1.000000000000000000, 0.8660254037844387076, 1.000000000000000000, 0.8660254037844387076, 1.000000000000000000, 0.8660254037844387076, 1.000000000000000000, 0.8660254037844387076, 1.000000000000000000, 0.8660254037844387076, 1.000000000000000000, 0.8660254037844387076, 1.000000000000000000, 0.8660254037844387076, 1.000000000000000000, 0.8660254037844387076, 1.000000000000000000, 0.8660254037844387076, 1.000000000000000000, 0.8660254037844387076, 1.000000000000000000, 0.8660254037844387076, 1.000000000000000000, 0.8660254037844387076, 1.000000000000000000, 0.8660254037844387076, 1.000000000000000000, 0.8660254037844387076, 1.000000000000000000, 0.8660254037844387076, 1.000000000000000000, 0.8660254037844387076, 1.000000000000000000, 0.8660254037844387076, 1.000000000000000000, 0.8660254037844387076, 1.000000000000000000, 0.8660254037844387076, 1.000000000000000000, 0.8660254037844387076, 1.000000000000000000, 0.8660254037844387076, 1.000000000000000000, 0.8660254037844387076, 1.000000000000000000, 0.8660254037844387076, 1.000000000000000000, 0.8660254037844387076, 1.000000000000000000, 0.8660254037844387076, 1.000000000000000000, 0.8660254037844387076, 1.000000000000000000, 0.8660254037844387076, 1.000000000000000000, 0.8660254037844387076, 1.000000000000000000, 0.8660254037844387076, 1.000000000000000000, 0.8660254037844387076, 1.000000000000000000, 0.8660254037844387076, 1.000000000000000000, 0.8660254037844387076, 1.000000000000000000, 0.8660254037844387076, 1.000000000000000000, 0.8660254037844387076, 1.000000000000000000, 0.8660254037844387076, 1.000000000000000000, 0.8660254037844387076, 1.000000000000000000, 0.8660254037844387076, 1.000000000000000000, 0.8660254037844387076, 1.000000000000000000, 0.8660254037844387076, 1.000000000000000000, 0.8660254037844387076, 1.000000000000000000, 0.8660254037844387076, 1.000000000000000000, 0.8660254037844387076, 1.000000000000000000, 0.8660254037844387076, 1.000000000000000000, 0.8660254037844387076, 1.000000000000000000, 0.8660254037844387076, 1.000000000000000000, 0.8660254037844387076, 1.000000000000000000, 0.8660254037844387076, 1.000000000000000000, 0.8660254037844387076, 1.000000000000000000, 0.8660254037844387076, 1.000000000000000000, 0.8660254037844387076, 1.000000000000000000, 0.8660254037844387076, 1.000000000000000000, 0.8660254037844387076, 1.000000000000000000, 0.8660254037844387076, 1.000000000000000000, 0.8660254037844387076, 1.000000000000000000, 0.8660254037844387076, 1.000000000000000000, 0.8660254037844387076, 1.000000000000000000, 0.8660254037844387076, 1.000000000000000000, 0.8660254037844387076, 1.000000000000000000, 0.8660254037844387076, 1.000000000000000000, 0.8660254037844387076, 1.000000000000000000, 0.8660254037844387076, 1.000000000000000000, 0.8660254037844387076, 1.000000000000000000, 0.8660254037844387076, 1.000000000000000000, 0.8660254037844387076, 1.000000000000000000, 0.8660254037844387076, 1.000000000000000000, 0.8660254037844387076, 1.000000000000000000, 0.8660254037844387076, 1.000000000000000000, 0.8660254037844387076, 1.000000000000000000, 0.8660254037844387076, 1.000000000000000000, 0.8660254037844387076, 1.000000000000000000, 0.8660254037844387076, 1.000000000000000000, 0.8660254037844387076, 1.000000000000000000, 0.8660254037844387076, 1.000000000000000000, 0.8660254037844387076, 1.000000000000000000, 0.8660254037844387076, 1.000000000000000000, 0.8660254037844387076, 1.000000000000000000, 0.8660254037844387076, 1.000000000000000000, 0.8660254037844387076, 1.000000000000000000, 0.8660254037844387076, 1.000000000000000000, 0.8660254037844387076, 1.000000000000000000, 0.8660254037844387076, 1.000000000000000000, 0.8660254037844387076, 1.000000000000000000, 0.8660254037844387076, 1.000000000000000000, 0.8660254037844387076, 1.000000000000000000, 0.8660254037844387076, 1.000000000000000000, 0.8660254037844387076, 1.000000000000000000, 0.8660254037844387076, 1.000000000000000000, 0.8660254037844387076, 1.000000000000000000, 0.8660254037844387076, 1.000000000000000000, 0.8660254037844387076, 1.000000000000000000, 0.8660254037844387076, 1.000000000000000000, 0.8660254037844387076, 1.000000000000000000, 0.8660254037844387076, 1.000000000000000000, 0.8660254037844387076, 1.000000000000000000, 0.8660254037844387076, 1.000000000000000000, 0.8660254037844387076, 1.000000000000000000, 0.8660254037844387076, 1.000000000000000000, 0.8660254037844387076, 1.000000000000000000, 0.8660254037844387076, 1.000000000000000000, 0.8660254037844387076, 1.000000000000000000, 0.8660254037844387076, 1.000000000000000000, 0.8660254037844387076, 1.000000000000000000, 0.8660254037844387076, 1.000000000000000000, 0.8660254037844387076, 1.000000000000000000, 0.8660254037844387076, 1.000000000000000000, 0.8660254037844387076, 1.000000000000000000, 0.8660254037844387076, 1.000000000000000000, 0.8660254037844387076, 1.000000000000000000, 0.8660254037844387076, 1.000000000000000000, 0.8660254037844387076, 1.000000000000000000, 0.8660254037844387076, 1.000000000000000000, 0.8660254037844387076, 1.000000000000000000, 0.8660254037844387076, 1.000000000000000000, 0.8660254037844387076, 1.000000000000000000, 0.8660254037844387076, 1.000000000000000000, 0.8660254037844387076, 1.000000000000000000, 0.8660254037844387076, 1.000000000000000000, 0.8660254037844387076, 1.000000000000000000, 0.8660254037844387076, 1.000000000000000000, 0.8660254037844387076, 1.000000000000000000, 0.9548847207714155072, 0.9401541335272467492),
 ( 1.000000000000000000, 0.8660254037844387076, 1.000000000000000000, 0.8660254037844387076, 1.000000000000000000, 0.8660254037844387076, 1.000000000000000000, 0.8660254037844387076, 1.000000000000000000, 0.8660254037844387076, 1.000000000000000000, 0.8660254037844387076, 1.000000000000000000, 0.8660254037844387076, 1.000000000000000000, 0.8660254037844387076, 1.000000000000000000, 0.8660254037844387076, 1.000000000000000000, 0.8660254037844387076, 1.000000000000000000, 0.8660254037844387076, 1.000000000000000000, 0.8660254037844387076, 1.000000000000000000, 0.8660254037844387076, 1.000000000000000000, 0.8660254037844387076, 1.000000000000000000, 0.8660254037844387076, 1.000000000000000000, 0.8660254037844387076, 1.000000000000000000, 0.8660254037844387076, 1.000000000000000000, 0.8660254037844387076, 1.000000000000000000, 0.8660254037844387076, 1.000000000000000000, 0.8660254037844387076, 1.000000000000000000, 0.8660254037844387076, 1.000000000000000000, 0.8660254037844387076, 1.000000000000000000, 0.8660254037844387076, 1.000000000000000000, 0.8660254037844387076, 1.000000000000000000, 0.8660254037844387076, 1.000000000000000000, 0.8660254037844387076, 1.000000000000000000, 0.8660254037844387076, 1.000000000000000000, 0.8660254037844387076, 1.000000000000000000, 0.8660254037844387076, 1.000000000000000000, 0.8660254037844387076, 1.000000000000000000, 0.8660254037844387076, 1.000000000000000000, 0.8660254037844387076, 1.000000000000000000, 0.8660254037844387076, 1.000000000000000000, 0.8660254037844387076, 1.000000000000000000, 0.8660254037844387076, 1.000000000000000000, 0.8660254037844387076, 1.000000000000000000, 0.8660254037844387076, 1.000000000000000000, 0.8660254037844387076, 1.000000000000000000, 0.8660254037844387076, 1.000000000000000000, 0.8660254037844387076, 1.000000000000000000, 0.8660254037844387076, 1.000000000000000000, 0.8660254037844387076, 1.000000000000000000, 0.8660254037844387076, 1.000000000000000000, 0.8660254037844387076, 1.000000000000000000, 0.8660254037844387076, 1.000000000000000000, 0.8660254037844387076, 1.000000000000000000, 0.8660254037844387076, 1.000000000000000000, 0.8660254037844387076, 1.000000000000000000, 0.8660254037844387076, 1.000000000000000000, 0.8660254037844387076, 1.000000000000000000, 0.8660254037844387076, 1.000000000000000000, 0.8660254037844387076, 1.000000000000000000, 0.8660254037844387076, 1.000000000000000000, 0.8660254037844387076, 1.000000000000000000, 0.8660254037844387076, 1.000000000000000000, 0.8660254037844387076, 1.000000000000000000, 0.8660254037844387076, 1.000000000000000000, 0.8660254037844387076, 1.000000000000000000, 0.8660254037844387076, 1.000000000000000000, 0.8660254037844387076, 1.000000000000000000, 0.8660254037844387076, 1.000000000000000000, 0.8660254037844387076, 1.000000000000000000, 0.8660254037844387076, 1.000000000000000000, 0.8660254037844387076, 1.000000000000000000, 0.8660254037844387076, 1.000000000000000000, 0.8660254037844387076, 1.000000000000000000, 0.8660254037844387076, 1.000000000000000000, 0.8660254037844387076, 1.000000000000000000, 0.8660254037844387076, 1.000000000000000000, 0.8660254037844387076, 1.000000000000000000, 0.8660254037844387076, 1.000000000000000000, 0.8660254037844387076, 1.000000000000000000, 0.8660254037844387076, 1.000000000000000000, 0.8660254037844387076, 1.000000000000000000, 0.8660254037844387076, 1.000000000000000000, 0.8660254037844387076, 1.000000000000000000, 0.8660254037844387076, 1.000000000000000000, 0.8660254037844387076, 1.000000000000000000, 0.8660254037844387076, 1.000000000000000000, 0.8660254037844387076, 1.000000000000000000, 0.8660254037844387076, 1.000000000000000000, 0.8660254037844387076, 1.000000000000000000, 0.8660254037844387076, 1.000000000000000000, 0.8660254037844387076, 1.000000000000000000, 0.8660254037844387076, 1.000000000000000000, 0.8660254037844387076, 1.000000000000000000, 0.8660254037844387076, 1.000000000000000000, 0.8660254037844387076, 1.000000000000000000, 0.8660254037844387076, 1.000000000000000000, 0.8660254037844387076, 1.000000000000000000, 0.8660254037844387076, 1.000000000000000000, 0.8660254037844387076, 1.000000000000000000, 0.8660254037844387076, 1.000000000000000000, 0.8660254037844387076, 1.000000000000000000, 0.8660254037844387076, 1.000000000000000000, 0.8660254037844387076, 1.000000000000000000, 0.8660254037844387076, 1.000000000000000000, 0.8660254037844387076, 1.000000000000000000, 0.8660254037844387076, 1.000000000000000000, 0.8660254037844387076, 1.000000000000000000, 0.8660254037844387076, 1.000000000000000000, 0.8660254037844387076, 1.000000000000000000, 0.8660254037844387076, 1.000000000000000000, 0.8660254037844387076, 1.000000000000000000, 0.8660254037844387076, 1.000000000000000000, 0.8660254037844387076, 1.000000000000000000, 0.8660254037844387076, 1.000000000000000000, 0.8660254037844387076, 1.000000000000000000, 0.8660254037844387076, 1.000000000000000000, 0.8660254037844387076, 1.000000000000000000, 0.8660254037844387076, 1.000000000000000000, 0.8660254037844387076, 1.000000000000000000, 0.8660254037844387076, 1.000000000000000000, 0.8660254037844387076, 1.000000000000000000, 0.8660254037844387076, 1.000000000000000000, 0.8660254037844387076, 1.000000000000000000, 0.8660254037844387076, 1.000000000000000000, 0.8660254037844387076, 1.000000000000000000, 0.8660254037844387076, 1.000000000000000000, 0.8660254037844387076, 1.000000000000000000, 0.8660254037844387076, 1.000000000000000000, 0.8660254037844387076, 1.000000000000000000, 0.8660254037844387076, 1.000000000000000000, 0.8660254037844387076, 1.000000000000000000, 0.8660254037844387076, 1.000000000000000000, 0.8660254037844387076, 1.000000000000000000, 0.8660254037844387076, 1.000000000000000000, 0.8660254037844387076, 1.000000000000000000, 0.8660254037844387076, 1.000000000000000000, 0.8660254037844387076, 1.000000000000000000, 0.8660254037844387076, 1.000000000000000000, 0.8660254037844387076, 1.000000000000000000, 0.8660254037844387076, 1.000000000000000000, 0.9548847207714155072, 0.9401541335272467492) ) ) 
 REPRESENTATION_ITEM ( '' )  SURFACE ( )  );
#3972 = CARTESIAN_POINT ( 'NONE',  ( -6.932735513423968321, 133.7476862821014549, -10.69584247140445221 ) ) ;
#3973 = CARTESIAN_POINT ( 'NONE',  ( -27.24356964374999635, 196.7468750006145797, 15.72908226750539384 ) ) ;
#3974 = CARTESIAN_POINT ( 'NONE',  ( 26.75643035624999655, 240.0343750006145740, 3.323476615752267715 ) ) ;
#3975 = VERTEX_POINT ( 'NONE', #35384 ) ;
#3976 = CARTESIAN_POINT ( 'NONE',  ( 25.10569328411516921, 3.604726614523236616, 168.5652166982980305 ) ) ;
#3977 = CARTESIAN_POINT ( 'NONE',  ( 26.75643035624999655, 3.323476615752271712, -3.028124999385441107 ) ) ;
#3978 = CARTESIAN_POINT ( 'NONE',  ( 16.56230152254411081, -6.928203230275506996, -5.174999998771001586 ) ) ;
#3979 = DIRECTION ( 'NONE',  ( -1.000000000000000000, 0.000000000000000000, 0.000000000000000000 ) ) ;
#3980 = CARTESIAN_POINT ( 'NONE',  ( 26.99999999999999645, 7.347880794884117764E-16, -2.475000000000004974 ) ) ;
#3981 = CARTESIAN_POINT ( 'NONE',  ( 18.00000000000000000, 5.196152422706630247, -3.168749998770953091 ) ) ;
#3982 = CARTESIAN_POINT ( 'NONE',  ( 27.00000000000000355, 198.4250000000000114, -3.306546357697854128E-15 ) ) ;
#3983 = CARTESIAN_POINT ( 'NONE',  ( -8.843639120294245259, 16.26481371789853370, -3.474262827703533230 ) ) ;
#3984 = CARTESIAN_POINT ( 'NONE',  ( -13.62178482187498396, 198.1343750006145399, 23.59362340125808188 ) ) ;
#3986 = ORIENTED_EDGE ( 'NONE', *, *, #19589, .F. ) ;
#3985 = VERTEX_POINT ( 'NONE', #18734 ) ;
#3987 = CARTESIAN_POINT ( 'NONE',  ( 15.24356964374999990, 246.5968750006145171, 0.000000000000000000 ) ) ;
#3988 = CARTESIAN_POINT ( 'NONE',  ( -10.69584247140429412, 16.55231371789855999, -6.932735513424201024 ) ) ;
#3989 = CARTESIAN_POINT ( 'NONE',  ( 26.75643035624999655, -3.323476615752267715, -2.653124999385471305 ) ) ;
#3990 = CARTESIAN_POINT ( 'NONE',  ( -13.04141134922778456, 125.2273137178985394, 8.927990412390377273 ) ) ;
#3991 = CARTESIAN_POINT ( 'NONE',  ( 18.00000000000000355, -5.196152422706632912, -10.21874999877095469 ) ) ;
#3992 = CARTESIAN_POINT ( 'NONE',  ( 20.99999999999999645, 202.0000000000000000, 0.000000000000000000 ) ) ;
#3993 = ORIENTED_EDGE ( 'NONE', *, *, #36975, .T. ) ;
#3994 = CARTESIAN_POINT ( 'NONE',  ( 13.44051670066911441, -5.407089921784865361, -6.421874999385540406 ) ) ;
#3995 = EDGE_LOOP ( 'NONE', ( #16459, #23432, #36012, #20738 ) ) ;
#3996 = CARTESIAN_POINT ( 'NONE',  ( 27.24356964374999635, 196.0156250006145626, -15.72908226750539029 ) ) ;
#3997 = CARTESIAN_POINT ( 'NONE',  ( 4.944772684328679446, 125.9851862821014521, -11.48171059495397373 ) ) ;
#3998 = CARTESIAN_POINT ( 'NONE',  ( 37.17109026623309376, 7.646167579472024665E-16, 163.1994798139711520 ) ) ;
#3999 = CIRCLE ( 'NONE', #28217, 2.649999999999999467 ) ;
#4000 = CARTESIAN_POINT ( 'NONE',  ( -55.73586230271182984, 205.8500491399821613, 7.418979330068642852 ) ) ;
#4001 = CARTESIAN_POINT ( 'NONE',  ( 18.12178482187499640, 246.0718750006145115, -4.985214923628404904 ) ) ;
#4002 = CARTESIAN_POINT ( 'NONE',  ( 16.56230152254411081, -6.928203230275506996, -9.674999998771022902 ) ) ;
#4003 = CARTESIAN_POINT ( 'NONE',  ( -48.80877896937850124, 211.0902445701383101, -4.530955311639234040 ) ) ;
#4005 = EDGE_CURVE ( 'NONE', #19287, #15548, #15251, .T. ) ;
#4004 = DIRECTION ( 'NONE',  ( -0.000000000000000000, -0.000000000000000000, -1.000000000000000000 ) ) ;
#4006 = CARTESIAN_POINT ( 'NONE',  ( 28.18618370907300275, -5.407089921784859143, 167.9569195128432000 ) ) ;
#4007 = ORIENTED_EDGE ( 'NONE', *, *, #23768, .F. ) ;
#4008 = CARTESIAN_POINT ( 'NONE',  ( 20.99999999999998579, 247.9187500012290002, 5.999999999999998224 ) ) ;
#4009 = CARTESIAN_POINT ( 'NONE',  ( -13.23911966647218463, 140.6476862821014322, 8.632099005475506459 ) ) ;
#4010 = CARTESIAN_POINT ( 'NONE',  ( -46.63913769728824121, 205.8500491399820760, -7.418979330068584233 ) ) ;
#4011 =( BOUNDED_CURVE ( )  B_SPLINE_CURVE ( 2, ( #22876, #17188, #290, #5603, #11856, #34977, #8835 ),
 .UNSPECIFIED., .F., .F. ) 
 B_SPLINE_CURVE_WITH_KNOTS ( ( 3, 2, 2, 3 ),
 ( 0.2826086956521731142, 0.2898550724637674603, 0.2971014492753617509, 0.3043478260869560970 ),
 .UNSPECIFIED. ) 
 CURVE ( )  GEOMETRIC_REPRESENTATION_ITEM ( )  RATIONAL_B_SPLINE_CURVE ( ( 1.000000000000014433, 0.8660254037844243857, 1.000000000000000000, 0.8660254037844387076, 1.000000000000000000, 0.8660254037844469233, 0.9999999999999917843 ) ) 
 REPRESENTATION_ITEM ( '' )  );
#4012 = AXIS2_PLACEMENT_3D ( 'NONE', #34312, #2285, #36776 ) ;
#4013 = CARTESIAN_POINT ( 'NONE',  ( -5.233372021372430183, 124.5476862821014663, -8.152565276336710909 ) ) ;
#4014 = CARTESIAN_POINT ( 'NONE',  ( 15.00000000000000178, 246.4937500012290172, 3.464101615137757051 ) ) ;
#4015 = CARTESIAN_POINT ( 'NONE',  ( -4.944772684328673229, 29.38518628210144712, 11.48171059495397728 ) ) ;
#4016 = CARTESIAN_POINT ( 'NONE',  ( 19.56230152254411792, -5.196152422706635576, -6.150000000000044764 ) ) ;
#4017 = UNCERTAINTY_MEASURE_WITH_UNIT (LENGTH_MEASURE( 1.000000000000000082E-05 ), #8757, 'distance_accuracy_value', 'NONE');
#4018 = ORIENTED_EDGE ( 'NONE', *, *, #22396, .T. ) ;
#4019 = CARTESIAN_POINT ( 'NONE',  ( -33.77455436395489841, 205.1570982666397640, 4.673758765035199048 ) ) ;
#4020 = CARTESIAN_POINT ( 'NONE',  ( 15.53471296425195369, 127.4226862821014521, -2.908627838312120684 ) ) ;
#4021 = CYLINDRICAL_SURFACE ( 'NONE', #15775, 5.999999999999999112 ) ;
#4022 = CARTESIAN_POINT ( 'NONE',  ( 8.152565276336593669, 140.7523137178985166, 5.233372021372610483 ) ) ;
#4023 = CARTESIAN_POINT ( 'NONE',  ( -13.62178482187498396, 198.9781250006145399, 23.59362340125808188 ) ) ;
#4024 = CYLINDRICAL_SURFACE ( 'NONE', #12318, 27.00000000000000355 ) ;
#4025 = CARTESIAN_POINT ( 'NONE',  ( -13.49999999999998401, 196.4750000000000227, 23.38268590217985476 ) ) ;
#4026 = CARTESIAN_POINT ( 'NONE',  ( 10.49999999999999645, 252.0000000000000000, 5.000000000000000000 ) ) ;
#4027 = EDGE_CURVE ( 'NONE', #32139, #23609, #17530, .T. ) ;
#4028 = DIRECTION ( 'NONE',  ( 0.08715574274765150453, 0.000000000000000000, 0.9961946980917461003 ) ) ;
#4029 = CARTESIAN_POINT ( 'NONE',  ( 8.710071997420211432, 84.11481371789855643, -3.796722387233181895 ) ) ;
#4030 = VERTEX_POINT ( 'NONE', #24216 ) ;
#4031 = CARTESIAN_POINT ( 'NONE',  ( 21.00000000000000000, 244.5437500012290286, -6.928203230275506996 ) ) ;
#4032 = CARTESIAN_POINT ( 'NONE',  ( -8.715434833792127023, 78.93981371789855928, 8.962234695871568846 ) ) ;
#4033 = CARTESIAN_POINT ( 'NONE',  ( 19.68408634441910721, 5.407089921784862696, -4.396874999385541827 ) ) ;
#4034 = CARTESIAN_POINT ( 'NONE',  ( -27.24356964375000345, 199.8031250006145285, 0.000000000000000000 ) ) ;
#4035 = CARTESIAN_POINT ( 'NONE',  ( 21.00000000000000000, -6.646953231504538984, -5.090624999385466865 ) ) ;
#4036 = CARTESIAN_POINT ( 'NONE',  ( -11.61527771782809282, 53.06481371789854506, -4.622313124798832717 ) ) ;
#4037 = EDGE_CURVE ( 'NONE', #22329, #4445, #17973, .T. ) ;
#4038 = EDGE_LOOP ( 'NONE', ( #19316, #13265 ) ) ;
#4039 = CARTESIAN_POINT ( 'NONE',  ( 18.12178482187500350, -4.985214923628407568, -7.715624999385467753 ) ) ;
#4040 = CARTESIAN_POINT ( 'NONE',  ( 15.24356964375000167, 244.8343750006145285, 3.323476615752272600 ) ) ;
#4041 = AXIS2_PLACEMENT_3D ( 'NONE', #30951, #17105, #10662 ) ;
#4042 = CARTESIAN_POINT ( 'NONE',  ( 4.944772684328679446, 15.58518628210145351, -11.48171059495397373 ) ) ;
#4043 = CARTESIAN_POINT ( 'NONE',  ( -40.69419563604516554, 203.5000000000000000, 0.1155267958017914542 ) ) ;
#4044 = CARTESIAN_POINT ( 'NONE',  ( -58.70461230271182984, 208.1428034533959135, -6.469044688360754414 ) ) ;
#4045 = FILL_AREA_STYLE ('',( #824 ) ) ;
#4046 = CARTESIAN_POINT ( 'NONE',  ( 36.63838227223477872, -3.464101615137751278, 159.9052478282085303 ) ) ;
#4047 = CARTESIAN_POINT ( 'NONE',  ( 4.622313124798831829, 92.16481371789855359, -11.61527771782809282 ) ) ;
#4048 = CARTESIAN_POINT ( 'NONE',  ( -42.87872103062157692, 205.4690446883607535, 1.090244570138264368 ) ) ;
#4049 = CARTESIAN_POINT ( 'NONE',  ( -66.82663769728823411, 204.3130714775002730, 3.149950860017883603 ) ) ;
#4050 = CARTESIAN_POINT ( 'NONE',  ( 26.75643035624999655, 3.323476615752271268, -5.840624999385470417 ) ) ;
#4051 = CYLINDRICAL_SURFACE ( 'NONE', #16179, 5.999999999999999112 ) ;
#4052 = CARTESIAN_POINT ( 'NONE',  ( -13.04141134922778456, 51.62731371789855928, 8.927990412390377273 ) ) ;
#4053 = CARTESIAN_POINT ( 'NONE',  ( -51.77752896937850124, 214.3500491399821897, 7.303452534266821949 ) ) ;
#4054 = VECTOR ( 'NONE', #6445, 999.9999999999998863 ) ;
#4055 = ADVANCED_FACE ( 'NONE', ( #9806 ), #27055, .F. ) ;
#4056 = CARTESIAN_POINT ( 'NONE',  ( -7.234628195640289583, 198.1075961894323143, -27.00000000000001421 ) ) ;
#4057 = CARTESIAN_POINT ( 'NONE',  ( 6.932735513423970097, 83.14768628210144641, 10.69584247140445044 ) ) ;
#4058 = CARTESIAN_POINT ( 'NONE',  ( -13.23911966647218463, 30.24768628210144783, 8.632099005475506459 ) ) ;
#4059 = DIRECTION ( 'NONE',  ( 0.000000000000000000, 0.000000000000000000, 1.000000000000000000 ) ) ;
#4060 = CARTESIAN_POINT ( 'NONE',  ( 38.16802127826974100, 7.686353184319911769, 158.6159210646234783 ) ) ;
#4061 = ORIENTED_EDGE ( 'NONE', *, *, #8048, .T. ) ;
#4062 = CARTESIAN_POINT ( 'NONE',  ( -2.908627838312119351, 51.52268628210144641, -15.53471296425195369 ) ) ;
#4063 = VECTOR ( 'NONE', #21364, 1000.000000000000000 ) ;
#4064 = CARTESIAN_POINT ( 'NONE',  ( -27.24356964375000345, 198.0031250006145456, 0.000000000000000000 ) ) ;
#4065 = EDGE_CURVE ( 'NONE', #20125, #23018, #707, .T. ) ;
#4066 = LINE ( 'NONE', #10130, #20503 ) ;
#4067 = FACE_OUTER_BOUND ( 'NONE', #24122, .T. ) ;
#4068 = CARTESIAN_POINT ( 'NONE',  ( -42.48288769728824121, 203.5309553116391612, -1.857196546604028775 ) ) ;
#4069 = CARTESIAN_POINT ( 'NONE',  ( 23.34314575050770202, 3.999999999999897859, 49.79500130984166617 ) ) ;
#4070 = CARTESIAN_POINT ( 'NONE',  ( 2.311890736173175753, 28.52268628210144641, 12.53471296425194836 ) ) ;
#4071 = CARTESIAN_POINT ( 'NONE',  ( 15.24356964374999990, 249.8593750006145342, 0.000000000000000000 ) ) ;
#4072 = CARTESIAN_POINT ( 'NONE',  ( 0.1745138560723095977, 132.9898137178985564, 9.500000000000005329 ) ) ;
#4073 = CARTESIAN_POINT ( 'NONE',  ( 20.99999999999999645, 244.5718750006145399, 6.646953231504538984 ) ) ;
#4074 = ORIENTED_EDGE ( 'NONE', *, *, #23631, .F. ) ;
#4075 = CARTESIAN_POINT ( 'NONE',  ( 15.00000000000000000, 0.000000000000000000, -7.649999999999989697 ) ) ;
#4076 = DIRECTION ( 'NONE',  ( -1.558072081575740353E-16, -1.134704379232807653E-16, -1.000000000000000000 ) ) ;
#4077 = EDGE_CURVE ( 'NONE', #26234, #30347, #12463, .T. ) ;
#4078 = CARTESIAN_POINT ( 'NONE',  ( 12.50000000000000355, 130.6898137178985735, -0.1745138560722771515 ) ) ;
#4079 = CARTESIAN_POINT ( 'NONE',  ( 13.44051670066911264, 5.407089921784856479, -6.065624999385538452 ) ) ;
#4080 = CARTESIAN_POINT ( 'NONE',  ( 27.95086320365434318, -5.407089921784859143, 165.2671938279954702 ) ) ;
#4081 = CARTESIAN_POINT ( 'NONE',  ( 22.56230152254410370, 7.347880794884117764E-16, -2.362499998771028231 ) ) ;
#4082 = CARTESIAN_POINT ( 'NONE',  ( -7.794113622367441430, 220.1661624776399719, 2.888482486952295591 ) ) ;
#4083 = ORIENTED_EDGE ( 'NONE', *, *, #20736, .T. ) ;
#4084 = CARTESIAN_POINT ( 'NONE',  ( -8.715434833791929847, 50.66018628210144925, -8.962234695871762469 ) ) ;
#4085 = ORIENTED_EDGE ( 'NONE', *, *, #18977, .F. ) ;
#4086 = ORIENTED_EDGE ( 'NONE', *, *, #8477, .T. ) ;
#4087 = CARTESIAN_POINT ( 'NONE',  ( 27.00000000000001421, 196.7000000012290286, 15.58845726811988897 ) ) ;
#4088 = PLANE ( 'NONE',  #11659 ) ;
#4089 = CARTESIAN_POINT ( 'NONE',  ( 18.00000000000000355, -5.196152422706632912, -1.274999999999998357 ) ) ;
#4090 = CARTESIAN_POINT ( 'NONE',  ( -7.234628195640302017, 198.4049038117967143, 27.00000000000000711 ) ) ;
#4091 = CARTESIAN_POINT ( 'NONE',  ( 18.12178482187500350, -4.985214923628407568, -9.065624999385457627 ) ) ;
#4092 = CARTESIAN_POINT ( 'NONE',  ( -8.962234695871760692, 75.96018628210144641, 8.715434833791933400 ) ) ;
#4093 = CARTESIAN_POINT ( 'NONE',  ( -13.04141134922778456, 14.82731371789855324, 8.927990412390377273 ) ) ;
#4094 = CARTESIAN_POINT ( 'NONE',  ( 10.56230152254427601, -3.464101615137852974, -5.812500000000041744 ) ) ;
#4095 = ADVANCED_FACE ( 'NONE', ( #18348 ), #27242, .F. ) ;
#4096 = CARTESIAN_POINT ( 'NONE',  ( 12.98158921324744774, 213.0069040450338491, 5.206989594055764670 ) ) ;
#4097 = CARTESIAN_POINT ( 'NONE',  ( -51.18377896937850835, 208.9097554298617183, 4.530955311639234040 ) ) ;
#4098 = DIRECTION ( 'NONE',  ( 0.08715574274765150453, 0.000000000000000000, 0.9961946980917461003 ) ) ;
#4099 = CARTESIAN_POINT ( 'NONE',  ( 28.31649303895732928, 5.196152422706630247, 168.0490378450901687 ) ) ;
#4100 = CARTESIAN_POINT ( 'NONE',  ( 9.465287035748106703, 10.80231371789855466, -2.064181346179063237 ) ) ;
#4101 = CARTESIAN_POINT ( 'NONE',  ( -42.87872103062156981, 203.4690446883607535, 1.626142955000567936 ) ) ;
#4102 = CARTESIAN_POINT ( 'NONE',  ( -64.45163769728823411, 217.4189793300686233, -4.149950860017907139 ) ) ;
#4103 = CARTESIAN_POINT ( 'NONE',  ( 15.00000000000000178, 241.0374999999999943, 3.464101615137757051 ) ) ;
#4104 = CARTESIAN_POINT ( 'NONE',  ( 27.24356964375000700, 197.7406250006145285, 15.72908226750537075 ) ) ;
#4105 = AXIS2_PLACEMENT_3D ( 'NONE', #32264, #25832, #37379 ) ;
#4106 = CARTESIAN_POINT ( 'NONE',  ( -13.23911966647199812, 117.7523137178985735, -8.632099005475788900 ) ) ;
#4107 = CARTESIAN_POINT ( 'NONE',  ( -44.45461230271182274, 208.1428034533959135, -6.469044688360754414 ) ) ;
#4108 = EDGE_CURVE ( 'NONE', #37310, #22812, #29896, .T. ) ;
#4109 = EDGE_LOOP ( 'NONE', ( #17978, #4758, #11450, #28178 ) ) ;
#4110 = CARTESIAN_POINT ( 'NONE',  ( -2.660918448318275509, 29.09768628210144925, 12.46528703574805874 ) ) ;
#4111 = CARTESIAN_POINT ( 'NONE',  ( 10.49999999999999822, 222.9518338469886203, -2.500000000000000000 ) ) ;
#4112 = FACE_BOUND ( 'NONE', #26718, .T. ) ;
#4113 = CARTESIAN_POINT ( 'NONE',  ( 31.25523494279520165, -7.209453229046482114, 167.2178717732638233 ) ) ;
#4114 = CARTESIAN_POINT ( 'NONE',  ( -2.908627838312119351, 106.7226862821014635, -15.53471296425195369 ) ) ;
#4115 = CARTESIAN_POINT ( 'NONE',  ( -54.95163769728823411, 215.6869285224996986, -3.149950860017881382 ) ) ;
#4116 = CARTESIAN_POINT ( 'NONE',  ( 22.80587116629411781, -3.604726614523235284, -3.553124999385526728 ) ) ;
#4117 = CARTESIAN_POINT ( 'NONE',  ( -5.529263428287477744, 38.87268628210144072, 7.954856959092191815 ) ) ;
#4118 = DIRECTION ( 'NONE',  ( 0.000000000000000000, 0.000000000000000000, -1.000000000000000000 ) ) ;
#4119 = CARTESIAN_POINT ( 'NONE',  ( -33.18080436395489841, 201.5000000000000000, -0.1155267958017054536 ) ) ;
#4120 = DIRECTION ( 'NONE',  ( 1.000000000000000000, 0.000000000000000000, 0.000000000000000000 ) ) ;
#4121 = CARTESIAN_POINT ( 'NONE',  ( 12.46528703574805874, 72.79768628210146630, 2.660918448318279950 ) ) ;
#4122 = FACE_OUTER_BOUND ( 'NONE', #31746, .T. ) ;
#4123 = CARTESIAN_POINT ( 'NONE',  ( 22.56230152254469346, -3.464101615137414214, -7.799999998771006027 ) ) ;
#4125 = ORIENTED_EDGE ( 'NONE', *, *, #17246, .T. ) ;
#4124 = CARTESIAN_POINT ( 'NONE',  ( -5.233372021372430183, 50.94768628210145067, -8.152565276336710909 ) ) ;
#4126 = CARTESIAN_POINT ( 'NONE',  ( 18.00000000000000355, -5.196152422706632912, -6.168749998770955756 ) ) ;
#4128 = ADVANCED_FACE ( 'NONE', ( #24950 ), #21942, .F. ) ;
#4127 = EDGE_LOOP ( 'NONE', ( #7309, #1381, #30410, #24410 ) ) ;
#4129 = CARTESIAN_POINT ( 'NONE',  ( 24.00000000000000000, -5.196152422706629359, -0.7500000000000006661 ) ) ;
#4130 = CARTESIAN_POINT ( 'NONE',  ( 37.18419511108445619, 3.464101615137973766, 166.1439171237837513 ) ) ;
#4131 = CARTESIAN_POINT ( 'NONE',  ( 37.13513852234969193, 3.604726614523243278, 162.7885495010082764 ) ) ;
#4132 = CARTESIAN_POINT ( 'NONE',  ( 27.83604700695378398, 5.196152422706636465, 162.5575145706350781 ) ) ;
#4133 = CARTESIAN_POINT ( 'NONE',  ( 21.00000000000000000, 246.7375000000000114, -6.928203230275506996 ) ) ;
#4134 = CARTESIAN_POINT ( 'NONE',  ( 27.24356964375000700, 195.4906250006145001, 15.72908226750537075 ) ) ;
#4135 = CARTESIAN_POINT ( 'NONE',  ( -10.69584247140429412, 99.35231371789855359, -6.932735513424201024 ) ) ;
#4136 = CARTESIAN_POINT ( 'NONE',  ( 11.48171059495397728, 109.8851862821014436, 4.944772684328674117 ) ) ;
#4137 = ORIENTED_EDGE ( 'NONE', *, *, #29096, .F. ) ;
#4138 = ORIENTED_EDGE ( 'NONE', *, *, #3543, .T. ) ;
#4139 = CARTESIAN_POINT ( 'NONE',  ( 5.778771075727756162E-15, 196.7656250006145342, 31.45816453501075927 ) ) ;
#4140 = CARTESIAN_POINT ( 'NONE',  ( 21.00000000000000000, 240.1843750006145513, -6.646953231504538984 ) ) ;
#4141 = CARTESIAN_POINT ( 'NONE',  ( 14.38691631536194393, 76.06481371789855928, 5.770363421894124656 ) ) ;
#4142 = CARTESIAN_POINT ( 'NONE',  ( 18.12178482187500350, -4.985214923628407568, -6.928124999385470772 ) ) ;
#4143 = CARTESIAN_POINT ( 'NONE',  ( 26.75643035624999655, 244.7218750006145456, -3.323476615752271712 ) ) ;
#4144 = CARTESIAN_POINT ( 'NONE',  ( -5.529263428287477744, 94.07268628210144357, 7.954856959092191815 ) ) ;
#4145 = CARTESIAN_POINT ( 'NONE',  ( 5.727106289114498080E-15, 195.2750000012290172, 31.17691453623979214 ) ) ;
#4146 = CARTESIAN_POINT ( 'NONE',  ( -9.500000000000005329, 52.48981371789855643, 0.1745138560723101806 ) ) ;
#4147 = EDGE_CURVE ( 'NONE', #30190, #23622, #27268, .T. ) ;
#4148 = CARTESIAN_POINT ( 'NONE',  ( 16.56230152254411081, -7.209453229046475009, -8.128124999385510918 ) ) ;
#4149 = CIRCLE ( 'NONE', #8989, 5.000000000000000888 ) ;
#4150 = CARTESIAN_POINT ( 'NONE',  ( 8.710071997420211432, 111.7148137178985792, -3.796722387233181895 ) ) ;
#4151 = CARTESIAN_POINT ( 'NONE',  ( 26.75643035624999655, 240.1093750006145342, -3.323476615752271268 ) ) ;
#4152 = CARTESIAN_POINT ( 'NONE',  ( 12.53471296425189330, 29.77731371789854720, 2.311890736173451977 ) ) ;
#4153 = CARTESIAN_POINT ( 'NONE',  ( -6.932735513423968321, 87.74768628210145494, -10.69584247140445221 ) ) ;
#4154 = CARTESIAN_POINT ( 'NONE',  ( 13.56230152254410370, 5.196152422706630247, -4.912499998770996967 ) ) ;
#4155 = EDGE_CURVE ( 'NONE', #28841, #4918, #31359, .T. ) ;
#4156 = CARTESIAN_POINT ( 'NONE',  ( -47.00000000000000711, 244.5000000000000000, -2.499999999999997780 ) ) ;
#4157 = CARTESIAN_POINT ( 'NONE',  ( 24.68080903822037087, -3.604726614523240613, 163.7087675451007271 ) ) ;
#4158 = CARTESIAN_POINT ( 'NONE',  ( 13.44051670066911086, 5.407089921784862696, -3.871874999385516158 ) ) ;
#4159 = DIRECTION ( 'NONE',  ( -2.057406622567553763E-16, 0.000000000000000000, 1.000000000000000000 ) ) ;
#4160 = DIRECTION ( 'NONE',  ( -0.000000000000000000, -0.000000000000000000, 1.000000000000000000 ) ) ;
#4161 = CARTESIAN_POINT ( 'NONE',  ( 18.00000000000000000, 244.0749999999999886, -5.196152422706630247 ) ) ;
#4162 = CARTESIAN_POINT ( 'NONE',  ( 9.465287035748067623, 91.19768628210145778, 2.064181346179272847 ) ) ;
#4163 = DIRECTION ( 'NONE',  ( -0.000000000000000000, 1.000000000000000000, -0.000000000000000000 ) ) ;
#4164 = CARTESIAN_POINT ( 'NONE',  ( 6.932735513423970097, 138.3476862821014493, 10.69584247140445044 ) ) ;
#4165 = CARTESIAN_POINT ( 'NONE',  ( 25.01079625726091749, 203.5081962293401148, -5.000000000000000000 ) ) ;
#4166 = CARTESIAN_POINT ( 'NONE',  ( 21.00000000000000000, 240.6343750006145115, -6.646953231504538984 ) ) ;
#4167 = ORIENTED_EDGE ( 'NONE', *, *, #17535, .T. ) ;
#4168 = CARTESIAN_POINT ( 'NONE',  ( 34.25565102910361759, -5.407089921784855591, 165.6943207089371981 ) ) ;
#4169 = CARTESIAN_POINT ( 'NONE',  ( 26.75643035624999655, -3.323476615752267715, -3.553124999385494753 ) ) ;
#4170 = CARTESIAN_POINT ( 'NONE',  ( 23.99999999999999645, 242.6500000000000057, -5.196152422706631135 ) ) ;
#4171 = CARTESIAN_POINT ( 'NONE',  ( 36.98482634954957859, 7.347880794884125653E-16, 163.8651217518988688 ) ) ;
#4172 = CARTESIAN_POINT ( 'NONE',  ( 34.38190641693269356, -5.196152422706635576, 168.5347505191977859 ) ) ;
#4173 = DIRECTION ( 'NONE',  ( 0.08715574274765150453, 0.000000000000000000, 0.9961946980917461003 ) ) ;
#4174 = CARTESIAN_POINT ( 'NONE',  ( 18.12178482187499640, 243.9343750006145513, -4.985214923628404904 ) ) ;
#4175 = CARTESIAN_POINT ( 'NONE',  ( -5.233372021372612259, 23.45231371789854435, 8.152565276336593669 ) ) ;
#4176 = CARTESIAN_POINT ( 'NONE',  ( 27.24356964374999279, 196.0718750006145399, -15.72908226750539207 ) ) ;
#4178 = VERTEX_POINT ( 'NONE', #1832 ) ;
#4177 = ORIENTED_EDGE ( 'NONE', *, *, #27306, .T. ) ;
#4179 = CARTESIAN_POINT ( 'NONE',  ( 15.24356964374999990, 247.4593750006145285, -3.323476615752268604 ) ) ;
#4180 = CARTESIAN_POINT ( 'NONE',  ( 6.932735513424201024, 28.05231371789855643, -10.69584247140429412 ) ) ;
#4181 = CARTESIAN_POINT ( 'NONE',  ( 15.24356964374999990, 3.323476615752268604, -1.528124999385498173 ) ) ;
#4182 = CARTESIAN_POINT ( 'NONE',  ( -14.38691631536193860, 135.8648137178985849, -5.770363421894132649 ) ) ;
#4183 =( BOUNDED_CURVE ( )  B_SPLINE_CURVE ( 2, ( #2152, #5183, #10876, #27568, #11062, #1598, #34184, #22265, #33439 ),
 .UNSPECIFIED., .F., .F. ) 
 B_SPLINE_CURVE_WITH_KNOTS ( ( 3, 2, 2, 2, 3 ),
 ( 0.6041666666666667407, 0.6111111111111111605, 0.6250000000000000000, 0.6388888888888888395, 0.6458333333333333703 ),
 .UNSPECIFIED. ) 
 CURVE ( )  GEOMETRIC_REPRESENTATION_ITEM ( )  RATIONAL_B_SPLINE_CURVE ( ( 0.9330127018922192983, 0.9330127018922198534, 1.000000000000000000, 0.8660254037844387076, 1.000000000000000000, 0.8660254037844387076, 1.000000000000000000, 0.9330127018922187432, 0.9330127018922192983 ) ) 
 REPRESENTATION_ITEM ( '' )  );
#4184 = CARTESIAN_POINT ( 'NONE',  ( 23.87821517812499650, 4.985214923628404904, -0.4031249993854957303 ) ) ;
#4185 = ORIENTED_EDGE ( 'NONE', *, *, #35475, .F. ) ;
#4186 = CARTESIAN_POINT ( 'NONE',  ( 10.31873187879410558, 0.000000000000000000, -6.946874999385510563 ) ) ;
#4187 = ORIENTED_EDGE ( 'NONE', *, *, #34152, .F. ) ;
#4188 = CARTESIAN_POINT ( 'NONE',  ( 27.24356964375000345, 195.9781250006145399, -3.336375036156643733E-15 ) ) ;
#4189 = CARTESIAN_POINT ( 'NONE',  ( -6.932735513423968321, 133.7476862821014549, -10.69584247140445221 ) ) ;
#4190 = CARTESIAN_POINT ( 'NONE',  ( 27.78908035617901717, -5.407089921784865361, 163.4180074196626720 ) ) ;
#4191 = CARTESIAN_POINT ( 'NONE',  ( -56.32961230271183695, 212.3930949314663792, 8.469044688360751749 ) ) ;
#4192 = CARTESIAN_POINT ( 'NONE',  ( 26.75643035624999655, 247.6843750006145513, 3.323476615752267271 ) ) ;
#4193 = CARTESIAN_POINT ( 'NONE',  ( -40.49627896937850835, 205.4690446883607535, -1.090244570138286351 ) ) ;
#4194 = CARTESIAN_POINT ( 'NONE',  ( -11.61527771782819940, 131.7351862821014663, 4.622313124798574258 ) ) ;
#4195 = CARTESIAN_POINT ( 'NONE',  ( 37.37536153829788077, 3.604726614523238837, 165.5343111376236607 ) ) ;
#4196 = VERTEX_POINT ( 'NONE', #4671 ) ;
#4197 =( BOUNDED_CURVE ( )  B_SPLINE_CURVE ( 2, ( #248, #11812, #18082, #26779, #26588, #20172, #32464, #12187, #23759 ),
 .UNSPECIFIED., .F., .F. ) 
 B_SPLINE_CURVE_WITH_KNOTS ( ( 3, 2, 2, 2, 3 ),
 ( 0.2934782608695652439, 0.2971014492753623060, 0.3043478260869565410, 0.3115942028985507206, 0.3152173913043477826 ),
 .UNSPECIFIED. ) 
 CURVE ( )  GEOMETRIC_REPRESENTATION_ITEM ( )  RATIONAL_B_SPLINE_CURVE ( ( 0.9330127018922194093, 0.9330127018922198534, 1.000000000000000000, 0.8660254037844387076, 1.000000000000000000, 0.8660254037844387076, 1.000000000000000000, 0.9330127018922198534, 0.9330127018922191873 ) ) 
 REPRESENTATION_ITEM ( '' )  );
#4198 = CARTESIAN_POINT ( 'NONE',  ( 20.99999999999999645, -6.928203230275506996, -5.287499999999990763 ) ) ;
#4199 = CARTESIAN_POINT ( 'NONE',  ( -5.770363421893818234, 134.0351862821014493, -14.38691631536207005 ) ) ;
#4200 = CARTESIAN_POINT ( 'NONE',  ( -52.57663769728824832, 202.5810206699313767, 4.149950860017909804 ) ) ;
#4201 = CARTESIAN_POINT ( 'NONE',  ( 3.474262827703335166, 111.0351862821014635, 8.843639120294326972 ) ) ;
#4202 = CARTESIAN_POINT ( 'NONE',  ( 15.00000000000000000, 241.4124999999999659, -3.464101615137752610 ) ) ;
#4203 = CARTESIAN_POINT ( 'NONE',  ( 10.69584247140445221, 25.64768628210143930, -6.932735513423970097 ) ) ;
#4204 = CARTESIAN_POINT ( 'NONE',  ( 22.56230152254412147, -3.464101615137755275, -7.912500000000034284 ) ) ;
#4205 = EDGE_LOOP ( 'NONE', ( #21903, #16404, #32468, #17665, #13665 ) ) ;
#4206 = FACE_OUTER_BOUND ( 'NONE', #5940, .T. ) ;
#4207 = CARTESIAN_POINT ( 'NONE',  ( -15.50000000000000533, 113.9101862821014493, -0.1745138560725808530 ) ) ;
#4208 = CARTESIAN_POINT ( 'NONE',  ( 20.99999999999997513, 246.7937500012290286, -5.999999999999999112 ) ) ;
#4209 = CARTESIAN_POINT ( 'NONE',  ( 8.843639120294328748, 7.535186282101451916, -3.474262827703334722 ) ) ;
#4210 = CARTESIAN_POINT ( 'NONE',  ( 27.24356964374999635, 198.7156250006145513, -15.72908226750539029 ) ) ;
#4211 = CARTESIAN_POINT ( 'NONE',  ( -27.00000000000000355, 200.0000000000000000, 0.000000000000000000 ) ) ;
#4212 = CARTESIAN_POINT ( 'NONE',  ( 27.00000000000000355, 195.7250000000000227, -3.306546357697854128E-15 ) ) ;
#4213 = CARTESIAN_POINT ( 'NONE',  ( 19.56230152254410370, 5.196152422706631135, -1.387499998770996834 ) ) ;
#4214 = DIRECTION ( 'NONE',  ( 0.000000000000000000, 0.000000000000000000, 1.000000000000000000 ) ) ;
#4215 = CARTESIAN_POINT ( 'NONE',  ( -1.715153634034442431, 68.87731371789855928, 9.534712964251900402 ) ) ;
#4216 = EDGE_LOOP ( 'NONE', ( #33261, #19684 ) ) ;
#4217 = CARTESIAN_POINT ( 'NONE',  ( 24.00000000000000000, 244.8062500012290457, 5.196152422706629359 ) ) ;
#4218 = CARTESIAN_POINT ( 'NONE',  ( -8.962234695871565293, 81.23981371789855643, -8.715434833792128799 ) ) ;
#4219 = CARTESIAN_POINT ( 'NONE',  ( 10.31873187879410914, 0.000000000000000000, -4.696874999385508787 ) ) ;
#4220 = CARTESIAN_POINT ( 'NONE',  ( -6.443006283225887643, 143.0000000000001421, 10.75771091796995726 ) ) ;
#4221 = CARTESIAN_POINT ( 'NONE',  ( 18.12178482187499640, 4.985214923628404904, -3.478124999385490135 ) ) ;
#4222 = CARTESIAN_POINT ( 'NONE',  ( 10.49813415416005213, 47.02731371789855075, -7.228626920338837358 ) ) ;
#4223 =( REPRESENTATION_RELATIONSHIP ('NONE','NONE', #4304, #36285 ) REPRESENTATION_RELATIONSHIP_WITH_TRANSFORMATION ( #12820 )SHAPE_REPRESENTATION_RELATIONSHIP( ) );
#4224 = ORIENTED_EDGE ( 'NONE', *, *, #14456, .F. ) ;
#4225 = DIRECTION ( 'NONE',  ( 0.000000000000000000, 0.000000000000000000, -1.000000000000000000 ) ) ;
#4226 = CARTESIAN_POINT ( 'NONE',  ( 23.87821517812500005, 244.4968750006145228, 4.985214923628404016 ) ) ;
#4227 = CARTESIAN_POINT ( 'NONE',  ( 8.715434833791931624, 18.46018628210144286, 8.962234695871760692 ) ) ;
#4228 = CARTESIAN_POINT ( 'NONE',  ( -38.51711230271183695, 216.4690446883607535, -1.857196546604089393 ) ) ;
#4229 = CIRCLE ( 'NONE', #23608, 2.649999999999999467 ) ;
#4230 = CARTESIAN_POINT ( 'NONE',  ( -53.16294563604517265, 214.6737587650350747, -4.842901733360249317 ) ) ;
#4231 =( BOUNDED_CURVE ( )  B_SPLINE_CURVE ( 2, ( #32123, #5784, #34231, #14145, #25882, #5409, #2941 ),
 .UNSPECIFIED., .F., .F. ) 
 B_SPLINE_CURVE_WITH_KNOTS ( ( 3, 2, 2, 3 ),
 ( 0.3913043478260868069, 0.3985507246376810975, 0.4057971014492754436, 0.4130434782608697342 ),
 .UNSPECIFIED. ) 
 CURVE ( )  GEOMETRIC_REPRESENTATION_ITEM ( )  RATIONAL_B_SPLINE_CURVE ( ( 1.000000000000003109, 0.8660254037844357100, 1.000000000000000000, 0.8660254037844387076, 1.000000000000000000, 0.8660254037844355990, 1.000000000000003109 ) ) 
 REPRESENTATION_ITEM ( '' )  );
#4232 = LINE ( 'NONE', #9554, #3049 ) ;
#4233 = CARTESIAN_POINT ( 'NONE',  ( 6.932735513424201024, 92.45231371789856212, -10.69584247140429412 ) ) ;
#4234 = CARTESIAN_POINT ( 'NONE',  ( -41.49330436395490551, 210.1155267958017703, -4.499999999999996447 ) ) ;
#4235 = CARTESIAN_POINT ( 'NONE',  ( -51.38913769728823411, 206.8500491399821044, -5.686928522499717253 ) ) ;
#4236 = DIRECTION ( 'NONE',  ( 1.000000000000000000, 0.000000000000000000, 0.000000000000000000 ) ) ;
#4237 = DIRECTION ( 'NONE',  ( 0.9961946980917462113, 0.000000000000000000, -0.08715574274765118534 ) ) ;
#4238 = CARTESIAN_POINT ( 'NONE',  ( 14.38691631536194393, 66.86481371789854222, 5.770363421894124656 ) ) ;
#4239 = CARTESIAN_POINT ( 'NONE',  ( -51.57961230271184405, 212.3930949314663792, 8.469044688360751749 ) ) ;
#4240 = AXIS2_PLACEMENT_3D ( 'NONE', #34513, #2486, #34694 ) ;
#4241 = DIRECTION ( 'NONE',  ( 0.000000000000000000, 0.000000000000000000, 1.000000000000000000 ) ) ;
#4242 = CARTESIAN_POINT ( 'NONE',  ( -8.715434833791929847, 78.26018628210144357, -8.962234695871762469 ) ) ;
#4243 = CARTESIAN_POINT ( 'NONE',  ( 8.632099005475504683, 18.74768628210143362, 13.23911966647218996 ) ) ;
#4244 = CARTESIAN_POINT ( 'NONE',  ( 10.56230152254411614, -3.464101615137761048, -0.4125000000000307865 ) ) ;
#4245 = CARTESIAN_POINT ( 'NONE',  ( -28.37024444651914123, 204.7169729760873906, -6.013169554073232170 ) ) ;
#4246 = B_SPLINE_CURVE_WITH_KNOTS ( 'NONE', 1,
 ( #28767, #23658 ),
 .UNSPECIFIED., .F., .F.,
 ( 2, 2 ),
 ( 0.000000000000000000, 1.000000000000000000 ),
 .UNSPECIFIED. ) ;
#4247 = VERTEX_POINT ( 'NONE', #16254 ) ;
#4248 = CARTESIAN_POINT ( 'NONE',  ( -15.53471296425195369, 40.02268628210144641, 2.908627838312118019 ) ) ;
#4249 = CARTESIAN_POINT ( 'NONE',  ( -27.24356964375000345, 197.1031250006145399, 0.000000000000000000 ) ) ;
#4250 = CARTESIAN_POINT ( 'NONE',  ( 22.56230152254400423, -3.464101615137808565, -0.5999999987710193938 ) ) ;
#4251 = CARTESIAN_POINT ( 'NONE',  ( 36.82467767225140420, -3.464101615137388013, 162.0346139941552508 ) ) ;
#4252 = CARTESIAN_POINT ( 'NONE',  ( -36.74330436395489841, 210.1155267958017134, -6.500000000000000888 ) ) ;
#4253 = CARTESIAN_POINT ( 'NONE',  ( -1.045839947578415010E-13, 195.1625000000000512, 27.00000000000000355 ) ) ;
#4254 = CARTESIAN_POINT ( 'NONE',  ( -7.228626920339069173, 20.47268628210144570, 10.49813415415989581 ) ) ;
#4255 = CARTESIAN_POINT ( 'NONE',  ( 21.00000000000000000, 249.0718750006145399, 6.646953231504538984 ) ) ;
#4256 = CARTESIAN_POINT ( 'NONE',  ( 6.840914352311949109, 131.8398137178985792, 6.594114490232462877 ) ) ;
#4257 = CARTESIAN_POINT ( 'NONE',  ( 23.87821517812500005, 244.1593750006145171, 4.985214923628404016 ) ) ;
#4258 = PRESENTATION_LAYER_ASSIGNMENT (  '', '', ( #30921 ) ) ;
#4259 = ORIENTED_EDGE ( 'NONE', *, *, #9642, .F. ) ;
#4260 = DIRECTION ( 'NONE',  ( -0.000000000000000000, 1.000000000000000000, -0.000000000000000000 ) ) ;
#4261 = CARTESIAN_POINT ( 'NONE',  ( 8.962234695871567070, 131.8398137178985792, 8.715434833792127023 ) ) ;
#4262 = CARTESIAN_POINT ( 'NONE',  ( 10.31873187879410914, 0.000000000000000000, -7.790624999385542537 ) ) ;
#4263 = CARTESIAN_POINT ( 'NONE',  ( 34.21643094486717729, -5.407089921784855591, 165.2460330947959051 ) ) ;
#4264 = CARTESIAN_POINT ( 'NONE',  ( 22.56230152254410370, 0.000000000000000000, -10.00000000000000000 ) ) ;
#4265 = CARTESIAN_POINT ( 'NONE',  ( 27.00000000000000355, 197.5250000000000057, -3.306546357697854128E-15 ) ) ;
#4266 = EDGE_CURVE ( 'NONE', #32003, #30542, #13215, .T. ) ;
#4267 = ORIENTED_EDGE ( 'NONE', *, *, #20101, .F. ) ;
#4268 = CARTESIAN_POINT ( 'NONE',  ( 12.53471296425194659, 26.22268628210144925, -2.311890736173178418 ) ) ;
#4269 = ORIENTED_EDGE ( 'NONE', *, *, #629, .T. ) ;
#4270 = EDGE_LOOP ( 'NONE', ( #13366, #36759, #31537, #32986 ) ) ;
#4271 = LINE ( 'NONE', #21353, #32148 ) ;
#4272 = DIRECTION ( 'NONE',  ( -0.000000000000000000, 1.000000000000000000, -0.000000000000000000 ) ) ;
#4273 = CARTESIAN_POINT ( 'NONE',  ( 22.60769515458673951, 249.2888461906613884, 5.999999999999998224 ) ) ;
#4274 = CARTESIAN_POINT ( 'NONE',  ( 23.99999999999999645, 5.196152422706631135, -6.000000000000005329 ) ) ;
#4275 = CARTESIAN_POINT ( 'NONE',  ( 23.87821517812499650, 4.985214923628404904, -9.740624999385467220 ) ) ;
#4276 = CARTESIAN_POINT ( 'NONE',  ( 2.660918448318279950, 79.69768628210144357, -12.46528703574805697 ) ) ;
#4277 = CARTESIAN_POINT ( 'NONE',  ( -8.927990412390371944, 7.927313717898536005, -13.04141134922778988 ) ) ;
#4278 = CARTESIAN_POINT ( 'NONE',  ( 26.99999999999999645, 243.5687500012290343, -3.464101615137755275 ) ) ;
#4279 = CARTESIAN_POINT ( 'NONE',  ( 15.00000000000000000, 243.7562500012290627, 0.000000000000000000 ) ) ;
#4280 = CARTESIAN_POINT ( 'NONE',  ( -55.34002896937850124, 206.1606490808709111, 2.350049139982143931 ) ) ;
#4281 = DIRECTION ( 'NONE',  ( -0.000000000000000000, -0.000000000000000000, 1.000000000000000000 ) ) ;
#4282 = CARTESIAN_POINT ( 'NONE',  ( 37.11229162342512211, 7.347880794884117764E-16, 165.3220564990824073 ) ) ;
#4283 = CARTESIAN_POINT ( 'NONE',  ( -2.311890736173448424, 142.4773137178985678, 12.53471296425189330 ) ) ;
#4284 = CARTESIAN_POINT ( 'NONE',  ( -48.81622103062156270, 211.6261429550005744, 6.530955311639227823 ) ) ;
#4285 = CARTESIAN_POINT ( 'NONE',  ( -53.56622103062157692, 212.1620413398628671, 8.530955311639223382 ) ) ;
#4286 = CONTEXT_DEPENDENT_SHAPE_REPRESENTATION ( #18530, #20776 ) ;
#4287 = AXIS2_PLACEMENT_3D ( 'NONE', #12544, #3629, #18811 ) ;
#4288 = DIRECTION ( 'NONE',  ( 0.000000000000000000, -1.000000000000000000, 0.000000000000000000 ) ) ;
#4289 = CARTESIAN_POINT ( 'NONE',  ( -13.62178482187500528, 199.7281250006145399, -23.59362340125807123 ) ) ;
#4290 = CARTESIAN_POINT ( 'NONE',  ( 8.632099005475788900, 110.8523137178985252, -13.23911966647199812 ) ) ;
#4291 = CARTESIAN_POINT ( 'NONE',  ( -51.77752896937849414, 213.3500491399821613, 5.571401726697954970 ) ) ;
#4292 = ADVANCED_FACE ( 'NONE', ( #4491 ), #4860, .T. ) ;
#4293 = EDGE_LOOP ( 'NONE', ( #6512, #33594, #114, #10757 ) ) ;
#4294 = DIRECTION ( 'NONE',  ( 0.000000000000000000, -1.000000000000000000, 0.000000000000000000 ) ) ;
#4295 = DIRECTION ( 'NONE',  ( 1.000000000000000000, 0.000000000000000000, 0.000000000000000000 ) ) ;
#4296 = CARTESIAN_POINT ( 'NONE',  ( 24.75107835581066240, 0.000000000000000000, 164.5119495204372413 ) ) ;
#4297 = CARTESIAN_POINT ( 'NONE',  ( 3.257655550457285720, 107.2976862821014521, -15.46528703574804986 ) ) ;
#4298 = CARTESIAN_POINT ( 'NONE',  ( -52.97247103062156981, 206.6499508600178672, 5.571401726697986057 ) ) ;
#4299 = CARTESIAN_POINT ( 'NONE',  ( 13.44051670066911264, -5.407089921784859143, -3.215624999385519267 ) ) ;
#4300 = CARTESIAN_POINT ( 'NONE',  ( 8.710071997420127943, 36.28518628210144215, 3.796722387233375073 ) ) ;
#4301 = DIRECTION ( 'NONE',  ( 1.000000000000000000, 0.000000000000000000, 0.000000000000000000 ) ) ;
#4302 = CARTESIAN_POINT ( 'NONE',  ( -36.94122103062156981, 207.8379586601371329, -8.530955311639223382 ) ) ;
#4303 = CARTESIAN_POINT ( 'NONE',  ( 21.00000000000000355, 0.000000000000000000, 50.00000000000001421 ) ) ;
#4304 = SHAPE_REPRESENTATION ( 'MAS-158', ( #33551, #21446, #31118, #11761, #2663, #23870, #27492, #28692, #12960, #17811, #34757, #16623, #15399, #23272, #13587 ), #1452 ) ;
#4305 = CARTESIAN_POINT ( 'NONE',  ( -0.1745138560725500443, 74.81018628210145494, 12.50000000000000355 ) ) ;
#4306 = CARTESIAN_POINT ( 'NONE',  ( 0.000000000000000000, 200.0000000000000000, 0.000000000000000000 ) ) ;
#4308 = EDGE_LOOP ( 'NONE', ( #16637, #26921, #22360, #2910 ) ) ;
#4307 = CARTESIAN_POINT ( 'NONE',  ( 6.594114490232313663, 46.06018628210144072, 6.840914352312096547 ) ) ;
#4309 = CYLINDRICAL_SURFACE ( 'NONE', #32457, 27.00000000000000000 ) ;
#4310 = ORIENTED_EDGE ( 'NONE', *, *, #8311, .F. ) ;
#4311 = CARTESIAN_POINT ( 'NONE',  ( 15.00000000000000000, 0.000000000000000000, -1.799999999999996048 ) ) ;
#4312 = CARTESIAN_POINT ( 'NONE',  ( -61.68080436395489841, 203.5000000000000000, -0.1155267958017335561 ) ) ;
#4313 = CARTESIAN_POINT ( 'NONE',  ( 24.75107835581066240, 0.000000000000000000, 164.5119495204372413 ) ) ;
#4314 = CARTESIAN_POINT ( 'NONE',  ( 33.79360515338605353, -5.196152422706635576, 161.8104363070785041 ) ) ;
#4315 = CARTESIAN_POINT ( 'NONE',  ( 26.99999999999999645, 246.6625000000000227, -3.464101615137755275 ) ) ;
#4316 = FACE_OUTER_BOUND ( 'NONE', #9865, .T. ) ;
#4317 = CARTESIAN_POINT ( 'NONE',  ( -12.46528703574811558, 79.80231371789857064, 2.660918448318003726 ) ) ;
#4318 = CARTESIAN_POINT ( 'NONE',  ( 2.311890736173175753, 102.1226862821014549, 12.53471296425194659 ) ) ;
#4319 = ORIENTED_EDGE ( 'NONE', *, *, #28696, .F. ) ;
#4320 = AXIS2_PLACEMENT_3D ( 'NONE', #185, #22254, #37331 ) ;
#4321 = ORIENTED_EDGE ( 'NONE', *, *, #23832, .F. ) ;
#4322 = CARTESIAN_POINT ( 'NONE',  ( -27.00000000000000355, 199.1750000012290513, -15.58845726811989429 ) ) ;
#4323 = FACE_OUTER_BOUND ( 'NONE', #36129, .T. ) ;
#4324 = CARTESIAN_POINT ( 'NONE',  ( -15.46528703574811736, 52.20231371789854080, 3.257655550456946436 ) ) ;
#4325 = CARTESIAN_POINT ( 'NONE',  ( 21.00000000000000000, -6.646953231504538984, -6.440624999385486049 ) ) ;
#4326 = CARTESIAN_POINT ( 'NONE',  ( 18.12178482187499640, 245.7343750006145342, -4.985214923628404904 ) ) ;
#4327 = CARTESIAN_POINT ( 'NONE',  ( -50.99330436395489841, 210.1155267958017703, -4.499999999999996447 ) ) ;
#4328 = CARTESIAN_POINT ( 'NONE',  ( 27.00000000000001066, 194.9000000012290457, 15.58845726811988897 ) ) ;
#4329 = CARTESIAN_POINT ( 'NONE',  ( -7.954856959092309943, 51.62731371789855928, 5.529263428287300108 ) ) ;
#4330 = CARTESIAN_POINT ( 'NONE',  ( 19.68408634441910721, 5.407089921784857367, -8.840624999385537919 ) ) ;
#4331 = CARTESIAN_POINT ( 'NONE',  ( 8.710071997420211432, 120.9148137178985678, -3.796722387233181895 ) ) ;
#4332 = CARTESIAN_POINT ( 'NONE',  ( 23.87821517812499650, 240.1468750006145285, -4.985214923628404904 ) ) ;
#4333 = CARTESIAN_POINT ( 'NONE',  ( -8.715434833792127023, 32.93981371789854506, 8.962234695871568846 ) ) ;
#4334 = VECTOR ( 'NONE', #23750, 1000.000000000000000 ) ;
#4335 = CARTESIAN_POINT ( 'NONE',  ( 12.50000000000000355, 90.91018628210146346, 0.1745138560725507937 ) ) ;
#4336 = CARTESIAN_POINT ( 'NONE',  ( 13.56230152254410370, 5.196152422706630247, -8.062499998771011533 ) ) ;
#4337 = DIRECTION ( 'NONE',  ( 0.000000000000000000, 0.000000000000000000, -1.000000000000000000 ) ) ;
#4338 = CARTESIAN_POINT ( 'NONE',  ( 24.83768937516614272, -3.604726614523240613, 165.5019180016658993 ) ) ;
#4339 = CARTESIAN_POINT ( 'NONE',  ( 10.31873187879410914, 0.000000000000000000, -4.696874999385508787 ) ) ;
#4340 = PRESENTATION_STYLE_ASSIGNMENT (( #15920 ) ) ;
#4341 = CARTESIAN_POINT ( 'NONE',  ( 18.00000000000000355, -5.196152422706632912, -3.918749998770953979 ) ) ;
#4342 = CARTESIAN_POINT ( 'NONE',  ( 29.51299565928205482, 6.068759932216711839, 159.5818089612911024 ) ) ;
#4343 = CARTESIAN_POINT ( 'NONE',  ( 8.710071997420127943, 91.48518628210145209, 3.796722387233375073 ) ) ;
#4344 = DIRECTION ( 'NONE',  ( -0.9925324990730152175, 0.1219804832088933616, 0.000000000000000000 ) ) ;
#4345 = EDGE_CURVE ( 'NONE', #35499, #15520, #10408, .T. ) ;
#4346 = CARTESIAN_POINT ( 'NONE',  ( -10.49813415415989581, 133.1726862821014663, -7.228626920339068285 ) ) ;
#4347 = DIRECTION ( 'NONE',  ( 0.000000000000000000, 0.000000000000000000, 1.000000000000000000 ) ) ;
#4348 = CARTESIAN_POINT ( 'NONE',  ( 15.24356964374999990, 249.8593750006145342, 0.000000000000000000 ) ) ;
#4349 = EDGE_LOOP ( 'NONE', ( #10680, #4641, #36463, #13800 ) ) ;
#4350 = CARTESIAN_POINT ( 'NONE',  ( 37.25770128558855987, 3.604726614523238837, 164.1894482951998100 ) ) ;
#4351 = CARTESIAN_POINT ( 'NONE',  ( 26.75643035624999655, -3.323476615752267715, -4.003124999385458516 ) ) ;
#4352 = CARTESIAN_POINT ( 'NONE',  ( 5.778771075727756162E-15, 197.2718750006145569, 31.45816453501076637 ) ) ;
#4353 = CARTESIAN_POINT ( 'NONE',  ( 25.36712902881142284, -3.464101615137761048, 168.7587926862500467 ) ) ;
#4354 = DIRECTION ( 'NONE',  ( 0.000000000000000000, 0.000000000000000000, 1.000000000000000000 ) ) ;
#4355 = CARTESIAN_POINT ( 'NONE',  ( 18.12178482187499640, 243.4843750006145342, -4.985214923628404904 ) ) ;
#4356 = CARTESIAN_POINT ( 'NONE',  ( 10.31873187879410558, 3.604726614523236616, -2.878124999385517135 ) ) ;
#4357 = CARTESIAN_POINT ( 'NONE',  ( -2.311890736173448424, 142.4773137178985678, 12.53471296425189330 ) ) ;
#4358 = CARTESIAN_POINT ( 'NONE',  ( 27.24356964375000700, 197.3468750006145740, 15.72908226750537075 ) ) ;
#4360 = ORIENTED_EDGE ( 'NONE', *, *, #36569, .F. ) ;
#4359 = VERTEX_POINT ( 'NONE', #10923 ) ;
#4361 = AXIS2_PLACEMENT_3D ( 'NONE', #4901, #13445, #30878 ) ;
#4362 = CARTESIAN_POINT ( 'NONE',  ( 18.12178482187499640, 246.5218750006145001, -4.985214923628404904 ) ) ;
#4363 = CARTESIAN_POINT ( 'NONE',  ( -10.49813415416004858, 33.22731371789855359, 7.228626920338840023 ) ) ;
#4364 = EDGE_CURVE ( 'NONE', #22619, #29003, #35223, .T. ) ;
#4365 = CARTESIAN_POINT ( 'NONE',  ( 18.12178482187499640, 4.985214923628404904, -2.915624999385468819 ) ) ;
#4366 = CARTESIAN_POINT ( 'NONE',  ( 3.257655550456945548, 123.5023137178985451, 15.46528703574811736 ) ) ;
#4367 = ADVANCED_FACE ( 'NONE', ( #28170 ), #2200, .F. ) ;
#4368 = CARTESIAN_POINT ( 'NONE',  ( 15.00000000000000000, 0.000000000000000000, -9.843749998770940479 ) ) ;
#4369 = VERTEX_POINT ( 'NONE', #27616 ) ;
#4370 = CARTESIAN_POINT ( 'NONE',  ( 19.68408634441912142, -5.407089921784861808, -6.796874999385527083 ) ) ;
#4371 = ORIENTED_EDGE ( 'NONE', *, *, #15199, .F. ) ;
#4372 = CARTESIAN_POINT ( 'NONE',  ( -13.62178482187498396, 197.1781250006145569, 23.59362340125808188 ) ) ;
#4373 = CARTESIAN_POINT ( 'NONE',  ( 2.311890736173175753, 129.7226862821014777, 12.53471296425194836 ) ) ;
#4374 = CARTESIAN_POINT ( 'NONE',  ( 30.86303410043077022, -7.209453229046482114, 162.7349956318509783 ) ) ;
#4375 = EDGE_CURVE ( 'NONE', #7924, #6128, #11760, .T. ) ;
#4376 = CARTESIAN_POINT ( 'NONE',  ( -56.52752896937850124, 214.3500491399821897, 7.303452534266821949 ) ) ;
#4377 = CARTESIAN_POINT ( 'NONE',  ( 18.12178482187499640, 247.4218750006145342, -4.985214923628404904 ) ) ;
#4378 = SURFACE_STYLE_USAGE ( .BOTH. , #30164 ) ;
#4379 = CARTESIAN_POINT ( 'NONE',  ( -7.234628195640307347, 199.1200961906613713, -27.00000000000000711 ) ) ;
#4380 = CARTESIAN_POINT ( 'NONE',  ( -42.27752896937850835, 212.3500491399821613, 3.839350919129088435 ) ) ;
#4381 = CARTESIAN_POINT ( 'NONE',  ( -4.944772684328673229, 139.7851862821014493, 11.48171059495397728 ) ) ;
#4382 = CARTESIAN_POINT ( 'NONE',  ( 10.56230152254411614, -3.464101615137757051, -1.649999998770997678 ) ) ;
#4383 = VERTEX_POINT ( 'NONE', #37250 ) ;
#4384 = CYLINDRICAL_SURFACE ( 'NONE', #12489, 6.000000000000001776 ) ;
#4385 = CARTESIAN_POINT ( 'NONE',  ( -15.53471296425195369, 113.6226862821014549, 2.908627838312118019 ) ) ;
#4386 = CARTESIAN_POINT ( 'NONE',  ( -51.78497103062156981, 202.6965474657331185, -4.350049139982091084 ) ) ;
#4387 = CARTESIAN_POINT ( 'NONE',  ( -6.840914352312096547, 112.7601862821014720, 6.594114490232313663 ) ) ;
#4388 = CARTESIAN_POINT ( 'NONE',  ( 2.311890736173175753, 19.32268628210144712, 12.53471296425194836 ) ) ;
#4389 = CARTESIAN_POINT ( 'NONE',  ( 10.31873187879410914, 0.000000000000000000, -0.5906249993855583469 ) ) ;
#4390 = ORIENTED_EDGE ( 'NONE', *, *, #21678, .T. ) ;
#4391 = CARTESIAN_POINT ( 'NONE',  ( 19.56230152254412502, -5.196152422706635576, -7.950000000000068567 ) ) ;
#4392 = CARTESIAN_POINT ( 'NONE',  ( 3.474262827703335166, 83.43518628210145494, 8.843639120294326972 ) ) ;
#4393 = PLANE ( 'NONE',  #29689 ) ;
#4394 = CARTESIAN_POINT ( 'NONE',  ( -9.465287035748106703, 135.0023137178985166, 2.064181346179061460 ) ) ;
#4395 = CARTESIAN_POINT ( 'NONE',  ( 5.778771075727756162E-15, 197.6656250006145399, 31.45816453501075927 ) ) ;
#4397 = CARTESIAN_POINT ( 'NONE',  ( -44.35000000000001563, 244.5000000000000000, 0.4999999999999995559 ) ) ;
#4396 =( BOUNDED_CURVE ( )  B_SPLINE_CURVE ( 2, ( #21436, #23706, #15363, #754, #21062, #15174, #12130 ),
 .UNSPECIFIED., .F., .F. ) 
 B_SPLINE_CURVE_WITH_KNOTS ( ( 3, 2, 2, 3 ),
 ( 0.4565217391304328132, 0.4637681159420271593, 0.4710144927536215054, 0.4782608695652158515 ),
 .UNSPECIFIED. ) 
 CURVE ( )  GEOMETRIC_REPRESENTATION_ITEM ( )  RATIONAL_B_SPLINE_CURVE ( ( 1.000000000000035749, 0.8660254037844027364, 1.000000000000000000, 0.8660254037844387076, 1.000000000000000000, 0.8660254037844674624, 0.9999999999999712452 ) ) 
 REPRESENTATION_ITEM ( '' )  );
#4398 = CARTESIAN_POINT ( 'NONE',  ( 13.62178482187501416, 197.7593750006145399, 23.59362340125806767 ) ) ;
#4399 = FACE_OUTER_BOUND ( 'NONE', #4127, .T. ) ;
#4400 = DIRECTION ( 'NONE',  ( 0.000000000000000000, 0.000000000000000000, 1.000000000000000000 ) ) ;
#4401 = CARTESIAN_POINT ( 'NONE',  ( 5.233372021372610483, 74.05231371789854222, -8.152565276336593669 ) ) ;
#4402 = ORIENTED_EDGE ( 'NONE', *, *, #2381, .F. ) ;
#4403 = CARTESIAN_POINT ( 'NONE',  ( 18.00000000000000000, 243.6812500012290457, -5.196152422706630247 ) ) ;
#4404 = CARTESIAN_POINT ( 'NONE',  ( -7.228626920338836470, 81.52731371789856496, -10.49813415416005213 ) ) ;
#4405 = CARTESIAN_POINT ( 'NONE',  ( 22.80587116629412137, 7.646167579472024665E-16, -3.121874999385543248 ) ) ;
#4406 = CARTESIAN_POINT ( 'NONE',  ( -13.83312331854208743, 143.0000000000000000, 2.380703716050323049 ) ) ;
#4407 = CARTESIAN_POINT ( 'NONE',  ( 23.87821517812499650, 4.985214923628404904, -5.353124999385477700 ) ) ;
#4408 = CARTESIAN_POINT ( 'NONE',  ( -7.228626920338836470, 44.72731371789855359, -10.49813415416005213 ) ) ;
#4409 = EDGE_CURVE ( 'NONE', #31449, #11542, #36437, .T. ) ;
#4410 = ORIENTED_EDGE ( 'NONE', *, *, #6952, .F. ) ;
#4411 = CARTESIAN_POINT ( 'NONE',  ( 26.60793733450167053, 1.299049382686714882, -8.000000000000000000 ) ) ;
#4412 = CARTESIAN_POINT ( 'NONE',  ( 23.87821517812499650, 244.6468750006145285, -4.985214923628404904 ) ) ;
#4413 = CARTESIAN_POINT ( 'NONE',  ( -8.715434833791929847, 13.86018628210145032, -8.962234695871762469 ) ) ;
#4414 = CIRCLE ( 'NONE', #34663, 2.649999999999999467 ) ;
#4415 = CARTESIAN_POINT ( 'NONE',  ( -38.91294563604516554, 214.6737587650350747, -4.842901733360248429 ) ) ;
#4416 =( BOUNDED_CURVE ( )  B_SPLINE_CURVE ( 2, ( #6515, #14670, #817, #26220, #256, #11821, #23390, #20555, #37156 ),
 .UNSPECIFIED., .F., .F. ) 
 B_SPLINE_CURVE_WITH_KNOTS ( ( 3, 2, 2, 2, 3 ),
 ( 0.8125000000000000000, 0.8194444444444444198, 0.8333333333333333703, 0.8472222222222222099, 0.8541666666666667407 ),
 .UNSPECIFIED. ) 
 CURVE ( )  GEOMETRIC_REPRESENTATION_ITEM ( )  RATIONAL_B_SPLINE_CURVE ( ( 0.9330127018922194093, 0.9330127018922194093, 1.000000000000000000, 0.8660254037844387076, 1.000000000000000000, 0.8660254037844387076, 1.000000000000000000, 0.9330127018922187432, 0.9330127018922192983 ) ) 
 REPRESENTATION_ITEM ( '' )  );
#4417 = CARTESIAN_POINT ( 'NONE',  ( -59.29836230271183695, 204.3130714775002446, -3.149950860017828091 ) ) ;
#4418 = SHAPE_REPRESENTATION_RELATIONSHIP ( 'NONE' , 'NONE' ,  #16167, #5631 ) ;
#4419 = CARTESIAN_POINT ( 'NONE',  ( 24.71019261795811772, -3.464101615137757051, 161.2499751506078667 ) ) ;
#4420 = CARTESIAN_POINT ( 'NONE',  ( 2.311890736173452865, 64.27731371789855075, -12.53471296425189152 ) ) ;
#4421 = CARTESIAN_POINT ( 'NONE',  ( -43.86830436395490551, 209.8844732041982297, 4.499999999999996447 ) ) ;
#4422 = CARTESIAN_POINT ( 'NONE',  ( -63.26413769728824121, 213.1499508600178672, 5.686928522499718142 ) ) ;
#4423 = CARTESIAN_POINT ( 'NONE',  ( -71.06414469631722852, 221.4078028065942476, -7.500000000000000888 ) ) ;
#4424 = CARTESIAN_POINT ( 'NONE',  ( 0.000000000000000000, 210.0000000000000284, -27.00000000000000000 ) ) ;
#4425 = CARTESIAN_POINT ( 'NONE',  ( -15.46528703574811736, 61.40231371789855785, 3.257655550456946436 ) ) ;
#4426 = CARTESIAN_POINT ( 'NONE',  ( -49.40252896937850124, 205.6499508600178103, -7.303452534266820173 ) ) ;
#4427 = COLOUR_RGB ( '',0.8941176470588234615, 0.8941176470588234615, 0.8941176470588234615 ) ;
#4428 = CYLINDRICAL_SURFACE ( 'NONE', #11372, 6.000000000000001776 ) ;
#4429 = CARTESIAN_POINT ( 'NONE',  ( 8.962234695871762469, 71.36018628210145209, -8.715434833791931624 ) ) ;
#4430 = CARTESIAN_POINT ( 'NONE',  ( 10.83675517735155225, 36.86018628210144499, 11.08355503943142573 ) ) ;
#4431 = DIRECTION ( 'NONE',  ( 0.000000000000000000, 1.000000000000000000, 0.000000000000000000 ) ) ;
#4432 = CARTESIAN_POINT ( 'NONE',  ( -28.72461751544321018, 203.0584876166405195, -4.011490837943430421 ) ) ;
#4433 = ORIENTED_EDGE ( 'NONE', *, *, #32992, .F. ) ;
#4434 = CARTESIAN_POINT ( 'NONE',  ( 8.927990412390657937, 34.27268628210144641, -13.04141134922759804 ) ) ;
#4435 = CARTESIAN_POINT ( 'NONE',  ( -27.24356964374999279, 196.6906250006145456, 15.72908226750539384 ) ) ;
#4436 = CARTESIAN_POINT ( 'NONE',  ( -44.35000000000001563, 244.5000000000000000, 5.000000000000000000 ) ) ;
#4437 = CARTESIAN_POINT ( 'NONE',  ( 24.00000000000000000, 247.4500000000000171, 5.196152422706629359 ) ) ;
#4438 = CARTESIAN_POINT ( 'NONE',  ( -39.71205436395490551, 214.6737587650352168, 4.842901733360204908 ) ) ;
#4439 = CARTESIAN_POINT ( 'NONE',  ( 0.000000000000000000, -20.00000000000000000, 4.899999999999999467 ) ) ;
#4440 = CARTESIAN_POINT ( 'NONE',  ( 12.53471296425194836, 17.02268628210144996, -2.311890736173178418 ) ) ;
#4441 = AXIS2_PLACEMENT_3D ( 'NONE', #28119, #30415, #18867 ) ;
#4442 = CARTESIAN_POINT ( 'NONE',  ( 21.00000000000000000, 247.4687500012290400, 5.999999999999998224 ) ) ;
#4443 = CARTESIAN_POINT ( 'NONE',  ( -3.474262827703527901, 133.5648137178985735, 8.843639120294245259 ) ) ;
#4444 = CARTESIAN_POINT ( 'NONE',  ( 18.12178482187500350, 244.0843750006145285, 4.985214923628407568 ) ) ;
#4445 = VERTEX_POINT ( 'NONE', #28905 ) ;
#4446 = DIRECTION ( 'NONE',  ( 0.000000000000000000, 0.000000000000000000, 1.000000000000000000 ) ) ;
#4447 = CARTESIAN_POINT ( 'NONE',  ( 10.69584247140429589, 140.7523137178985735, 6.932735513424201024 ) ) ;
#4448 = CARTESIAN_POINT ( 'NONE',  ( 22.80587116629410360, 7.646167579472015790E-16, -7.565624999385539340 ) ) ;
#4449 = CARTESIAN_POINT ( 'NONE',  ( 37.13350435217316203, -3.604726614523235284, 162.7698708504190677 ) ) ;
#4450 = CARTESIAN_POINT ( 'NONE',  ( 6.500000000000000000, 244.5000000000000000, 1.000000000000000000 ) ) ;
#4451 = CARTESIAN_POINT ( 'NONE',  ( -26.99999999999998934, 198.6875000000000284, 15.58845726811991561 ) ) ;
#4452 = ORIENTED_EDGE ( 'NONE', *, *, #8939, .F. ) ;
#4453 = CARTESIAN_POINT ( 'NONE',  ( -6.932735513423968321, 32.54768628210144499, -10.69584247140445221 ) ) ;
#4454 = ORIENTED_EDGE ( 'NONE', *, *, #35475, .T. ) ;
#4455 = VERTEX_POINT ( 'NONE', #37430 ) ;
#4456 = DIRECTION ( 'NONE',  ( 0.000000000000000000, 0.000000000000000000, -1.000000000000000000 ) ) ;
#4457 = LINE ( 'NONE', #1424, #25577 ) ;
#4458 = CARTESIAN_POINT ( 'NONE',  ( 24.00000000000000000, 249.3062500012290457, 5.196152422706629359 ) ) ;
#4459 =( BOUNDED_CURVE ( )  B_SPLINE_CURVE ( 2, ( #28654, #34716, #22985, #6092, #5528, #26372, #28840 ),
 .UNSPECIFIED., .F., .F. ) 
 B_SPLINE_CURVE_WITH_KNOTS ( ( 3, 2, 2, 3 ),
 ( 0.08695652173913032135, 0.09420289855072443153, 0.1014492753623185417, 0.1086956521739126380 ),
 .UNSPECIFIED. ) 
 CURVE ( )  GEOMETRIC_REPRESENTATION_ITEM ( )  RATIONAL_B_SPLINE_CURVE ( ( 1.000000000000001998, 0.8660254037844367092, 1.000000000000000000, 0.8660254037844387076, 1.000000000000000000, 0.8660254037844461461, 0.9999999999999925615 ) ) 
 REPRESENTATION_ITEM ( '' )  );
#4461 = CARTESIAN_POINT ( 'NONE',  ( 15.00000000000000000, 0.000000000000000000, -4.500000000000003553 ) ) ;
#4460 = PRESENTATION_LAYER_ASSIGNMENT (  '', '', ( #34112 ) ) ;
#4462 = CARTESIAN_POINT ( 'NONE',  ( 26.75643035624999655, -3.323476615752267715, -8.503124999385478944 ) ) ;
#4463 = CARTESIAN_POINT ( 'NONE',  ( 10.49813415415989581, 82.57268628210145778, 7.228626920339068285 ) ) ;
#4464 = CARTESIAN_POINT ( 'NONE',  ( 15.53471296425188797, 11.37731371789854506, 2.908627838312457747 ) ) ;
#4465 = AXIS2_PLACEMENT_3D ( 'NONE', #37028, #37216, #2355 ) ;
#4466 = CARTESIAN_POINT ( 'NONE',  ( 27.84585202812001015, 5.196152422706630247, 162.6695864753947660 ) ) ;
#4467 = CARTESIAN_POINT ( 'NONE',  ( -55.93377896937850124, 208.9097554298617183, 4.530955311639234040 ) ) ;
#4468 = CARTESIAN_POINT ( 'NONE',  ( 15.00000000000001954, -11.99999999999999822, 50.26196565745151190 ) ) ;
#4469 = CARTESIAN_POINT ( 'NONE',  ( 34.20868437832884013, 5.196152422706631135, 166.5548135579648488 ) ) ;
#4470 = CARTESIAN_POINT ( 'NONE',  ( -10.69584247140429412, 126.9523137178985621, -6.932735513424201024 ) ) ;
#4471 = CARTESIAN_POINT ( 'NONE',  ( -48.61830436395490551, 209.8844732041982581, 6.500000000000000888 ) ) ;
#4472 = CARTESIAN_POINT ( 'NONE',  ( -52.18080436395490551, 201.5000000000000000, -0.1155267958017054536 ) ) ;
#4473 = PRODUCT_CONTEXT ( 'NONE', #1567, 'mechanical' ) ;
#4474 = CARTESIAN_POINT ( 'NONE',  ( 15.24356964374999990, 0.000000000000000000, -1.153124999385496396 ) ) ;
#4475 = CARTESIAN_POINT ( 'NONE',  ( 5.778771075727756162E-15, 196.7656250006145342, 31.45816453501075927 ) ) ;
#4476 = CARTESIAN_POINT ( 'NONE',  ( 15.50000000000000533, 112.2898137178985678, -0.1745138560722452326 ) ) ;
#4477 = CARTESIAN_POINT ( 'NONE',  ( -45.64211230271183695, 203.5309553116391612, 1.857196546604092280 ) ) ;
#4478 = ORIENTED_EDGE ( 'NONE', *, *, #22111, .T. ) ;
#4479 = CARTESIAN_POINT ( 'NONE',  ( 31.24297866652485922, -6.928203230275506996, 167.0777818944568480 ) ) ;
#4480 = CARTESIAN_POINT ( 'NONE',  ( 21.00000000000000355, 0.000000000000000000, 50.00000000000001421 ) ) ;
#4481 = EDGE_CURVE ( 'NONE', #19092, #11864, #4231, .T. ) ;
#4482 = CARTESIAN_POINT ( 'NONE',  ( -0.1745138560725817967, 84.01018628210145778, 15.50000000000000533 ) ) ;
#4483 = CYLINDRICAL_SURFACE ( 'NONE', #15052, 25.00000000000000000 ) ;
#4484 = CARTESIAN_POINT ( 'NONE',  ( 31.00030439525832193, 7.209453229046482114, 164.3040022813455039 ) ) ;
#4485 = AXIS2_PLACEMENT_3D ( 'NONE', #6361, #3700, #26630 ) ;
#4486 = CARTESIAN_POINT ( 'NONE',  ( -15.50000000000000533, 77.11018628210145209, -0.1745138560725808530 ) ) ;
#4487 = PRODUCT_DEFINITION_FORMATION_WITH_SPECIFIED_SOURCE ( 'ANY', '', #34976, .NOT_KNOWN. ) ;
#4488 = CARTESIAN_POINT ( 'NONE',  ( -54.35788769728821990, 216.4690446883607535, 1.857196546604031662 ) ) ;
#4489 = CARTESIAN_POINT ( 'NONE',  ( 13.44051670066911619, -5.407089921784859143, -4.565624999385536675 ) ) ;
#4490 = CARTESIAN_POINT ( 'NONE',  ( -6.840914352312096547, 48.36018628210145209, 6.594114490232313663 ) ) ;
#4491 = FACE_OUTER_BOUND ( 'NONE', #25254, .T. ) ;
#4492 = CARTESIAN_POINT ( 'NONE',  ( -37.33705436395491262, 203.8621396198270475, -6.307003348497942419 ) ) ;
#4493 = CARTESIAN_POINT ( 'NONE',  ( 22.80587116629411781, -3.604726614523238837, -9.459374999385545379 ) ) ;
#4494 = CARTESIAN_POINT ( 'NONE',  ( -12.46528703574805697, 77.39768628210144641, -2.660918448318280838 ) ) ;
#4495 = CARTESIAN_POINT ( 'NONE',  ( 13.49999999999999645, 199.8499999999999943, -23.38268590217984766 ) ) ;
#4496 = CARTESIAN_POINT ( 'NONE',  ( 22.60769515458672885, 247.4888461906613770, 5.999999999999997335 ) ) ;
#4498 = CARTESIAN_POINT ( 'NONE',  ( 22.80587116629411781, 3.604726614523243278, -0.8343749993855380520 ) ) ;
#4497 = CARTESIAN_POINT ( 'NONE',  ( -8.843639120294326972, 39.73518628210145209, 3.474262827703335166 ) ) ;
#4499 = CYLINDRICAL_SURFACE ( 'NONE', #1508, 5.999999999999994671 ) ;
#4500 = ORIENTED_EDGE ( 'NONE', *, *, #22553, .F. ) ;
#4501 = CARTESIAN_POINT ( 'NONE',  ( 18.00000000000000355, -5.196152422706632912, -3.074999999999994404 ) ) ;
#4502 = CARTESIAN_POINT ( 'NONE',  ( 37.17109026623309376, 7.646167579472024665E-16, 163.1994798139711520 ) ) ;
#4503 = CARTESIAN_POINT ( 'NONE',  ( 36.71028575989448228, 7.347880794884125653E-16, 160.7271084529098744 ) ) ;
#4504 = CARTESIAN_POINT ( 'NONE',  ( 26.99999999999999645, 244.8249999999999886, -7.347880794884117764E-16 ) ) ;
#4505 = CARTESIAN_POINT ( 'NONE',  ( 16.56230152254410726, 0.000000000000000000, 2.535898384862258492 ) ) ;
#4506 = EDGE_CURVE ( 'NONE', #2146, #12569, #26067, .T. ) ;
#4507 = CARTESIAN_POINT ( 'NONE',  ( 12.53471296425189330, 75.77731371789855075, 2.311890736173451977 ) ) ;
#4508 = CARTESIAN_POINT ( 'NONE',  ( -6.932735513423968321, 78.54768628210145209, -10.69584247140445221 ) ) ;
#4509 = ORIENTED_EDGE ( 'NONE', *, *, #18682, .T. ) ;
#4510 = ORIENTED_EDGE ( 'NONE', *, *, #6847, .F. ) ;
#4511 = CARTESIAN_POINT ( 'NONE',  ( -27.00000000000000355, 198.3125000012290400, 0.000000000000000000 ) ) ;
#4512 = CARTESIAN_POINT ( 'NONE',  ( 19.39230484541326049, 248.6138461906613770, -5.999999999999997335 ) ) ;
#4513 = CARTESIAN_POINT ( 'NONE',  ( -15.50000000000000533, 61.68981371789855928, 0.1745138560722471477 ) ) ;
#4514 =( BOUNDED_CURVE ( )  B_SPLINE_CURVE ( 2, ( #31991, #516, #32364, #23657, #23466, #32548, #35200, #9250, #20823 ),
 .UNSPECIFIED., .F., .F. ) 
 B_SPLINE_CURVE_WITH_KNOTS ( ( 3, 2, 2, 2, 3 ),
 ( 0.02083333333333333565, 0.02777777777777777624, 0.04166666666666666435, 0.05555555555555555247, 0.06250000000000000000 ),
 .UNSPECIFIED. ) 
 CURVE ( )  GEOMETRIC_REPRESENTATION_ITEM ( )  RATIONAL_B_SPLINE_CURVE ( ( 0.9330127018922194093, 0.9330127018922194093, 1.000000000000000000, 0.8660254037844387076, 1.000000000000000000, 0.8660254037844387076, 1.000000000000000000, 0.9330127018922194093, 0.9330127018922194093 ) ) 
 REPRESENTATION_ITEM ( '' )  );
#4515 = CARTESIAN_POINT ( 'NONE',  ( 23.87821517812499650, 4.985214923628404904, -6.253124999385489602 ) ) ;
#4516 = EDGE_CURVE ( 'NONE', #10660, #6278, #34966, .T. ) ;
#4517 = CARTESIAN_POINT ( 'NONE',  ( 21.00000000000000000, 245.2468750006145228, -6.646953231504538984 ) ) ;
#4518 = CARTESIAN_POINT ( 'NONE',  ( -51.58705436395489841, 206.7903428501026042, -3.378800118222489157 ) ) ;
#4519 = CARTESIAN_POINT ( 'NONE',  ( 37.41951561650326852, 3.464101615137893386, 168.8336428086315095 ) ) ;
#4520 = CARTESIAN_POINT ( 'NONE',  ( -8.152565276336593669, 53.35231371789856780, -5.233372021372610483 ) ) ;
#4521 = CARTESIAN_POINT ( 'NONE',  ( 13.44051670066911264, 5.407089921784856479, -8.765624999385545735 ) ) ;
#4522 = CARTESIAN_POINT ( 'NONE',  ( 7.954856959092311719, 93.02731371789853654, -5.529263428287300108 ) ) ;
#4523 = CARTESIAN_POINT ( 'NONE',  ( -4.694659320240884604E-14, 197.8625000000000114, 27.00000000000000000 ) ) ;
#4524 = CARTESIAN_POINT ( 'NONE',  ( -4.944772684328424539, 26.61481371789854578, -11.48171059495408031 ) ) ;
#4525 = CARTESIAN_POINT ( 'NONE',  ( -12.50000000000000355, 77.11018628210145209, -0.1745138560725492671 ) ) ;
#4526 = CARTESIAN_POINT ( 'NONE',  ( 10.56230152254411436, -3.464101615137757051, -8.399999998770997678 ) ) ;
#4527 = SHAPE_REPRESENTATION ( 'follower plate', ( #17215 ), #16540 ) ;
#4528 = DIRECTION ( 'NONE',  ( -0.000000000000000000, -1.000000000000000000, -0.000000000000000000 ) ) ;
#4529 = CARTESIAN_POINT ( 'NONE',  ( 37.06160086440634416, 3.604726614523238837, 161.9480102244933732 ) ) ;
#4530 = CARTESIAN_POINT ( 'NONE',  ( 10.31873187879410736, 3.604726614523240613, -6.084374999385531169 ) ) ;
#4531 = EDGE_CURVE ( 'NONE', #32891, #23955, #23233, .T. ) ;
#4532 = LINE ( 'NONE', #16293, #34504 ) ;
#4533 = CARTESIAN_POINT ( 'NONE',  ( -6.840914352312096547, 94.36018628210146630, 6.594114490232313663 ) ) ;
#4534 = DIRECTION ( 'NONE',  ( 0.000000000000000000, 1.000000000000000000, 0.000000000000000000 ) ) ;
#4535 = CARTESIAN_POINT ( 'NONE',  ( -2.660918448318275509, 130.2976862821014379, 12.46528703574805874 ) ) ;
#4536 = CARTESIAN_POINT ( 'NONE',  ( 13.56230152254410548, 5.196152422706636465, -4.575000000000050804 ) ) ;
#4537 = CARTESIAN_POINT ( 'NONE',  ( 21.00000000000000000, 249.2968750006145342, -6.646953231504538984 ) ) ;
#4538 = ORIENTED_EDGE ( 'NONE', *, *, #36547, .F. ) ;
#4539 = CARTESIAN_POINT ( 'NONE',  ( 31.06403703214253653, -7.209453229046475009, 165.0324696543250411 ) ) ;
#4540 = CARTESIAN_POINT ( 'NONE',  ( 26.75643035624999655, 3.323476615752271712, -4.378124999385460292 ) ) ;
#4542 = ADVANCED_FACE ( 'NONE', ( #8274 ), #11657, .T. ) ;
#4541 = CARTESIAN_POINT ( 'NONE',  ( -27.24356964375000345, 197.5718750006145115, -15.72908226750537786 ) ) ;
#4543 = CARTESIAN_POINT ( 'NONE',  ( 37.41297893579741896, -3.464101615137755275, 168.7589282062745610 ) ) ;
#4544 = DIRECTION ( 'NONE',  ( -1.000000000000000000, 0.000000000000000000, 0.000000000000000000 ) ) ;
#4545 = CARTESIAN_POINT ( 'NONE',  ( 18.12178482187499640, 242.5843750006145285, -4.985214923628404904 ) ) ;
#4546 = CARTESIAN_POINT ( 'NONE',  ( -70.80918835584510873, 215.2843023367891249, -7.500000000000000000 ) ) ;
#4547 = AXIS2_PLACEMENT_3D ( 'NONE', #25714, #19863, #111 ) ;
#4548 = CARTESIAN_POINT ( 'NONE',  ( -2.311890736173448424, 133.2773137178985507, 12.53471296425189330 ) ) ;
#4549 = CARTESIAN_POINT ( 'NONE',  ( 12.50000000000000355, 136.9101862821014777, 0.1745138560725507937 ) ) ;
#4551 = VERTEX_POINT ( 'NONE', #16991 ) ;
#4550 = VERTEX_POINT ( 'NONE', #20205 ) ;
#4552 = CARTESIAN_POINT ( 'NONE',  ( 15.24356964375000167, 243.4843750006145058, 3.323476615752272600 ) ) ;
#4553 = EDGE_CURVE ( 'NONE', #149, #20414, #27964, .T. ) ;
#4554 = CARTESIAN_POINT ( 'NONE',  ( -2.660918448318005058, 8.502313717898557499, -12.46528703574811558 ) ) ;
#4555 = CARTESIAN_POINT ( 'NONE',  ( 26.75643035624999655, -3.323476615752267715, -4.453124999385455141 ) ) ;
#4556 = CARTESIAN_POINT ( 'NONE',  ( 6.092822981423662299, 114.0148137178985763, 14.25334919248795096 ) ) ;
#4557 = CARTESIAN_POINT ( 'NONE',  ( 15.00000000000000000, 3.464101615137752166, -8.981249998770968190 ) ) ;
#4558 = CARTESIAN_POINT ( 'NONE',  ( 22.80587116629411781, 3.604726614523243278, -5.784374999385524241 ) ) ;
#4559 = ORIENTED_EDGE ( 'NONE', *, *, #15916, .F. ) ;
#4560 = CARTESIAN_POINT ( 'NONE',  ( 13.62178482187499640, 196.0531250006145285, -23.59362340125807123 ) ) ;
#4561 = CARTESIAN_POINT ( 'NONE',  ( -11.61527771782819940, 131.7351862821014663, 4.622313124798574258 ) ) ;
#4562 = CARTESIAN_POINT ( 'NONE',  ( 22.80587116629410716, -3.604726614523235284, -0.8531249993855525293 ) ) ;
#4563 = CARTESIAN_POINT ( 'NONE',  ( 36.89328133622495898, -3.604726614523238837, 160.0241092138036834 ) ) ;
#4564 = CARTESIAN_POINT ( 'NONE',  ( -59.89211230271182274, 201.5309553116392181, 2.393094931466368980 ) ) ;
#4565 = CARTESIAN_POINT ( 'NONE',  ( 23.87821517812499650, 245.9968750006145228, -4.985214923628404904 ) ) ;
#4566 =( LENGTH_UNIT ( ) NAMED_UNIT ( * ) SI_UNIT ( .MILLI., .METRE. ) );
#4567 = CARTESIAN_POINT ( 'NONE',  ( -26.99999999999999645, 197.4500000012290002, 15.58845726811991561 ) ) ;
#4568 = CARTESIAN_POINT ( 'NONE',  ( -31.39211230271183339, 205.5309553116392465, 1.321298161741817356 ) ) ;
#4569 = CARTESIAN_POINT ( 'NONE',  ( 18.00000000000000000, 245.8750000000000000, -5.196152422706630247 ) ) ;
#4570 = CARTESIAN_POINT ( 'NONE',  ( 13.56230152254410548, 5.196152422706630247, -1.762499998771011045 ) ) ;
#4571 = ORIENTED_EDGE ( 'NONE', *, *, #13873, .T. ) ;
#4572 = AXIS2_PLACEMENT_3D ( 'NONE', #26454, #29864, #27025 ) ;
#4573 = CARTESIAN_POINT ( 'NONE',  ( 0.000000000000000000, 0.000000000000000000, 0.000000000000000000 ) ) ;
#4574 = CARTESIAN_POINT ( 'NONE',  ( 10.56230152254410903, 0.000000000000000000, -1.237499998771041110 ) ) ;
#4575 = CARTESIAN_POINT ( 'NONE',  ( -6.092822981423970496, 121.3851862821014578, 14.25334919248782661 ) ) ;
#4576 = CARTESIAN_POINT ( 'NONE',  ( 0.1745138560725194299, 116.2101862821014748, -9.500000000000005329 ) ) ;
#4577 = EDGE_CURVE ( 'NONE', #10335, #5564, #37064, .T. ) ;
#4578 = CARTESIAN_POINT ( 'NONE',  ( 24.00000000000000000, 242.5562500012290457, 5.196152422706629359 ) ) ;
#4579 = CARTESIAN_POINT ( 'NONE',  ( 8.715434833791931624, 18.46018628210144286, 8.962234695871760692 ) ) ;
#4580 = CARTESIAN_POINT ( 'NONE',  ( 19.56230152254412502, -5.196152422706635576, -8.850000000000052935 ) ) ;
#4581 = ORIENTED_EDGE ( 'NONE', *, *, #28607, .F. ) ;
#4582 = DIRECTION ( 'NONE',  ( 1.000000000000000000, 0.000000000000000000, 0.000000000000000000 ) ) ;
#4583 = CARTESIAN_POINT ( 'NONE',  ( -3.474262827703337830, 78.83518628210146062, -8.843639120294326972 ) ) ;
#4584 = CARTESIAN_POINT ( 'NONE',  ( 23.99999999999999645, 244.0562500012290457, -5.196152422706631135 ) ) ;
#4585 = CARTESIAN_POINT ( 'NONE',  ( 0.1745138560723095977, 132.9898137178985564, 9.500000000000005329 ) ) ;
#4586 = CARTESIAN_POINT ( 'NONE',  ( -27.24356964375000345, 197.1031250006145399, 0.000000000000000000 ) ) ;
#4587 = CARTESIAN_POINT ( 'NONE',  ( 26.99999999999999645, 7.347880794884117764E-16, -6.525000000000003020 ) ) ;
#4588 = CARTESIAN_POINT ( 'NONE',  ( -27.24356964375000345, 197.1593750006145456, 0.000000000000000000 ) ) ;
#4589 = CARTESIAN_POINT ( 'NONE',  ( 33.98970557456826214, -5.196152422706635576, 164.0518743777849409 ) ) ;
#4590 = CARTESIAN_POINT ( 'NONE',  ( 16.56230152254411081, 6.928203230275514990, -3.712500000000020339 ) ) ;
#4591 = CARTESIAN_POINT ( 'NONE',  ( 8.843639120294245259, 57.66481371789855359, 3.474262827703527901 ) ) ;
#4592 = ORIENTED_EDGE ( 'NONE', *, *, #7163, .T. ) ;
#4593 = CARTESIAN_POINT ( 'NONE',  ( 26.99999999999999645, 240.4187500012290286, -3.464101615137755275 ) ) ;
#4594 = CARTESIAN_POINT ( 'NONE',  ( 0.1745138560722779009, 86.98981371789855643, 12.50000000000000355 ) ) ;
#4595 = CARTESIAN_POINT ( 'NONE',  ( 16.56230152254411436, -7.209453229046482114, -6.384374999385507010 ) ) ;
#4596 = CARTESIAN_POINT ( 'NONE',  ( 27.24356964374999635, 199.6156250006145285, -15.72908226750539029 ) ) ;
#4597 = CARTESIAN_POINT ( 'NONE',  ( 26.75643035624999655, -3.323476615752267715, -8.165624999385475036 ) ) ;
#4598 = CARTESIAN_POINT ( 'NONE',  ( -11.61527771782809282, 25.46481371789855075, -4.622313124798832717 ) ) ;
#4599 = ORIENTED_EDGE ( 'NONE', *, *, #27014, .T. ) ;
#4600 = CARTESIAN_POINT ( 'NONE',  ( 23.87821517812499650, 4.985214923628404904, -6.590624999385480187 ) ) ;
#4601 = CARTESIAN_POINT ( 'NONE',  ( -7.228626920339069173, 20.47268628210144570, 10.49813415415989581 ) ) ;
#4602 = CARTESIAN_POINT ( 'NONE',  ( 37.59924285248093412, -3.604726614523238837, 168.0932862683468443 ) ) ;
#4603 = CARTESIAN_POINT ( 'NONE',  ( -51.77752896937849414, 213.3500491399821613, 5.571401726697954970 ) ) ;
#4604 = CARTESIAN_POINT ( 'NONE',  ( 16.56230152254410726, 0.000000000000000000, -10.00000000000000000 ) ) ;
#4605 = CARTESIAN_POINT ( 'NONE',  ( -11.61527771782809282, 71.46481371789856496, -4.622313124798832717 ) ) ;
#4606 = CARTESIAN_POINT ( 'NONE',  ( -50.00372103062156981, 214.5309553116392749, -1.090244570138262148 ) ) ;
#4607 = CARTESIAN_POINT ( 'NONE',  ( -60.69122103062155560, 208.3738570449993404, -6.530955311639226935 ) ) ;
#4608 = CARTESIAN_POINT ( 'NONE',  ( 3.306546357697854128E-15, 200.0000000000000000, 27.00000000000000355 ) ) ;
#4609 = DIRECTION ( 'NONE',  ( 1.000000000000000000, 6.123233995736766036E-17, 0.000000000000000000 ) ) ;
#4610 = CARTESIAN_POINT ( 'NONE',  ( -6.092822981423666739, 45.01481371789854791, -14.25334919248795096 ) ) ;
#4611 = CARTESIAN_POINT ( 'NONE',  ( -41.09002896937850124, 202.6965474657332038, 4.350049139982197666 ) ) ;
#4612 =( BOUNDED_CURVE ( )  B_SPLINE_CURVE ( 2, ( #7079, #32835, #6879, #15792, #27156, #29997, #9727 ),
 .UNSPECIFIED., .F., .F. ) 
 B_SPLINE_CURVE_WITH_KNOTS ( ( 3, 2, 2, 3 ),
 ( 0.7826086956521727256, 0.7898550724637667386, 0.7971014492753607517, 0.8043478260869548757 ),
 .UNSPECIFIED. ) 
 CURVE ( )  GEOMETRIC_REPRESENTATION_ITEM ( )  RATIONAL_B_SPLINE_CURVE ( ( 1.000000000000022649, 0.8660254037844161701, 1.000000000000000000, 0.8660254037844387076, 1.000000000000000000, 0.8660254037844694608, 0.9999999999999692468 ) ) 
 REPRESENTATION_ITEM ( '' )  );
#4613 = CARTESIAN_POINT ( 'NONE',  ( 7.234628195640322446, 199.6825961894323598, 26.99999999999999645 ) ) ;
#4614 = CARTESIAN_POINT ( 'NONE',  ( -12.46528703574805697, 68.19768628210144357, -2.660918448318280838 ) ) ;
#4615 = EDGE_CURVE ( 'NONE', #20931, #12997, #25698, .T. ) ;
#4616 = CARTESIAN_POINT ( 'NONE',  ( 8.927990412390657937, 15.87268628210144605, -13.04141134922759804 ) ) ;
#4617 = MECHANICAL_DESIGN_GEOMETRIC_PRESENTATION_REPRESENTATION (  '', ( #24602 ), #31250 ) ;
#4618 = CARTESIAN_POINT ( 'NONE',  ( 22.56230152254412857, -3.464101615137755275, -2.512500000000021494 ) ) ;
#4619 = CARTESIAN_POINT ( 'NONE',  ( 20.99999999999999289, 244.0937500012290116, -5.999999999999997335 ) ) ;
#4620 = ORIENTED_EDGE ( 'NONE', *, *, #20907, .T. ) ;
#4621 = CARTESIAN_POINT ( 'NONE',  ( -15.46528703574804986, 22.19768628210144001, -3.257655550457287497 ) ) ;
#4622 = CARTESIAN_POINT ( 'NONE',  ( 5.778771075727756162E-15, 198.1156250006145285, 31.45816453501076637 ) ) ;
#4623 = CARTESIAN_POINT ( 'NONE',  ( -27.24356964375000345, 199.4093750006145456, 0.000000000000000000 ) ) ;
#4624 = CARTESIAN_POINT ( 'NONE',  ( 31.11551339264930860, -6.928203230275514990, 165.6208471472733095 ) ) ;
#4625 = LINE ( 'NONE', #9762, #14797 ) ;
#4626 = CARTESIAN_POINT ( 'NONE',  ( -10.49813415415989581, 4.372686282101440725, -7.228626920339068285 ) ) ;
#4627 = CARTESIAN_POINT ( 'NONE',  ( 15.24356964374999990, 248.4718750006145171, -3.323476615752268604 ) ) ;
#4628 = CARTESIAN_POINT ( 'NONE',  ( 8.152565276336593669, 103.9523137178985763, 5.233372021372610483 ) ) ;
#4629 = CARTESIAN_POINT ( 'NONE',  ( 18.12178482187500350, 243.6343750006145115, 4.985214923628407568 ) ) ;
#4630 = ORIENTED_EDGE ( 'NONE', *, *, #11394, .T. ) ;
#4631 = AXIS2_PLACEMENT_3D ( 'NONE', #8852, #2599, #6000 ) ;
#4632 = CARTESIAN_POINT ( 'NONE',  ( 20.99999999999999645, 185.0294372515228645, 0.000000000000000000 ) ) ;
#4633 = CARTESIAN_POINT ( 'NONE',  ( -5.558451987054219501, 142.8813032066705944, 11.24274018108063267 ) ) ;
#4634 = CARTESIAN_POINT ( 'NONE',  ( 22.80587116629411426, -3.604726614523235284, -8.053124999385516958 ) ) ;
#4635 = CARTESIAN_POINT ( 'NONE',  ( 31.06403703214253653, -7.209453229046475009, 165.0324696543250411 ) ) ;
#4636 = CARTESIAN_POINT ( 'NONE',  ( 6.123233995736766282E-16, 2.000000000000000000, 5.000000000000000000 ) ) ;
#4637 = CARTESIAN_POINT ( 'NONE',  ( -13.49999999999998401, 197.3750000000000284, 23.38268590217985476 ) ) ;
#4638 = VERTEX_POINT ( 'NONE', #31754 ) ;
#4639 = CARTESIAN_POINT ( 'NONE',  ( -12.53471296425194659, 40.02268628210143930, 2.311890736173176641 ) ) ;
#4640 = ORIENTED_EDGE ( 'NONE', *, *, #22827, .F. ) ;
#4641 = ORIENTED_EDGE ( 'NONE', *, *, #36536, .T. ) ;
#4642 = CARTESIAN_POINT ( 'NONE',  ( 18.00000000000000000, 5.196152422706630247, -5.418749998770955756 ) ) ;
#4643 = DIRECTION ( 'NONE',  ( 0.000000000000000000, 0.000000000000000000, -1.000000000000000000 ) ) ;
#4644 = CARTESIAN_POINT ( 'NONE',  ( 27.00000000000036593, 3.464101615137540779, -4.687500000000010658 ) ) ;
#4645 = CARTESIAN_POINT ( 'NONE',  ( 15.24356964374999990, 3.323476615752268604, -8.728124999385462601 ) ) ;
#4646 = CARTESIAN_POINT ( 'NONE',  ( 4.944772684328679446, 79.98518628210145209, -11.48171059495397373 ) ) ;
#4647 = CARTESIAN_POINT ( 'NONE',  ( -8.927990412390661490, 140.0726862821014151, 13.04141134922759804 ) ) ;
#4648 = CARTESIAN_POINT ( 'NONE',  ( -64.64211230271182274, 203.5309553116391896, 1.857196546604092724 ) ) ;
#4649 = CARTESIAN_POINT ( 'NONE',  ( 14.14550961275805996, 216.8544903872546286, 0.3345106846866886530 ) ) ;
#4650 = CARTESIAN_POINT ( 'NONE',  ( -60.09002896937850124, 206.1606490808709111, 2.350049139982143931 ) ) ;
#4651 = DIRECTION ( 'NONE',  ( 0.000000000000000000, 0.000000000000000000, 1.000000000000000000 ) ) ;
#4652 = CARTESIAN_POINT ( 'NONE',  ( 31.14492845593375847, 6.928203230275506996, 165.9570628591036439 ) ) ;
#4653 = CARTESIAN_POINT ( 'NONE',  ( -12.53471296425189152, 117.1773137178985564, -2.311890736173453753 ) ) ;
#4654 = CARTESIAN_POINT ( 'NONE',  ( -41.29538769728821990, 211.8571965466039444, -6.469044688360768625 ) ) ;
#4655 = CARTESIAN_POINT ( 'NONE',  ( -52.37872103062156981, 201.4690446883607819, 2.162041339862843525 ) ) ;
#4656 = CARTESIAN_POINT ( 'NONE',  ( 15.24356964374999990, 0.000000000000000000, -2.953124999385492444 ) ) ;
#4657 = CARTESIAN_POINT ( 'NONE',  ( 13.62178482187499640, 197.4031250006145228, -23.59362340125807123 ) ) ;
#4658 = CARTESIAN_POINT ( 'NONE',  ( 14.38691631536194393, 103.6648137178985678, 5.770363421894124656 ) ) ;
#4659 = CARTESIAN_POINT ( 'NONE',  ( -49.40252896937850124, 206.6499508600178387, -5.571401726697954970 ) ) ;
#4660 = AXIS2_PLACEMENT_3D ( 'NONE', #10118, #16561, #4796 ) ;
#4661 = ORIENTED_EDGE ( 'NONE', *, *, #25880, .F. ) ;
#4662 = CARTESIAN_POINT ( 'NONE',  ( 20.99999999999999645, 185.0294372515228645, 0.000000000000000000 ) ) ;
#4663 = CARTESIAN_POINT ( 'NONE',  ( -7.228626920339069173, 130.8726862821014834, 10.49813415415989581 ) ) ;
#4664 = CARTESIAN_POINT ( 'NONE',  ( -8.927990412390661490, 75.67268628210143788, 13.04141134922759804 ) ) ;
#4665 = CARTESIAN_POINT ( 'NONE',  ( -70.80918835584510873, 215.2843023367891249, 7.500000000000000000 ) ) ;
#4666 = CARTESIAN_POINT ( 'NONE',  ( 34.10694154304044901, 5.407089921784862696, 163.9945635053181547 ) ) ;
#4667 = CARTESIAN_POINT ( 'NONE',  ( -13.23911966647218463, 76.24768628210145494, 8.632099005475506459 ) ) ;
#4668 = CARTESIAN_POINT ( 'NONE',  ( -53.76413769728823411, 213.1499508600178672, 5.686928522499718142 ) ) ;
#4669 = CARTESIAN_POINT ( 'NONE',  ( 22.80587116629411071, -3.604726614523235284, -4.903124999385513938 ) ) ;
#4670 = CARTESIAN_POINT ( 'NONE',  ( -7.954856959092191815, 31.97268628210143149, -5.529263428287477744 ) ) ;
#4671 = CARTESIAN_POINT ( 'NONE',  ( 36.90638618107669799, 7.347880794884125653E-16, 162.9685465236163111 ) ) ;
#4672 = CARTESIAN_POINT ( 'NONE',  ( -69.79538769728823411, 211.8571965466039444, -6.469044688360768625 ) ) ;
#4673 = CARTESIAN_POINT ( 'NONE',  ( 13.44051670066911441, -5.407089921784865361, -9.571874999385554972 ) ) ;
#4674 = ADVANCED_FACE ( 'NONE', ( #14328 ), #14511, .F. ) ;
#4675 = CARTESIAN_POINT ( 'NONE',  ( -8.962234695871760692, 66.76018628210145778, 8.715434833791933400 ) ) ;
#4676 = CARTESIAN_POINT ( 'NONE',  ( 5.727106289114498080E-15, 199.6625000000000227, 31.17691453623979214 ) ) ;
#4677 = DIRECTION ( 'NONE',  ( 0.08715574274765150453, 0.000000000000000000, 0.9961946980917461003 ) ) ;
#4679 = CARTESIAN_POINT ( 'NONE',  ( 19.68408634441911076, 5.407089921784862696, -1.696874999385505900 ) ) ;
#4678 = CARTESIAN_POINT ( 'NONE',  ( -8.710071997420127943, 50.08518628210143930, -3.796722387233380402 ) ) ;
#4680 = DIRECTION ( 'NONE',  ( 1.000000000000000000, 0.000000000000000000, 0.000000000000000000 ) ) ;
#4681 = VERTEX_POINT ( 'NONE', #22866 ) ;
#4682 = CARTESIAN_POINT ( 'NONE',  ( 21.00000000000000000, 6.928203230275506996, -1.912500000000006084 ) ) ;
#4683 =( BOUNDED_CURVE ( )  B_SPLINE_CURVE ( 2, ( #30317, #36175, #10221, #21795, #4341, #15921, #33348 ),
 .UNSPECIFIED., .F., .F. ) 
 B_SPLINE_CURVE_WITH_KNOTS ( ( 3, 2, 2, 3 ),
 ( 0.3260869565217381361, 0.3333333333333324267, 0.3405797101449267172, 0.3478260869565210078 ),
 .UNSPECIFIED. ) 
 CURVE ( )  GEOMETRIC_REPRESENTATION_ITEM ( )  RATIONAL_B_SPLINE_CURVE ( ( 1.000000000000018430, 0.8660254037844202779, 1.000000000000000000, 0.8660254037844387076, 1.000000000000000000, 0.8660254037844520303, 0.9999999999999866773 ) ) 
 REPRESENTATION_ITEM ( '' )  );
#4684 = CARTESIAN_POINT ( 'NONE',  ( 27.71064018770612947, -5.407089921784865361, 162.5214321913800859 ) ) ;
#4685 = CARTESIAN_POINT ( 'NONE',  ( 24.85399959338462139, 0.000000000000000000, 162.8936964012349051 ) ) ;
#4686 = CARTESIAN_POINT ( 'NONE',  ( 26.99999999999999645, 246.5874999999999773, 3.464101615137751278 ) ) ;
#4687 = CARTESIAN_POINT ( 'NONE',  ( -80.47386374675558329, 210.4269316912311183, 5.000000000000000000 ) ) ;
#4688 = CARTESIAN_POINT ( 'NONE',  ( -4.944772684328424539, 91.01481371789856212, -11.48171059495408031 ) ) ;
#4689 = CARTESIAN_POINT ( 'NONE',  ( 12.53471296425194659, 90.62268628210145494, -2.311890736173178418 ) ) ;
#4690 = ORIENTED_EDGE ( 'NONE', *, *, #23960, .T. ) ;
#4691 = ORIENTED_EDGE ( 'NONE', *, *, #13324, .T. ) ;
#4692 = CARTESIAN_POINT ( 'NONE',  ( 13.49999999999999645, 198.6125000012290513, -23.38268590217984766 ) ) ;
#4693 = CARTESIAN_POINT ( 'NONE',  ( 27.00000000000018474, -3.464101615137644696, -3.862499999999974953 ) ) ;
#4694 = AXIS2_PLACEMENT_3D ( 'NONE', #5646, #19525, #28580 ) ;
#4695 = CARTESIAN_POINT ( 'NONE',  ( -10.83675517735179028, 60.53981371789856070, 11.08355503943118947 ) ) ;
#4696 = EDGE_CURVE ( 'NONE', #27232, #16220, #28719, .T. ) ;
#4697 = CARTESIAN_POINT ( 'NONE',  ( 26.75643035624999655, 7.049594010296217766E-16, -7.678124999385471661 ) ) ;
#4698 = CARTESIAN_POINT ( 'NONE',  ( 21.00000000000000000, 244.1218750006145513, 6.646953231504538984 ) ) ;
#4699 = ADVANCED_FACE ( 'NONE', ( #2388 ), #34416, .F. ) ;
#4700 = CARTESIAN_POINT ( 'NONE',  ( -57.72247103062156270, 207.6499508600178387, 3.839350919129076445 ) ) ;
#4701 = DIRECTION ( 'NONE',  ( 1.000000000000000000, 0.000000000000000000, 0.000000000000000000 ) ) ;
#4702 = CARTESIAN_POINT ( 'NONE',  ( 9.500000000000005329, 38.68981371789855217, -0.1745138560723090149 ) ) ;
#4703 = CARTESIAN_POINT ( 'NONE',  ( 10.31873187879411091, 3.604726614523236616, -8.278124999385530813 ) ) ;
#4704 = CARTESIAN_POINT ( 'NONE',  ( 6.594114490232462877, 92.73981371789854222, -6.840914352311949109 ) ) ;
#4705 = CARTESIAN_POINT ( 'NONE',  ( -27.24356964375000345, 198.0593750006145513, 0.000000000000000000 ) ) ;
#4706 = CARTESIAN_POINT ( 'NONE',  ( -6.932735513424201912, 14.25231371789853441, 10.69584247140429412 ) ) ;
#4707 = CARTESIAN_POINT ( 'NONE',  ( 4.622313124798573369, 74.23518628210145209, 11.61527771782819940 ) ) ;
#4708 = CARTESIAN_POINT ( 'NONE',  ( 10.56230152254411436, -3.464101615137757051, -8.849999998770995191 ) ) ;
#4709 = CARTESIAN_POINT ( 'NONE',  ( -14.50000000000000533, 237.0000000000000000, -2.500000000000000000 ) ) ;
#4710 = CARTESIAN_POINT ( 'NONE',  ( 24.48470861703815515, -3.604726614523240613, 161.4673294743943188 ) ) ;
#4711 = CARTESIAN_POINT ( 'NONE',  ( 18.00000000000000000, 5.196152422706630247, -0.9187499987709513150 ) ) ;
#4712 = CARTESIAN_POINT ( 'NONE',  ( 16.56230152254411436, 7.209453229046482114, -5.259374999385500793 ) ) ;
#4713 = CARTESIAN_POINT ( 'NONE',  ( 27.88834045260238526, -5.196152422706638241, 163.1552313894900976 ) ) ;
#4714 = AXIS2_PLACEMENT_3D ( 'NONE', #16980, #85, #37056 ) ;
#4715 = CARTESIAN_POINT ( 'NONE',  ( -7.234628195640263826, 195.5200961906613770, -27.00000000000003553 ) ) ;
#4716 = CARTESIAN_POINT ( 'NONE',  ( 1.715153634034233487, 102.1226862821014549, 9.534712964251941258 ) ) ;
#4717 = CARTESIAN_POINT ( 'NONE',  ( 38.04237167757703020, 114.1383727779938511, -2.499999999999996447 ) ) ;
#4718 = EDGE_CURVE ( 'NONE', #32501, #13274, #11111, .T. ) ;
#4719 = CARTESIAN_POINT ( 'NONE',  ( 12.46528703574805874, 109.5976862821014493, 2.660918448318279950 ) ) ;
#4720 = CARTESIAN_POINT ( 'NONE',  ( 20.99999999999997513, 246.2874999999999943, -5.999999999999999112 ) ) ;
#4721 = CARTESIAN_POINT ( 'NONE',  ( 26.75643035624999655, 249.1468750006145285, 3.323476615752267715 ) ) ;
#4722 = VERTEX_POINT ( 'NONE', #29467 ) ;
#4723 = CARTESIAN_POINT ( 'NONE',  ( 24.75924920669325502, -3.604726614523240613, 164.6053427733833416 ) ) ;
#4724 = AXIS2_PLACEMENT_3D ( 'NONE', #18969, #19161, #22183 ) ;
#4725 = CARTESIAN_POINT ( 'NONE',  ( 26.75643035624999655, 7.049594010296217766E-16, -4.415624999385469707 ) ) ;
#4726 = CARTESIAN_POINT ( 'NONE',  ( -27.24356964375000345, 198.9593750006145285, 0.000000000000000000 ) ) ;
#4727 = CARTESIAN_POINT ( 'NONE',  ( 15.08123753375185849, -0.4834061343151928591, -8.000000000000001776 ) ) ;
#4728 =( BOUNDED_CURVE ( )  B_SPLINE_CURVE ( 2, ( #21610, #33160, #4899, #16481, #7206 ),
 .UNSPECIFIED., .F., .F. ) 
 B_SPLINE_CURVE_WITH_KNOTS ( ( 3, 2, 3 ),
 ( 0.000000000000000000, 0.01388888888888888985, 0.02083333333333333565 ),
 .UNSPECIFIED. ) 
 CURVE ( )  GEOMETRIC_REPRESENTATION_ITEM ( )  RATIONAL_B_SPLINE_CURVE ( ( 1.000000000000000000, 0.8660254037844387076, 1.000000000000000000, 0.9330127018922192983, 0.9330127018922194093 ) ) 
 REPRESENTATION_ITEM ( '' )  );
#4729 = CARTESIAN_POINT ( 'NONE',  ( 25.39981243234178976, 3.464101615137757051, 169.1323656980344765 ) ) ;
#4730 = CARTESIAN_POINT ( 'NONE',  ( 24.70038759679241736, -3.464101615138067469, 161.1379032458481788 ) ) ;
#4731 = CARTESIAN_POINT ( 'NONE',  ( 23.87821517812500005, 241.9093750006145456, 4.985214923628404016 ) ) ;
#4732 = CARTESIAN_POINT ( 'NONE',  ( 36.99463137071579411, 7.347880794884117764E-16, 163.9771936566585566 ) ) ;
#4733 = CARTESIAN_POINT ( 'NONE',  ( -6.840914352311947333, 7.639813717898540801, -6.594114490232462877 ) ) ;
#4734 = CARTESIAN_POINT ( 'NONE',  ( -27.24356964374999279, 194.9468750006145683, 15.72908226750539384 ) ) ;
#4736 = ORIENTED_EDGE ( 'NONE', *, *, #8440, .F. ) ;
#4735 = ORIENTED_EDGE ( 'NONE', *, *, #11334, .F. ) ;
#4737 = CARTESIAN_POINT ( 'NONE',  ( 15.24356964374999990, 244.7968750006145058, 0.000000000000000000 ) ) ;
#4738 = CARTESIAN_POINT ( 'NONE',  ( 8.715434833792128799, 9.939813717898537959, -8.962234695871567070 ) ) ;
#4739 = CARTESIAN_POINT ( 'NONE',  ( 23.87821517812499650, 4.985214923628404904, -4.790624999385456384 ) ) ;
#4740 = CARTESIAN_POINT ( 'NONE',  ( 2.908627838312458636, 110.2773137178985650, -15.53471296425188442 ) ) ;
#4741 = CARTESIAN_POINT ( 'NONE',  ( 13.34266913871822346, -5.365490278403956204, -9.999999999999996447 ) ) ;
#4742 = EDGE_CURVE ( 'NONE', #18566, #29619, #20741, .T. ) ;
#4743 = CARTESIAN_POINT ( 'NONE',  ( 21.00000000000000000, 6.928203230275506996, -9.956249998770953624 ) ) ;
#4744 = CLOSED_SHELL ( 'NONE', ( #24245, #27494, #28200, #19192, #1293, #6469, #32100, #16308, #5411, #18285, #28238, #3315, #20115, #18072, #18295, #24769, #16663, #12725 ) ) ;
#4745 = AXIS2_PLACEMENT_3D ( 'NONE', #5039, #19291, #16984 ) ;
#4746 = CARTESIAN_POINT ( 'NONE',  ( 10.31873187879410736, 3.604726614523240613, -7.434374999385486404 ) ) ;
#4747 = ORIENTED_EDGE ( 'NONE', *, *, #26822, .F. ) ;
#4748 = CARTESIAN_POINT ( 'NONE',  ( 27.24356964375000345, 195.0781250006145342, -3.336375036156643733E-15 ) ) ;
#4749 = CARTESIAN_POINT ( 'NONE',  ( 10.69584247140445221, 108.4476862821014578, -6.932735513423970097 ) ) ;
#4750 = DIRECTION ( 'NONE',  ( -0.8083506638593009885, -0.5887012860850802110, 0.000000000000000000 ) ) ;
#4751 =( BOUNDED_CURVE ( )  B_SPLINE_CURVE ( 2, ( #20603, #17756, #9407, #29297, #26835, #864, #12435, #19449, #30628 ),
 .UNSPECIFIED., .F., .F. ) 
 B_SPLINE_CURVE_WITH_KNOTS ( ( 3, 2, 2, 2, 3 ),
 ( 0.8541666666666667407, 0.8611111111111111605, 0.8750000000000000000, 0.8888888888888888395, 0.8958333333333333703 ),
 .UNSPECIFIED. ) 
 CURVE ( )  GEOMETRIC_REPRESENTATION_ITEM ( )  RATIONAL_B_SPLINE_CURVE ( ( 0.9330127018922192983, 0.9330127018922198534, 1.000000000000000000, 0.8660254037844387076, 1.000000000000000000, 0.8660254037844387076, 1.000000000000000000, 0.9330127018922187432, 0.9330127018922192983 ) ) 
 REPRESENTATION_ITEM ( '' )  );
#4752 = CARTESIAN_POINT ( 'NONE',  ( -41.09002896937850124, 202.6965474657332038, 4.350049139982197666 ) ) ;
#4753 = CARTESIAN_POINT ( 'NONE',  ( 23.87821517812500005, 244.0468750006145058, 4.985214923628404016 ) ) ;
#4754 = CARTESIAN_POINT ( 'NONE',  ( 0.000000000000000000, 0.000000000000000000, 0.000000000000000000 ) ) ;
#4755 = CARTESIAN_POINT ( 'NONE',  ( 10.56230152254411081, 0.000000000000000000, -7.537499998771012955 ) ) ;
#4756 = CARTESIAN_POINT ( 'NONE',  ( -65.03794563604516554, 205.3262412349647832, 4.842901733360250205 ) ) ;
#4757 = CARTESIAN_POINT ( 'NONE',  ( 19.56230152254411792, -5.196152422706629359, -2.437499998771047949 ) ) ;
#4758 = ORIENTED_EDGE ( 'NONE', *, *, #19169, .T. ) ;
#4759 = DIRECTION ( 'NONE',  ( -0.000000000000000000, -1.000000000000000000, -0.000000000000000000 ) ) ;
#4760 = CARTESIAN_POINT ( 'NONE',  ( -5.770363421893818234, 124.8351862821014748, -14.38691631536207005 ) ) ;
#4761 = ADVANCED_FACE ( 'NONE', ( #23602 ), #3877, .F. ) ;
#4762 = DIRECTION ( 'NONE',  ( -1.659705900203722642E-32, 2.710505431213758127E-16, 1.000000000000000000 ) ) ;
#4763 = CARTESIAN_POINT ( 'NONE',  ( -2.311890736173176641, 5.522686282101451738, -12.53471296425194836 ) ) ;
#4764 = CARTESIAN_POINT ( 'NONE',  ( 16.56230152254411081, -6.928203230275514990, -8.887500000000020606 ) ) ;
#4765 = AXIS2_PLACEMENT_3D ( 'NONE', #507, #31982, #5827 ) ;
#4766 = ORIENTED_EDGE ( 'NONE', *, *, #18461, .F. ) ;
#4767 = CARTESIAN_POINT ( 'NONE',  ( 15.24356964374999990, 0.000000000000000000, -0.1968749993854768121 ) ) ;
#4768 = CARTESIAN_POINT ( 'NONE',  ( -9.465287035748065847, 77.39768628210144641, -2.064181346179273735 ) ) ;
#4769 = CARTESIAN_POINT ( 'NONE',  ( 16.56230152254410726, 0.000000000000000000, -10.00000000000000000 ) ) ;
#4770 = CARTESIAN_POINT ( 'NONE',  ( 3.796722387233182339, 123.2148137178985792, 8.710071997420207879 ) ) ;
#4771 = CARTESIAN_POINT ( 'NONE',  ( 27.24356964374999635, 195.5656250006145171, -15.72908226750539029 ) ) ;
#4772 = DIRECTION ( 'NONE',  ( 0.08715574274765150453, 0.000000000000000000, 0.9961946980917461003 ) ) ;
#4773 = CARTESIAN_POINT ( 'NONE',  ( 27.24356964375000345, 197.3843750006145399, -3.336375036156643733E-15 ) ) ;
#4774 = CARTESIAN_POINT ( 'NONE',  ( 10.89885883991209425, 194.9999999999999432, 24.98405147375524749 ) ) ;
#4775 = CARTESIAN_POINT ( 'NONE',  ( -69.00000000000002842, 206.0000000000000000, -2.499999999999998668 ) ) ;
#4776 = CARTESIAN_POINT ( 'NONE',  ( 7.954856959092311719, 56.22731371789854649, -5.529263428287300108 ) ) ;
#4777 = CYLINDRICAL_SURFACE ( 'NONE', #24854, 27.00000000000000000 ) ;
#4778 = VERTEX_POINT ( 'NONE', #12602 ) ;
#4779 = CARTESIAN_POINT ( 'NONE',  ( 23.99999999999999645, 241.8062500012290457, -5.196152422706631135 ) ) ;
#4780 = CARTESIAN_POINT ( 'NONE',  ( 8.715434833792128799, 55.93981371789855217, -8.962234695871567070 ) ) ;
#4781 = CARTESIAN_POINT ( 'NONE',  ( 10.31873187879411091, -3.604726614523244610, -7.359374999385524418 ) ) ;
#4782 = CARTESIAN_POINT ( 'NONE',  ( -13.62178482187500528, 199.2781250006145228, -23.59362340125807123 ) ) ;
#4783 = CARTESIAN_POINT ( 'NONE',  ( 15.24356964374999990, 0.000000000000000000, -6.103124999385478588 ) ) ;
#4784 = CARTESIAN_POINT ( 'NONE',  ( -8.715434833792127023, 32.93981371789854506, 8.962234695871568846 ) ) ;
#4785 = VERTEX_POINT ( 'NONE', #651 ) ;
#4786 = UNCERTAINTY_MEASURE_WITH_UNIT (LENGTH_MEASURE( 1.000000000000000082E-05 ), #19083, 'distance_accuracy_value', 'NONE');
#4787 = CARTESIAN_POINT ( 'NONE',  ( 16.56230152254411792, 7.209453229046482114, -2.109374999385531080 ) ) ;
#4788 = CARTESIAN_POINT ( 'NONE',  ( -8.962234695871760692, 11.56018628210145316, 8.715434833791933400 ) ) ;
#4789 = CARTESIAN_POINT ( 'NONE',  ( 31.39250523762275691, 7.209453229046482114, 168.7868784227583205 ) ) ;
#4790 = CARTESIAN_POINT ( 'NONE',  ( -59.49627896937850124, 203.4690446883607535, -1.626142955000504209 ) ) ;
#4791 = DIRECTION ( 'NONE',  ( 1.000000000000000000, 0.000000000000000000, -0.000000000000000000 ) ) ;
#4792 = CARTESIAN_POINT ( 'NONE',  ( 11.48171059495408208, 65.71481371789855075, -4.944772684328420986 ) ) ;
#4793 = CARTESIAN_POINT ( 'NONE',  ( -65.82961230271185116, 211.3212981617417938, 4.469044688360757966 ) ) ;
#4794 = CARTESIAN_POINT ( 'NONE',  ( -54.55580436395489841, 216.5000000000000000, 0.1155267958017343610 ) ) ;
#4795 = CARTESIAN_POINT ( 'NONE',  ( 15.00000000000031797, 3.464101615137936019, -6.787500000000000533 ) ) ;
#4796 = DIRECTION ( 'NONE',  ( 1.000000000000000000, 0.000000000000000000, 0.000000000000000000 ) ) ;
#4797 = CARTESIAN_POINT ( 'NONE',  ( -15.50000000000000533, 34.08981371789853654, 0.1745138560722471477 ) ) ;
#4798 = CARTESIAN_POINT ( 'NONE',  ( -30.60044563604516199, 203.6929966515019430, -6.137860380172892150 ) ) ;
#4799 = CARTESIAN_POINT ( 'NONE',  ( -12.53471296425194836, 30.82268628210144001, 2.311890736173176641 ) ) ;
#4800 = CARTESIAN_POINT ( 'NONE',  ( 26.99999999999999645, 7.347880794884117764E-16, -7.874999999999992895 ) ) ;
#4801 = CARTESIAN_POINT ( 'NONE',  ( -4.944772684328673229, 66.18518628210144072, 11.48171059495397728 ) ) ;
#4802 = CARTESIAN_POINT ( 'NONE',  ( 3.257655550457285720, 6.097686282101443922, -15.46528703574804986 ) ) ;
#4803 = CARTESIAN_POINT ( 'NONE',  ( 16.56230152254411436, 6.928203230275514990, -1.912500000000037836 ) ) ;
#4804 = CARTESIAN_POINT ( 'NONE',  ( -28.58889042833610361, 203.6434601642691007, -4.885801288223162508 ) ) ;
#4805 = ORIENTED_EDGE ( 'NONE', *, *, #9600, .T. ) ;
#4806 = CARTESIAN_POINT ( 'NONE',  ( 6.092822981423978490, 33.98518628210143788, -14.25334919248782306 ) ) ;
#4807 = LINE ( 'NONE', #25277, #10293 ) ;
#4808 = CARTESIAN_POINT ( 'NONE',  ( 5.778771075727756162E-15, 198.1718750006145342, 31.45816453501075927 ) ) ;
#4809 = DIRECTION ( 'NONE',  ( 0.000000000000000000, 0.000000000000000000, 1.000000000000000000 ) ) ;
#4810 = SURFACE_STYLE_USAGE ( .BOTH. , #22635 ) ;
#4811 = CARTESIAN_POINT ( 'NONE',  ( -13.49999999999998401, 195.1250000000000284, 23.38268590217985476 ) ) ;
#4812 = CARTESIAN_POINT ( 'NONE',  ( -7.228626920339069173, 11.27268628210143042, 10.49813415415989581 ) ) ;
#4813 = CARTESIAN_POINT ( 'NONE',  ( 26.75643035624999655, 248.2468750006145797, 3.323476615752267715 ) ) ;
#4814 = CARTESIAN_POINT ( 'NONE',  ( -1.715153634034442431, 105.6773137178985706, 9.534712964251900402 ) ) ;
#4815 = CARTESIAN_POINT ( 'NONE',  ( 15.24356964374999990, 243.1093750006145342, 0.000000000000000000 ) ) ;
#4816 = VERTEX_POINT ( 'NONE', #18493 ) ;
#4817 = CARTESIAN_POINT ( 'NONE',  ( 23.99999999999999645, 248.5562500012290457, -5.196152422706631135 ) ) ;
#4818 = CARTESIAN_POINT ( 'NONE',  ( 6.932735513424201024, 120.0523137178985706, -10.69584247140429412 ) ) ;
#4819 = CARTESIAN_POINT ( 'NONE',  ( 22.80587116629410716, 7.646167579472015790E-16, -9.815624999385569538 ) ) ;
#4820 = CARTESIAN_POINT ( 'NONE',  ( 24.55661210480496948, 3.604726614523236616, 162.2891901003200132 ) ) ;
#4821 = CARTESIAN_POINT ( 'NONE',  ( 18.12178482187500350, -4.985214923628407568, -0.6281249993854709501 ) ) ;
#4822 = CARTESIAN_POINT ( 'NONE',  ( -13.50000000000000533, 196.7750000000000057, -23.38268590217984411 ) ) ;
#4823 = ORIENTED_EDGE ( 'NONE', *, *, #34019, .F. ) ;
#4824 = CARTESIAN_POINT ( 'NONE',  ( 8.715434833791931624, 27.66018628210144215, 8.962234695871760692 ) ) ;
#4825 = ORIENTED_EDGE ( 'NONE', *, *, #7158, .F. ) ;
#4826 = ORIENTED_EDGE ( 'NONE', *, *, #19586, .T. ) ;
#4827 = CARTESIAN_POINT ( 'NONE',  ( 15.00000000000000000, 0.000000000000000000, -4.893749998770957177 ) ) ;
#4828 = CARTESIAN_POINT ( 'NONE',  ( 26.75643035624999655, 7.049594010296217766E-16, -0.8156249993854780556 ) ) ;
#4829 = CARTESIAN_POINT ( 'NONE',  ( 20.99999999999999645, -6.928203230275506996, -1.237499999999996270 ) ) ;
#4830 = CARTESIAN_POINT ( 'NONE',  ( 26.99999999999999645, 7.347880794884117764E-16, -6.074999999999997513 ) ) ;
#4831 = CARTESIAN_POINT ( 'NONE',  ( 15.24356964375000167, 249.3343750006145001, 3.323476615752272600 ) ) ;
#4832 = CARTESIAN_POINT ( 'NONE',  ( 11.61527771782819940, 81.13518628210145778, -4.622313124798573369 ) ) ;
#4833 = EDGE_CURVE ( 'NONE', #32427, #22420, #23128, .T. ) ;
#4834 = CARTESIAN_POINT ( 'NONE',  ( -6.092822981423666739, 8.214813717898532985, -14.25334919248795096 ) ) ;
#4835 = EDGE_CURVE ( 'NONE', #9824, #31631, #31140, .T. ) ;
#4836 = CARTESIAN_POINT ( 'NONE',  ( -61.07961230271182274, 211.8571965466040581, 6.469044688360755302 ) ) ;
#4837 = CARTESIAN_POINT ( 'NONE',  ( 14.59897497552647394, 216.4010250244744782, -0.7232488345312202416 ) ) ;
#4838 = CARTESIAN_POINT ( 'NONE',  ( -57.51711230271184405, 214.4690446883608104, -1.321298161741814914 ) ) ;
#4839 = CIRCLE ( 'NONE', #1811, 2.649999999999987477 ) ;
#4840 = CARTESIAN_POINT ( 'NONE',  ( 28.05502581071438328, -5.196152422706632912, 165.0604537508149008 ) ) ;
#4841 = CARTESIAN_POINT ( 'NONE',  ( 7.228626920338837358, 122.9273137178985422, 10.49813415416005036 ) ) ;
#4842 = CARTESIAN_POINT ( 'NONE',  ( -67.02455436395489130, 206.6211998817774997, 3.209657149897401585 ) ) ;
#4843 = CARTESIAN_POINT ( 'NONE',  ( -59.10788769728823411, 218.4690446883607535, 2.393094931466250408 ) ) ;
#4844 = ADVANCED_FACE ( 'NONE', ( #4067 ), #12787, .F. ) ;
#4845 = CARTESIAN_POINT ( 'NONE',  ( 20.99999999999999645, 6.646953231504538984, -2.615624999385474325 ) ) ;
#4846 = CARTESIAN_POINT ( 'NONE',  ( 27.24356964375000345, 196.4281250006145569, -3.336375036156643733E-15 ) ) ;
#4847 = CARTESIAN_POINT ( 'NONE',  ( 13.04141134922778988, 93.02731371789853654, -8.927990412390371944 ) ) ;
#4848 = CARTESIAN_POINT ( 'NONE',  ( -43.46502896937849414, 215.5714017266979567, -3.350049139982168800 ) ) ;
#4849 = ORIENTED_EDGE ( 'NONE', *, *, #5730, .F. ) ;
#4850 = CARTESIAN_POINT ( 'NONE',  ( -29.00000000000002487, 210.0000000000000000, 0.000000000000000000 ) ) ;
#4851 = CARTESIAN_POINT ( 'NONE',  ( 8.962234695871762469, 126.5601862821014691, -8.715434833791931624 ) ) ;
#4852 = CARTESIAN_POINT ( 'NONE',  ( 14.38691631536207538, 71.93518628210142651, -5.770363421893813793 ) ) ;
#4853 = LINE ( 'NONE', #31384, #28330 ) ;
#4854 = CARTESIAN_POINT ( 'NONE',  ( 24.75434669616370087, -3.604726614523244610, 164.5493068216156871 ) ) ;
#4855 = AXIS2_PLACEMENT_3D ( 'NONE', #18448, #29798, #30182 ) ;
#4856 = CARTESIAN_POINT ( 'NONE',  ( 13.23911966647218996, 90.04768628210145209, -8.632099005475504683 ) ) ;
#4857 = CARTESIAN_POINT ( 'NONE',  ( -53.36830436395489841, 209.8844732041982581, 6.500000000000000888 ) ) ;
#4858 = CARTESIAN_POINT ( 'NONE',  ( 16.56230152254411081, -7.209453229046475009, -5.428124999385503635 ) ) ;
#4859 = CARTESIAN_POINT ( 'NONE',  ( 8.843639120294328748, 44.33518628210144641, -3.474262827703334722 ) ) ;
#4860 = CYLINDRICAL_SURFACE ( 'NONE', #5541, 6.000000000000001776 ) ;
#4861 = CARTESIAN_POINT ( 'NONE',  ( -65.04538769728824832, 211.8571965466039444, -6.469044688360768625 ) ) ;
#4862 = CARTESIAN_POINT ( 'NONE',  ( 0.3500000000000030864, 244.5000000000000000, -5.000000000000001776 ) ) ;
#4863 = CARTESIAN_POINT ( 'NONE',  ( 12.46528703574805874, 54.39768628210146062, 2.660918448318279950 ) ) ;
#4864 = CARTESIAN_POINT ( 'NONE',  ( 26.99999999999999645, 198.4625000000000341, -15.58845726811990495 ) ) ;
#4865 = DIRECTION ( 'NONE',  ( 1.000000000000000000, 0.000000000000000000, 0.000000000000000000 ) ) ;
#4867 = CARTESIAN_POINT ( 'NONE',  ( 22.80587116629412492, -3.604726614523238837, -0.4593749993855362757 ) ) ;
#4866 = CARTESIAN_POINT ( 'NONE',  ( 8.152565276336714462, 25.64768628210144286, -5.233372021372432847 ) ) ;
#4868 = CARTESIAN_POINT ( 'NONE',  ( 27.00000000000000355, 198.5375000012290627, -3.306546357697854128E-15 ) ) ;
#4869 = VERTEX_POINT ( 'NONE', #15639 ) ;
#4870 = CARTESIAN_POINT ( 'NONE',  ( 15.00000000000000000, 0.000000000000000000, -2.250000000000001776 ) ) ;
#4871 = DIRECTION ( 'NONE',  ( 0.000000000000000000, -1.000000000000000000, 0.000000000000000000 ) ) ;
#4872 = AXIS2_PLACEMENT_3D ( 'NONE', #3531, #26647, #12247 ) ;
#4873 = CARTESIAN_POINT ( 'NONE',  ( 37.17435860658612512, 3.604726614523243278, 163.2368371151495694 ) ) ;
#4874 = CARTESIAN_POINT ( 'NONE',  ( 24.73633934067528983, 0.000000000000000000, 161.5488335588110544 ) ) ;
#4875 = CARTESIAN_POINT ( 'NONE',  ( 21.00000000000000000, 244.2624999999999886, 6.928203230275506996 ) ) ;
#4876 = CARTESIAN_POINT ( 'NONE',  ( 20.99999999999999289, 248.9874999999999829, -5.999999999999997335 ) ) ;
#4877 = CARTESIAN_POINT ( 'NONE',  ( 2.311890736173452865, 82.67731371789855643, -12.53471296425189152 ) ) ;
#4878 = CARTESIAN_POINT ( 'NONE',  ( 12.50000000000000355, 90.91018628210146346, 0.1745138560725507937 ) ) ;
#4879 = EDGE_LOOP ( 'NONE', ( #1046, #2449, #7578, #23453 ) ) ;
#4880 = ORIENTED_EDGE ( 'NONE', *, *, #33340, .T. ) ;
#4881 = CARTESIAN_POINT ( 'NONE',  ( 27.00000000000001066, 198.5000000012290400, 15.58845726811988897 ) ) ;
#4882 = CARTESIAN_POINT ( 'NONE',  ( 23.99999999999999645, 5.196152422706631135, -1.049999999999995381 ) ) ;
#4883 = CARTESIAN_POINT ( 'NONE',  ( 15.53471296425188797, 57.37731371789855928, 2.908627838312457747 ) ) ;
#4884 = CARTESIAN_POINT ( 'NONE',  ( 21.00000000000000000, -6.646953231504538984, -8.240624999385500971 ) ) ;
#4885 = CARTESIAN_POINT ( 'NONE',  ( 15.24356964374999990, 243.9718750006145456, -3.323476615752268604 ) ) ;
#4886 = CARTESIAN_POINT ( 'NONE',  ( -61.08705436395490551, 206.7903428501026042, -3.378800118222489157 ) ) ;
#4887 = CARTESIAN_POINT ( 'NONE',  ( 20.00041122355693801, 239.7848985277800864, -5.668978102276318154 ) ) ;
#4888 = CARTESIAN_POINT ( 'NONE',  ( -2.064181346179062349, 36.10231371789854649, -9.465287035748106703 ) ) ;
#4889 = CARTESIAN_POINT ( 'NONE',  ( 10.31873187879411091, -3.604726614523240613, -7.753124999385540228 ) ) ;
#4890 = CARTESIAN_POINT ( 'NONE',  ( 8.710071997420211432, 102.5148137178985621, -3.796722387233181895 ) ) ;
#4891 = CARTESIAN_POINT ( 'NONE',  ( -13.62178482187498396, 199.4843750006145626, 23.59362340125808188 ) ) ;
#4892 = CARTESIAN_POINT ( 'NONE',  ( -10.69584247140429412, 16.55231371789855999, -6.932735513424201024 ) ) ;
#4893 = CARTESIAN_POINT ( 'NONE',  ( -2.660918448318275509, 65.89768628210146062, 12.46528703574805874 ) ) ;
#4894 = CARTESIAN_POINT ( 'NONE',  ( 16.56230152254411081, 6.928203230275506996, -9.449999998771041021 ) ) ;
#4895 = FACE_OUTER_BOUND ( 'NONE', #21258, .T. ) ;
#4896 = CARTESIAN_POINT ( 'NONE',  ( 24.47817193633207822, 3.604726614523236616, 161.3926148720374556 ) ) ;
#4897 = CARTESIAN_POINT ( 'NONE',  ( 20.99999999999999645, 185.0294372515228645, 0.000000000000000000 ) ) ;
#4898 = CARTESIAN_POINT ( 'NONE',  ( 22.80587116629411781, -3.604726614523238837, -6.759374999385539873 ) ) ;
#4899 = CARTESIAN_POINT ( 'NONE',  ( -13.50000000000000533, 199.5875000012290457, -23.38268590217984411 ) ) ;
#4900 = CARTESIAN_POINT ( 'NONE',  ( 6.594114490232313663, 101.2601862821014436, 6.840914352312096547 ) ) ;
#4901 = CARTESIAN_POINT ( 'NONE',  ( 16.56230152254410726, 0.000000000000000000, 10.00000000000000000 ) ) ;
#4902 = CARTESIAN_POINT ( 'NONE',  ( 11.48171059495397728, 119.0851862821014606, 4.944772684328674117 ) ) ;
#4903 = CARTESIAN_POINT ( 'NONE',  ( -9.195083260712237916, 143.0000000000000000, 6.638546685473677655 ) ) ;
#4904 = CYLINDRICAL_SURFACE ( 'NONE', #4694, 3.999999999999996447 ) ;
#4906 = ORIENTED_EDGE ( 'NONE', *, *, #11723, .T. ) ;
#4905 = AXIS2_PLACEMENT_3D ( 'NONE', #10816, #16142, #10443 ) ;
#4907 = CARTESIAN_POINT ( 'NONE',  ( 37.33614145406145468, 3.604726614523238837, 165.0860235234823392 ) ) ;
#4908 = CARTESIAN_POINT ( 'NONE',  ( 26.75643035624999655, 7.049594010296217766E-16, -6.215624999385465976 ) ) ;
#4909 = CARTESIAN_POINT ( 'NONE',  ( -27.24356964374999279, 198.5468750006145342, 15.72908226750539384 ) ) ;
#4910 = DIRECTION ( 'NONE',  ( -0.000000000000000000, -0.000000000000000000, 1.000000000000000000 ) ) ;
#4911 = CARTESIAN_POINT ( 'NONE',  ( 25.32464060422194052, 0.000000000000000000, 168.2731477709303363 ) ) ;
#4912 = DIRECTION ( 'NONE',  ( 1.000000000000000000, 0.000000000000000000, 0.000000000000000000 ) ) ;
#4913 = CARTESIAN_POINT ( 'NONE',  ( 15.00000000000000000, 249.9625000000000057, -3.464101615137752166 ) ) ;
#4914 = LINE ( 'NONE', #5104, #2719 ) ;
#4915 = CARTESIAN_POINT ( 'NONE',  ( 8.715434833792128799, 138.7398137178985564, -8.962234695871567070 ) ) ;
#4916 = CARTESIAN_POINT ( 'NONE',  ( -7.228626920339070061, 140.0726862821014436, 10.49813415415989404 ) ) ;
#4918 = VERTEX_POINT ( 'NONE', #23984 ) ;
#4917 = ORIENTED_EDGE ( 'NONE', *, *, #414, .F. ) ;
#4919 = CARTESIAN_POINT ( 'NONE',  ( 21.00000000000000000, 245.1343750006145115, -6.646953231504538984 ) ) ;
#4920 = CARTESIAN_POINT ( 'NONE',  ( 10.49813415416005213, 10.22731371789853405, -7.228626920338837358 ) ) ;
#4921 = CARTESIAN_POINT ( 'NONE',  ( 15.24356964374999990, 0.000000000000000000, -4.190624999385467397 ) ) ;
#4922 = CARTESIAN_POINT ( 'NONE',  ( 8.632099005475788900, 120.0523137178985280, -13.23911966647199812 ) ) ;
#4923 = CARTESIAN_POINT ( 'NONE',  ( -29.50000000000000711, 252.0000000000000000, 5.000000000000000000 ) ) ;
#4924 = CARTESIAN_POINT ( 'NONE',  ( 15.24356964375000167, -3.323476615752272600, -0.6656249993855035685 ) ) ;
#4925 = CARTESIAN_POINT ( 'NONE',  ( 10.31873187879410736, 3.604726614523240613, -9.234374999385533300 ) ) ;
#4926 = VERTEX_POINT ( 'NONE', #24357 ) ;
#4927 = CARTESIAN_POINT ( 'NONE',  ( 27.24356964375000700, 195.0406250006145399, 15.72908226750537075 ) ) ;
#4928 = CARTESIAN_POINT ( 'NONE',  ( -12.46528703574805697, 114.1976862821014720, -2.660918448318280838 ) ) ;
#4929 = LINE ( 'NONE', #3856, #26261 ) ;
#4930 = CARTESIAN_POINT ( 'NONE',  ( -47.42336230271184405, 217.4189793300686233, 4.149950860017807663 ) ) ;
#4931 = CARTESIAN_POINT ( 'NONE',  ( 26.75643035624999655, 244.9843750006145342, 3.323476615752267271 ) ) ;
#4932 = FACE_OUTER_BOUND ( 'NONE', #16499, .T. ) ;
#4933 = CARTESIAN_POINT ( 'NONE',  ( -38.31919563604515844, 214.5000000000000284, -0.1155267958017627827 ) ) ;
#4934 = CARTESIAN_POINT ( 'NONE',  ( 10.49813415415989581, 119.3726862821014549, 7.228626920339068285 ) ) ;
#4935 = CARTESIAN_POINT ( 'NONE',  ( 22.56230152254410370, 7.347880794884117764E-16, -1.462499998771016330 ) ) ;
#4936 = CARTESIAN_POINT ( 'NONE',  ( -38.32663769728824121, 204.3130714775002730, 3.149950860017883603 ) ) ;
#4937 = CARTESIAN_POINT ( 'NONE',  ( -54.50000000000000711, 244.5000000000000000, -5.000000000000000000 ) ) ;
#4938 = CARTESIAN_POINT ( 'NONE',  ( 11.08355503943142750, 117.3601862821014663, -10.83675517735155225 ) ) ;
#4939 =( BOUNDED_CURVE ( )  B_SPLINE_CURVE ( 2, ( #7204, #19337, #7755, #18777, #7384, #35993, #13442 ),
 .UNSPECIFIED., .F., .F. ) 
 B_SPLINE_CURVE_WITH_KNOTS ( ( 3, 2, 2, 3 ),
 ( 0.1521739130434775489, 0.1594202898550718672, 0.1666666666666661856, 0.1739130434782605317 ),
 .UNSPECIFIED. ) 
 CURVE ( )  GEOMETRIC_REPRESENTATION_ITEM ( )  RATIONAL_B_SPLINE_CURVE ( ( 1.000000000000013545, 0.8660254037844254960, 1.000000000000000000, 0.8660254037844387076, 1.000000000000000000, 0.8660254037844448138, 0.9999999999999938938 ) ) 
 REPRESENTATION_ITEM ( '' )  );
#4940 = CARTESIAN_POINT ( 'NONE',  ( 1.255007937094097924E-14, 199.4375000000000284, -27.00000000000000000 ) ) ;
#4941 = CARTESIAN_POINT ( 'NONE',  ( 4.622313124798573369, 19.03518628210144925, 11.61527771782819940 ) ) ;
#4942 = EDGE_CURVE ( 'NONE', #14336, #33921, #9572, .T. ) ;
#4943 = CARTESIAN_POINT ( 'NONE',  ( 10.56230152254410903, 3.464101615137757051, -9.487500000000068212 ) ) ;
#4944 = ORIENTED_EDGE ( 'NONE', *, *, #22429, .F. ) ;
#4945 = CARTESIAN_POINT ( 'NONE',  ( 0.000000000000000000, 200.0000000000000000, 0.000000000000000000 ) ) ;
#4946 = CARTESIAN_POINT ( 'NONE',  ( 8.152565276336714462, 80.84768628210143504, -5.233372021372432847 ) ) ;
#4947 = VECTOR ( 'NONE', #1686, 1000.000000000000000 ) ;
#4948 = CARTESIAN_POINT ( 'NONE',  ( -2.064181346179062349, 128.1023137178985678, -9.465287035748106703 ) ) ;
#4949 = CARTESIAN_POINT ( 'NONE',  ( -27.24356964375000345, 196.2031250006145342, 0.000000000000000000 ) ) ;
#4950 = CARTESIAN_POINT ( 'NONE',  ( 20.99999999999999645, 185.0294372515228645, 5.999999999999999112 ) ) ;
#4951 = CARTESIAN_POINT ( 'NONE',  ( -27.24356964374999990, 198.4718750006145171, -15.72908226750537786 ) ) ;
#4952 = CARTESIAN_POINT ( 'NONE',  ( 22.56230152254410370, 0.000000000000000000, -10.00000000000000000 ) ) ;
#4953 = FACE_BOUND ( 'NONE', #35834, .T. ) ;
#4954 = EDGE_CURVE ( 'NONE', #3383, #37177, #27189, .T. ) ;
#4955 = CARTESIAN_POINT ( 'NONE',  ( 6.594114490232462877, 65.13981371789854791, -6.840914352311949109 ) ) ;
#4956 = FACE_OUTER_BOUND ( 'NONE', #26942, .T. ) ;
#4957 = ORIENTED_EDGE ( 'NONE', *, *, #728, .F. ) ;
#4958 = AXIS2_PLACEMENT_3D ( 'NONE', #3737, #3557, #15310 ) ;
#4959 = CARTESIAN_POINT ( 'NONE',  ( 18.00000000000000000, 241.4312500012290457, -5.196152422706630247 ) ) ;
#4960 = CARTESIAN_POINT ( 'NONE',  ( -12.50000000000000355, 70.88981371789856212, 0.1745138560722786503 ) ) ;
#4961 = CARTESIAN_POINT ( 'NONE',  ( 22.80587116629411426, -3.604726614523238837, -6.309374999385513050 ) ) ;
#4962 = CARTESIAN_POINT ( 'NONE',  ( -27.24356964374999990, 198.4156250006145399, -15.72908226750537786 ) ) ;
#4963 = CARTESIAN_POINT ( 'NONE',  ( 21.00000000000000000, 6.646953231504538984, -6.665624999385467930 ) ) ;
#4964 = CARTESIAN_POINT ( 'NONE',  ( 10.69584247140429589, 30.35231371789855359, 6.932735513424201024 ) ) ;
#4965 = EDGE_CURVE ( 'NONE', #23915, #23913, #20695, .T. ) ;
#4966 =( BOUNDED_CURVE ( )  B_SPLINE_CURVE ( 2, ( #30976, #5180, #7668, #7853, #10874, #28305, #2528 ),
 .UNSPECIFIED., .F., .F. ) 
 B_SPLINE_CURVE_WITH_KNOTS ( ( 3, 2, 2, 3 ),
 ( 0.8913043478260852526, 0.8985507246376795987, 0.9057971014492740558, 0.9130434782608682909 ),
 .UNSPECIFIED. ) 
 CURVE ( )  GEOMETRIC_REPRESENTATION_ITEM ( )  RATIONAL_B_SPLINE_CURVE ( ( 1.000000000000030864, 0.8660254037844079544, 1.000000000000000000, 0.8660254037844387076, 1.000000000000000000, 0.8660254037844612451, 0.9999999999999774625 ) ) 
 REPRESENTATION_ITEM ( '' )  );
#4967 = ORIENTED_EDGE ( 'NONE', *, *, #15688, .F. ) ;
#4968 = CARTESIAN_POINT ( 'NONE',  ( 19.68408634441911076, 5.407089921784862696, -1.696874999385505900 ) ) ;
#4969 = EDGE_CURVE ( 'NONE', #24301, #23005, #6540, .T. ) ;
#4970 = CARTESIAN_POINT ( 'NONE',  ( -74.35000000000002274, 210.0000000000000000, 5.000000000000000000 ) ) ;
#4971 = CARTESIAN_POINT ( 'NONE',  ( 28.32508817407707014, 5.407089921784862696, 169.5446048129269059 ) ) ;
#4972 = CARTESIAN_POINT ( 'NONE',  ( -46.63169563604516554, 210.1155267958017703, 6.500000000000000888 ) ) ;
#4973 = SURFACE_STYLE_FILL_AREA ( #36251 ) ;
#4974 = CARTESIAN_POINT ( 'NONE',  ( 19.56230152254411792, 5.196152422706637353, -9.600000000000052935 ) ) ;
#4975 = CARTESIAN_POINT ( 'NONE',  ( 2.660918448318002838, 59.10231371789854649, 12.46528703574811558 ) ) ;
#4976 = CARTESIAN_POINT ( 'NONE',  ( -65.03794563604515133, 206.7903428501025758, 3.378800118222471838 ) ) ;
#4977 = CARTESIAN_POINT ( 'NONE',  ( -52.37872103062156270, 203.4690446883607535, 1.626142955000567936 ) ) ;
#4978 = CARTESIAN_POINT ( 'NONE',  ( 13.49999999999999645, 195.9125000012290343, -23.38268590217984766 ) ) ;
#4979 = PLANE ( 'NONE',  #14973 ) ;
#4980 = CARTESIAN_POINT ( 'NONE',  ( 2.908627838312458636, 45.87731371789854506, -15.53471296425188442 ) ) ;
#4981 = CARTESIAN_POINT ( 'NONE',  ( -68.80580436395490551, 218.5000000000000000, 0.1155267958017064944 ) ) ;
#4982 = CARTESIAN_POINT ( 'NONE',  ( 11.61527771782819940, 35.13518628210143646, -4.622313124798573369 ) ) ;
#4983 = CARTESIAN_POINT ( 'NONE',  ( 4.944772684328679446, 70.78518628210144925, -11.48171059495397373 ) ) ;
#4984 = CARTESIAN_POINT ( 'NONE',  ( 13.04141134922759804, 18.17268628210144499, 8.927990412390657937 ) ) ;
#4985 = CARTESIAN_POINT ( 'NONE',  ( 22.56230152254412502, 7.347880794884125653E-16, -2.925000000000066436 ) ) ;
#4986 = FACE_OUTER_BOUND ( 'NONE', #33375, .T. ) ;
#4987 = ORIENTED_EDGE ( 'NONE', *, *, #28651, .F. ) ;
#4988 = CARTESIAN_POINT ( 'NONE',  ( 15.50000000000000533, 26.51018628210144001, 0.1745138560725827404 ) ) ;
#4989 = CARTESIAN_POINT ( 'NONE',  ( 5.778771075727756162E-15, 195.4156250006145399, 31.45816453501076637 ) ) ;
#4990 = EDGE_CURVE ( 'NONE', #13050, #3146, #7113, .T. ) ;
#4991 = CARTESIAN_POINT ( 'NONE',  ( 5.778771075727756162E-15, 199.0718750006145399, 31.45816453501075927 ) ) ;
#4992 = CARTESIAN_POINT ( 'NONE',  ( 24.85399959338462139, 0.000000000000000000, 162.8936964012349051 ) ) ;
#4993 = FACE_OUTER_BOUND ( 'NONE', #11077, .T. ) ;
#4994 = DIRECTION ( 'NONE',  ( 0.1155267958017759666, 0.9933043639548631010, -1.378486719154166141E-14 ) ) ;
#4995 = CARTESIAN_POINT ( 'NONE',  ( 15.00000000000000000, 247.7125000000000057, -3.464101615137752610 ) ) ;
#4996 = ADVANCED_FACE ( 'NONE', ( #21146 ), #18113, .F. ) ;
#4997 = CARTESIAN_POINT ( 'NONE',  ( 26.75643035624999655, 247.4218750006145058, -3.323476615752271712 ) ) ;
#4998 = CARTESIAN_POINT ( 'NONE',  ( -3.796722387233185003, 109.4148137178985536, -8.710071997420207879 ) ) ;
#4999 = CARTESIAN_POINT ( 'NONE',  ( 15.24356964374999990, 241.7218750006145456, -3.323476615752268604 ) ) ;
#5000 = ORIENTED_EDGE ( 'NONE', *, *, #14751, .F. ) ;
#5001 = FACE_OUTER_BOUND ( 'NONE', #5661, .T. ) ;
#5002 = CARTESIAN_POINT ( 'NONE',  ( 26.99999999999999289, 0.000000000000000000, -8.000000000000000000 ) ) ;
#5003 = CARTESIAN_POINT ( 'NONE',  ( 21.00000000000000000, 248.8187500012290627, 6.928203230275506996 ) ) ;
#5004 = CARTESIAN_POINT ( 'NONE',  ( 12.53471296425189330, 121.7773137178985792, 2.311890736173451533 ) ) ;
#5005 = EDGE_CURVE ( 'NONE', #21861, #11570, #10548, .T. ) ;
#5006 = CARTESIAN_POINT ( 'NONE',  ( 13.44051670066911441, -5.407089921784859143, -8.615624999385563143 ) ) ;
#5007 = CARTESIAN_POINT ( 'NONE',  ( 24.59583218904140978, 3.604726614523236616, 162.7374777144612779 ) ) ;
#5008 = CARTESIAN_POINT ( 'NONE',  ( 26.99999999999999645, 240.8687500012290457, -3.464101615137755275 ) ) ;
#5009 = CARTESIAN_POINT ( 'NONE',  ( -27.00000000000000355, 198.1625000000000227, -15.58845726811989429 ) ) ;
#5010 = AXIS2_PLACEMENT_3D ( 'NONE', #7498, #24558, #19074 ) ;
#5011 = ORIENTED_EDGE ( 'NONE', *, *, #586, .T. ) ;
#5012 = CARTESIAN_POINT ( 'NONE',  ( 8.715434833791931624, 36.86018628210144499, 8.962234695871760692 ) ) ;
#5013 = VERTEX_POINT ( 'NONE', #19056 ) ;
#5014 = ORIENTED_EDGE ( 'NONE', *, *, #24856, .T. ) ;
#5015 = CARTESIAN_POINT ( 'NONE',  ( 26.99999999999999645, 7.347880794884117764E-16, -5.568749998770966769 ) ) ;
#5016 = CARTESIAN_POINT ( 'NONE',  ( 18.12178482187500350, -4.985214923628407568, -2.315624999385479388 ) ) ;
#5017 = CARTESIAN_POINT ( 'NONE',  ( 22.56230152254534360, -3.464101615137050505, -4.312500000000021316 ) ) ;
#5018 = CARTESIAN_POINT ( 'NONE',  ( 24.82458453031440726, 0.000000000000000000, 162.5574806918533000 ) ) ;
#5019 = CARTESIAN_POINT ( 'NONE',  ( 23.87821517812499650, 248.2468750006145228, -4.985214923628404904 ) ) ;
#5020 = EDGE_CURVE ( 'NONE', #14391, #30675, #18090, .T. ) ;
#5021 = CARTESIAN_POINT ( 'NONE',  ( 0.1745138560725515708, 61.01018628210145067, -12.50000000000000355 ) ) ;
#5022 = CARTESIAN_POINT ( 'NONE',  ( -64.04836230271183695, 204.3130714775002446, -3.149950860017828091 ) ) ;
#5023 = CARTESIAN_POINT ( 'NONE',  ( 14.34881165084746613, 216.6511883491593835, 0.6450403596531998351 ) ) ;
#5024 = CARTESIAN_POINT ( 'NONE',  ( -41.88169563604517265, 210.1155267958017703, 4.499999999999996447 ) ) ;
#5025 = CARTESIAN_POINT ( 'NONE',  ( 10.56230152254410903, 7.347880794884117764E-16, -10.00000000000000000 ) ) ;
#5026 = CARTESIAN_POINT ( 'NONE',  ( 25.09585677961646866, 3.464101615137752166, 165.6581366896638485 ) ) ;
#5027 = CARTESIAN_POINT ( 'NONE',  ( 11.61527771782809637, 122.0648137178985735, 4.622313124798827388 ) ) ;
#5028 = CARTESIAN_POINT ( 'NONE',  ( -36.94122103062157692, 208.3738570449993404, -6.530955311639226935 ) ) ;
#5029 = AXIS2_PLACEMENT_3D ( 'NONE', #14926, #6766, #29888 ) ;
#5030 = CARTESIAN_POINT ( 'NONE',  ( -60.49330436395489130, 210.1155267958016850, -8.500000000000003553 ) ) ;
#5031 = CARTESIAN_POINT ( 'NONE',  ( 23.87821517812499650, 4.985214923628404904, -1.303124999385479876 ) ) ;
#5032 = CARTESIAN_POINT ( 'NONE',  ( -13.62178482187500528, 195.6781250006145569, -23.59362340125807123 ) ) ;
#5033 = CARTESIAN_POINT ( 'NONE',  ( -13.23911966647199812, 90.15231371789855075, -8.632099005475788900 ) ) ;
#5034 = CARTESIAN_POINT ( 'NONE',  ( -66.22544563604516554, 216.3070033484980854, 6.137860380172893926 ) ) ;
#5035 = ORIENTED_EDGE ( 'NONE', *, *, #3203, .T. ) ;
#5036 = CARTESIAN_POINT ( 'NONE',  ( 15.00000000000000000, 0.000000000000000000, -1.743749998770943721 ) ) ;
#5037 = CARTESIAN_POINT ( 'NONE',  ( 12.53471296425194836, 127.4226862821014663, -2.311890736173178418 ) ) ;
#5038 = CARTESIAN_POINT ( 'NONE',  ( -15.46528703574804986, 68.19768628210142936, -3.257655550457287497 ) ) ;
#5039 = CARTESIAN_POINT ( 'NONE',  ( 20.99999999999999645, 0.000000000000000000, 50.00000000000000000 ) ) ;
#5040 = CARTESIAN_POINT ( 'NONE',  ( 27.98518077736123288, -5.407089921784865361, 165.6594454903691087 ) ) ;
#5041 = CARTESIAN_POINT ( 'NONE',  ( 3.257655550457285720, 88.89768628210146062, -15.46528703574804986 ) ) ;
#5042 = CARTESIAN_POINT ( 'NONE',  ( -42.08705436395489841, 205.3262412349647548, -4.842901733360204908 ) ) ;
#5043 = EDGE_CURVE ( 'NONE', #32797, #21280, #5072, .T. ) ;
#5044 = CARTESIAN_POINT ( 'NONE',  ( 16.56230152254411081, -7.209453229046475009, -7.678124999385515181 ) ) ;
#5045 = CARTESIAN_POINT ( 'NONE',  ( -9.500000000000005329, 12.71018628210143753, -0.1745138560725176813 ) ) ;
#5046 = CARTESIAN_POINT ( 'NONE',  ( 20.99999999999997513, 246.2874999999999943, -5.999999999999999112 ) ) ;
#5047 = CARTESIAN_POINT ( 'NONE',  ( -66.03497103062157692, 204.4285982733020148, -3.350049139982115509 ) ) ;
#5048 = CARTESIAN_POINT ( 'NONE',  ( 10.49813415415989581, 64.17268628210143788, 7.228626920339068285 ) ) ;
#5049 = CARTESIAN_POINT ( 'NONE',  ( 13.49999999999999645, 198.9500000000000171, -23.38268590217984766 ) ) ;
#5050 = CARTESIAN_POINT ( 'NONE',  ( -4.694659320240884604E-14, 197.5250000012290172, 27.00000000000000000 ) ) ;
#5052 = CARTESIAN_POINT ( 'NONE',  ( 19.68408634441911431, -5.407089921784861808, -0.9468749993855329894 ) ) ;
#5051 = CARTESIAN_POINT ( 'NONE',  ( -6.594114490232312775, 32.26018628210145067, -6.840914352312096547 ) ) ;
#5053 = CARTESIAN_POINT ( 'NONE',  ( 23.87821517812500005, 247.7593750006145399, 4.985214923628404016 ) ) ;
#5054 = EDGE_LOOP ( 'NONE', ( #36895, #16077, #18935, #1891 ) ) ;
#5055 = CARTESIAN_POINT ( 'NONE',  ( 15.00000000000000000, 0.000000000000000000, -3.149999999999986144 ) ) ;
#5056 = COLOUR_RGB ( '',0.8941176470588234615, 0.8941176470588234615, 0.8941176470588234615 ) ;
#5057 = CARTESIAN_POINT ( 'NONE',  ( 26.66784417439646404, 1.063661697287894059, -7.999999999999996447 ) ) ;
#5058 = CARTESIAN_POINT ( 'NONE',  ( 30.70615376348499836, -7.209453229046482114, 160.9418451752858346 ) ) ;
#5059 = CARTESIAN_POINT ( 'NONE',  ( 19.68408634441911076, -5.407089921784855591, -1.340624999385559013 ) ) ;
#5060 = CARTESIAN_POINT ( 'NONE',  ( 25.18413345258806046, 3.604726614523236616, 169.4617919265805881 ) ) ;
#5061 = CARTESIAN_POINT ( 'NONE',  ( 18.00000000000000355, 243.7750000000000057, 5.196152422706632912 ) ) ;
#5062 = CARTESIAN_POINT ( 'NONE',  ( 29.50988163713361701, 5.988803496771938129, 159.3844543775923341 ) ) ;
#5063 = CIRCLE ( 'NONE', #33524, 9.999999999999994671 ) ;
#5064 = CARTESIAN_POINT ( 'NONE',  ( 12.50000000000000355, 81.71018628210144641, 0.1745138560725507937 ) ) ;
#5065 = ORIENTED_EDGE ( 'NONE', *, *, #32048, .T. ) ;
#5066 = ORIENTED_EDGE ( 'NONE', *, *, #29640, .T. ) ;
#5067 = CARTESIAN_POINT ( 'NONE',  ( -13.49999999999998401, 195.6875000012290400, 23.38268590217985476 ) ) ;
#5068 = CARTESIAN_POINT ( 'NONE',  ( 18.00000000000000000, 5.196152422706630247, -0.9750000000000036415 ) ) ;
#5069 = CARTESIAN_POINT ( 'NONE',  ( 6.092822981423662299, 49.61481371789856354, 14.25334919248795096 ) ) ;
#5070 = CARTESIAN_POINT ( 'NONE',  ( 15.24356964375000167, -3.323476615752272600, -10.11562499938547788 ) ) ;
#5071 = CARTESIAN_POINT ( 'NONE',  ( 15.24356964375000167, 242.6968750006145399, 3.323476615752272600 ) ) ;
#5072 = CIRCLE ( 'NONE', #4441, 28.99999999999999645 ) ;
#5073 = CARTESIAN_POINT ( 'NONE',  ( -53.96205436395491262, 213.2096571498974242, 3.378800118222489601 ) ) ;
#5074 = CARTESIAN_POINT ( 'NONE',  ( 20.99999999999999645, 6.928203230275506996, -6.356249998770953979 ) ) ;
#5075 = CARTESIAN_POINT ( 'NONE',  ( -3.796722387233185003, 45.01481371789854791, -8.710071997420207879 ) ) ;
#5076 = CARTESIAN_POINT ( 'NONE',  ( -66.62872103062152007, 203.4690446883607535, 1.626142955000567936 ) ) ;
#5077 = CARTESIAN_POINT ( 'NONE',  ( 5.233372021372610483, 101.6523137178985792, -8.152565276336593669 ) ) ;
#5078 = CARTESIAN_POINT ( 'NONE',  ( 27.24356964375000700, 199.1468750006145285, 15.72908226750537075 ) ) ;
#5079 = VECTOR ( 'NONE', #10139, 1000.000000000000000 ) ;
#5080 = CARTESIAN_POINT ( 'NONE',  ( 10.49813415416005213, 10.22731371789853227, -7.228626920338837358 ) ) ;
#5081 = B_SPLINE_CURVE_WITH_KNOTS ( 'NONE', 3,
 ( #24628, #4342, #7572, #18957 ),
 .UNSPECIFIED., .F., .F.,
 ( 4, 4 ),
 ( 0.000000000000000000, 1.000000000000000000 ),
 .UNSPECIFIED. ) ;
#5082 = ADVANCED_FACE ( 'NONE', ( #25279 ), #33436, .F. ) ;
#5083 = CARTESIAN_POINT ( 'NONE',  ( -2.311890736173176641, 69.92268628210146630, -12.53471296425194836 ) ) ;
#5084 = CARTESIAN_POINT ( 'NONE',  ( 22.56230152254411436, -3.464101615137751278, -7.349999998771018284 ) ) ;
#5085 = CARTESIAN_POINT ( 'NONE',  ( 20.99999999999997868, 245.1625000000000227, 5.999999999999999112 ) ) ;
#5086 = CARTESIAN_POINT ( 'NONE',  ( 27.55866236128991176, -5.407089921784859143, 160.7843176865825967 ) ) ;
#5087 = CARTESIAN_POINT ( 'NONE',  ( 22.80587116629412847, 3.604726614523243278, -9.834374999385516958 ) ) ;
#5088 = CARTESIAN_POINT ( 'NONE',  ( 22.80587116629411426, 3.604726614523243278, -7.584374999385505411 ) ) ;
#5089 = CARTESIAN_POINT ( 'NONE',  ( -27.00000000000000355, 195.6125000012290513, 0.000000000000000000 ) ) ;
#5090 = CARTESIAN_POINT ( 'NONE',  ( 6.840914352312096547, 71.36018628210143788, -6.594114490232313663 ) ) ;
#5091 = CYLINDRICAL_SURFACE ( 'NONE', #14055, 27.00000000000000355 ) ;
#5092 = EDGE_CURVE ( 'NONE', #13079, #24290, #35304, .T. ) ;
#5093 = CARTESIAN_POINT ( 'NONE',  ( 12.53471296425194836, 118.2226862821014635, -2.311890736173178418 ) ) ;
#5094 = DIRECTION ( 'NONE',  ( 0.000000000000000000, 0.000000000000000000, 1.000000000000000000 ) ) ;
#5095 = CARTESIAN_POINT ( 'NONE',  ( 22.60769515458672885, 248.5736538117967314, -5.999999999999998224 ) ) ;
#5096 = EDGE_LOOP ( 'NONE', ( #9638, #19365, #12138, #8583, #25132 ) ) ;
#5097 = CARTESIAN_POINT ( 'NONE',  ( 37.29038468911893034, -3.604726614523235284, 164.5630213069841830 ) ) ;
#5098 = CARTESIAN_POINT ( 'NONE',  ( 23.87821517812500005, -4.985214923628404016, -4.490624999385461891 ) ) ;
#5099 = CARTESIAN_POINT ( 'NONE',  ( -13.62178482187500528, 197.0843750006145285, -23.59362340125807123 ) ) ;
#5100 = CARTESIAN_POINT ( 'NONE',  ( 31.29445502703164550, -7.209453229046482114, 167.6661593874051164 ) ) ;
#5101 = CARTESIAN_POINT ( 'NONE',  ( 25.24293209539601435, 3.464101615137757051, 167.3392152414693328 ) ) ;
#5102 = CARTESIAN_POINT ( 'NONE',  ( -76.95115755716803108, 229.4913094451872553, 5.000000000000000000 ) ) ;
#5103 = CARTESIAN_POINT ( 'NONE',  ( 15.24356964374999990, 240.4093750006145456, 0.000000000000000000 ) ) ;
#5104 = CARTESIAN_POINT ( 'NONE',  ( 3.306546357697854128E-15, 200.0000000000000000, 27.00000000000000355 ) ) ;
#5105 = CARTESIAN_POINT ( 'NONE',  ( -4.622313124798826500, 133.5648137178985735, 11.61527771782809637 ) ) ;
#5106 = CARTESIAN_POINT ( 'NONE',  ( -27.24356964375000345, 195.7718750006145569, -15.72908226750537786 ) ) ;
#5108 = ORIENTED_EDGE ( 'NONE', *, *, #20736, .F. ) ;
#5107 = ORIENTED_EDGE ( 'NONE', *, *, #22482, .F. ) ;
#5109 = VECTOR ( 'NONE', #22448, 1000.000000000000000 ) ;
#5110 = CARTESIAN_POINT ( 'NONE',  ( 15.24356964374999990, 245.6593750006145171, -3.323476615752268604 ) ) ;
#5111 = CARTESIAN_POINT ( 'NONE',  ( -8.962234695871565293, 7.639813717898541690, -8.715434833792128799 ) ) ;
#5112 = CARTESIAN_POINT ( 'NONE',  ( 15.24356964374999990, 0.000000000000000000, -3.740624999385461003 ) ) ;
#5113 = CARTESIAN_POINT ( 'NONE',  ( 14.38691631536194393, 112.8648137178985564, 5.770363421894124656 ) ) ;
#5114 = CARTESIAN_POINT ( 'NONE',  ( 6.500000000000000888, 244.5000000000000000, -10.00000000000000000 ) ) ;
#5115 = CARTESIAN_POINT ( 'NONE',  ( 26.75643035624999655, 7.049594010296217766E-16, -0.9281249993854934210 ) ) ;
#5116 = CARTESIAN_POINT ( 'NONE',  ( 13.44051670066910731, 5.407089921784862696, -7.471874999385508254 ) ) ;
#5117 = CARTESIAN_POINT ( 'NONE',  ( -13.62178482187498396, 194.9281250006145569, 23.59362340125808188 ) ) ;
#5118 = CARTESIAN_POINT ( 'NONE',  ( 8.962234695871762469, 117.3601862821014521, -8.715434833791931624 ) ) ;
#5119 = CARTESIAN_POINT ( 'NONE',  ( 10.31873187879411091, -3.604726614523240613, -3.253124999385519356 ) ) ;
#5120 = CARTESIAN_POINT ( 'NONE',  ( -43.06919563604516554, 218.5000000000000000, -0.1155267958018185298 ) ) ;
#5121 = CARTESIAN_POINT ( 'NONE',  ( 26.75643035624999655, 244.1218750006145228, -7.049594010296217766E-16 ) ) ;
#5122 = CARTESIAN_POINT ( 'NONE',  ( 22.56230152254368804, -3.464101615137996415, -7.349999998771023613 ) ) ;
#5123 = CARTESIAN_POINT ( 'NONE',  ( -30.60044563604516199, 206.6211998817775566, -3.209657149897419348 ) ) ;
#5124 = CARTESIAN_POINT ( 'NONE',  ( 12.46528703574805874, 118.7976862821014663, 2.660918448318279950 ) ) ;
#5125 = CARTESIAN_POINT ( 'NONE',  ( 19.56230152254410370, 5.196152422706631135, -1.387499998770996834 ) ) ;
#5126 = CARTESIAN_POINT ( 'NONE',  ( -44.46205436395488420, 214.6737587650352168, 4.842901733360204908 ) ) ;
#5127 = DIRECTION ( 'NONE',  ( 1.000000000000000000, 0.000000000000000000, 0.000000000000000000 ) ) ;
#5128 = PLANE ( 'NONE',  #7526 ) ;
#5129 = CARTESIAN_POINT ( 'NONE',  ( -11.08355503943142573, 112.7601862821014720, 10.83675517735155402 ) ) ;
#5130 = CYLINDRICAL_SURFACE ( 'NONE', #13327, 6.000000000000001776 ) ;
#5131 = CARTESIAN_POINT ( 'NONE',  ( -4.944772684328673229, 10.98518628210143433, 11.48171059495397728 ) ) ;
#5132 = CARTESIAN_POINT ( 'NONE',  ( 15.52041721667876573, 5.908847357411728396, -9.999476446176704059 ) ) ;
#5133 = LINE ( 'NONE', #19755, #11840 ) ;
#5134 = ORIENTED_EDGE ( 'NONE', *, *, #8705, .F. ) ;
#5135 = CARTESIAN_POINT ( 'NONE',  ( 16.56230152254411792, -6.928203230275514990, -3.487500000000039346 ) ) ;
#5136 = CARTESIAN_POINT ( 'NONE',  ( -3.796722387233375073, 75.38518628210142936, 8.710071997420127943 ) ) ;
#5137 = DIRECTION ( 'NONE',  ( 0.000000000000000000, 0.000000000000000000, 1.000000000000000000 ) ) ;
#5138 = CARTESIAN_POINT ( 'NONE',  ( -27.24356964374999635, 196.2406250006145285, 15.72908226750539384 ) ) ;
#5139 = CARTESIAN_POINT ( 'NONE',  ( 20.99999999999995381, 242.5187500012290513, 5.999999999999998224 ) ) ;
#5140 = CARTESIAN_POINT ( 'NONE',  ( -27.24356964375000345, 198.9593750006145285, 0.000000000000000000 ) ) ;
#5141 = DIRECTION ( 'NONE',  ( 0.000000000000000000, 0.000000000000000000, 1.000000000000000000 ) ) ;
#5142 = CARTESIAN_POINT ( 'NONE',  ( 20.99999999999999645, 0.000000000000000000, -8.000000000000000000 ) ) ;
#5143 = CARTESIAN_POINT ( 'NONE',  ( 0.1745138560723095977, 50.18981371789855217, 9.500000000000005329 ) ) ;
#5144 = CARTESIAN_POINT ( 'NONE',  ( 18.00000000000000355, -5.196152422706632912, -9.825000000000001066 ) ) ;
#5145 = ORIENTED_EDGE ( 'NONE', *, *, #32855, .F. ) ;
#5146 = CARTESIAN_POINT ( 'NONE',  ( 23.99999999999999645, 242.7062500012290513, -5.196152422706631135 ) ) ;
#5147 = CARTESIAN_POINT ( 'NONE',  ( 2.660918448318003282, 59.10231371789854649, 12.46528703574811558 ) ) ;
#5148 = CARTESIAN_POINT ( 'NONE',  ( 10.31873187879410736, 0.000000000000000000, -5.146874999385541827 ) ) ;
#5149 = CARTESIAN_POINT ( 'NONE',  ( 18.12178482187500350, -4.985214923628407568, -6.478124999385492799 ) ) ;
#5150 = CARTESIAN_POINT ( 'NONE',  ( -7.228626920338836470, 26.32731371789854791, -10.49813415416005213 ) ) ;
#5151 = ORIENTED_EDGE ( 'NONE', *, *, #21319, .T. ) ;
#5152 = CARTESIAN_POINT ( 'NONE',  ( 13.44051670066911264, 5.407089921784862696, -2.521874999385525840 ) ) ;
#5153 = CARTESIAN_POINT ( 'NONE',  ( -13.50000000000000533, 199.9250000000000114, -23.38268590217984411 ) ) ;
#5154 = EDGE_CURVE ( 'NONE', #27666, #4551, #35006, .T. ) ;
#5155 = CARTESIAN_POINT ( 'NONE',  ( 25.10405911393864642, 0.000000000000000000, 168.5465380477087933 ) ) ;
#5156 = AXIS2_PLACEMENT_3D ( 'NONE', #20310, #31851, #28999 ) ;
#5157 = CARTESIAN_POINT ( 'NONE',  ( -40.29836230271182984, 204.3130714775002446, -3.149950860017828091 ) ) ;
#5158 = CARTESIAN_POINT ( 'NONE',  ( 33.65960319901864040, 5.196152422706631135, 160.2787869599868316 ) ) ;
#5159 = PRESENTATION_STYLE_ASSIGNMENT (( #36626 ) ) ;
#5160 = FACE_OUTER_BOUND ( 'NONE', #36474, .T. ) ;
#5161 = CARTESIAN_POINT ( 'NONE',  ( -36.34747103062156981, 212.3500491399821613, -3.839350919129076445 ) ) ;
#5162 =( BOUNDED_CURVE ( )  B_SPLINE_CURVE ( 2, ( #22040, #24870, #19017, #15983, #19572, #1927, #13311, #28083, #2115 ),
 .UNSPECIFIED., .F., .F. ) 
 B_SPLINE_CURVE_WITH_KNOTS ( ( 3, 2, 2, 2, 3 ),
 ( 0.7500000000000000000, 0.7536231884057971175, 0.7608695652173913526, 0.7681159420289854767, 0.7717391304347825942 ),
 .UNSPECIFIED. ) 
 CURVE ( )  GEOMETRIC_REPRESENTATION_ITEM ( )  RATIONAL_B_SPLINE_CURVE ( ( 0.9330127018922194093, 0.9330127018922194093, 1.000000000000000000, 0.8660254037844387076, 1.000000000000000000, 0.8660254037844387076, 1.000000000000000000, 0.9330127018922194093, 0.9330127018922194093 ) ) 
 REPRESENTATION_ITEM ( '' )  );
#5163 = CARTESIAN_POINT ( 'NONE',  ( -47.43080436395489841, 203.5000000000000000, -0.1155267958017335561 ) ) ;
#5164 = ORIENTED_EDGE ( 'NONE', *, *, #13324, .F. ) ;
#5165 = CARTESIAN_POINT ( 'NONE',  ( 0.000000000000000000, 200.0000000000000000, 0.000000000000000000 ) ) ;
#5166 = CARTESIAN_POINT ( 'NONE',  ( 20.99999999999999645, 202.0000000000000000, 0.000000000000000000 ) ) ;
#5167 = CARTESIAN_POINT ( 'NONE',  ( 13.23911966647199812, 39.55231371789854933, 8.632099005475788900 ) ) ;
#5168 = CARTESIAN_POINT ( 'NONE',  ( -36.53794563604517265, 203.8621396198271043, 6.307003348498029460 ) ) ;
#5169 = CARTESIAN_POINT ( 'NONE',  ( -11.48171059495397373, 4.085186282101443744, -4.944772684328680334 ) ) ;
#5170 = CARTESIAN_POINT ( 'NONE',  ( 12.53471296425194836, 72.22268628210143504, -2.311890736173178418 ) ) ;
#5171 = CARTESIAN_POINT ( 'NONE',  ( -10.83675517735155047, 13.86018628210145032, -11.08355503943142750 ) ) ;
#5172 = EDGE_CURVE ( 'NONE', #16919, #9886, #2150, .T. ) ;
#5173 = CARTESIAN_POINT ( 'NONE',  ( 22.56230152254411792, 7.347880794884125653E-16, -1.575000000000048583 ) ) ;
#5174 = CARTESIAN_POINT ( 'NONE',  ( 0.000000000000000000, 0.000000000000000000, -27.00000000000000355 ) ) ;
#5175 = ORIENTED_EDGE ( 'NONE', *, *, #15166, .T. ) ;
#5176 = CARTESIAN_POINT ( 'NONE',  ( -10.83675517735155047, 23.06018628210144783, -11.08355503943142750 ) ) ;
#5177 = CIRCLE ( 'NONE', #17289, 5.000000000000000000 ) ;
#5178 = CARTESIAN_POINT ( 'NONE',  ( -27.24356964374999279, 194.8906250006145342, 15.72908226750539384 ) ) ;
#5179 = CARTESIAN_POINT ( 'NONE',  ( -27.24356964374999990, 198.9218750006145626, -15.72908226750537786 ) ) ;
#5180 = CARTESIAN_POINT ( 'NONE',  ( 36.62857725106935192, -3.464101615137295642, 159.7931759234488140 ) ) ;
#5181 = DIRECTION ( 'NONE',  ( 1.000000000000000000, 0.000000000000000000, 0.000000000000000000 ) ) ;
#5182 = ADVANCED_FACE ( 'NONE', ( #36646 ), #27566, .T. ) ;
#5183 = CARTESIAN_POINT ( 'NONE',  ( 7.234628195640363302, 196.3799038117967086, -26.99999999999996803 ) ) ;
#5184 = VECTOR ( 'NONE', #20982, 1000.000000000000000 ) ;
#5185 =( BOUNDED_CURVE ( )  B_SPLINE_CURVE ( 2, ( #18949, #12869, #9465, #15722, #27272, #29930, #16098, #36167, #4523 ),
 .UNSPECIFIED., .F., .F. ) 
 B_SPLINE_CURVE_WITH_KNOTS ( ( 3, 2, 2, 2, 3 ),
 ( 0.3541666666666666852, 0.3611111111111111049, 0.3750000000000000000, 0.3888888888888888951, 0.3958333333333333703 ),
 .UNSPECIFIED. ) 
 CURVE ( )  GEOMETRIC_REPRESENTATION_ITEM ( )  RATIONAL_B_SPLINE_CURVE ( ( 0.9330127018922194093, 0.9330127018922196314, 1.000000000000000000, 0.8660254037844387076, 1.000000000000000000, 0.8660254037844387076, 1.000000000000000000, 0.9330127018922190762, 0.9330127018922194093 ) ) 
 REPRESENTATION_ITEM ( '' )  );
#5186 = CARTESIAN_POINT ( 'NONE',  ( 15.24356964374999990, 246.7093750006145569, 0.000000000000000000 ) ) ;
#5187 = CARTESIAN_POINT ( 'NONE',  ( -8.710071997420207879, 107.1148137178985564, 3.796722387233182339 ) ) ;
#5188 = CARTESIAN_POINT ( 'NONE',  ( 15.24356964375000167, 241.3468750006145171, 3.323476615752272600 ) ) ;
#5189 = ORIENTED_EDGE ( 'NONE', *, *, #35777, .T. ) ;
#5190 = CARTESIAN_POINT ( 'NONE',  ( -67.02455436395489130, 205.1570982666397356, 4.673758765035198159 ) ) ;
#5191 = CARTESIAN_POINT ( 'NONE',  ( 26.99999999999999289, 0.000000000000000000, -8.000000000000000000 ) ) ;
#5192 = CARTESIAN_POINT ( 'NONE',  ( -7.234628195640313564, 199.9075961894323541, -27.00000000000000355 ) ) ;
#5193 = CARTESIAN_POINT ( 'NONE',  ( 12.50000000000000355, 121.4898137178985564, -0.1745138560722771515 ) ) ;
#5194 = CARTESIAN_POINT ( 'NONE',  ( 22.80587116629411071, -3.604726614523235284, -9.853124999385531879 ) ) ;
#5195 = CARTESIAN_POINT ( 'NONE',  ( 24.67754069786733240, 0.000000000000000000, 163.6714102439223097 ) ) ;
#5196 = CARTESIAN_POINT ( 'NONE',  ( 20.99999999999999645, 0.000000000000000000, -8.000000000000000000 ) ) ;
#5197 = CARTESIAN_POINT ( 'NONE',  ( -27.00000000000000355, 195.0500000000000114, 0.000000000000000000 ) ) ;
#5198 = EDGE_LOOP ( 'NONE', ( #1983, #252, #12977, #1612 ) ) ;
#5199 = EDGE_LOOP ( 'NONE', ( #10198, #34656, #29786, #28896 ) ) ;
#5200 = ORIENTED_EDGE ( 'NONE', *, *, #1973, .T. ) ;
#5201 = CARTESIAN_POINT ( 'NONE',  ( 18.00000000000000355, -5.196152422706632912, -3.918749998770953979 ) ) ;
#5202 = CARTESIAN_POINT ( 'NONE',  ( 23.87821517812499650, 4.985214923628404904, -2.990624999385460558 ) ) ;
#5203 = FACE_OUTER_BOUND ( 'NONE', #11385, .T. ) ;
#5204 = CARTESIAN_POINT ( 'NONE',  ( 13.56230152254411614, -5.196152422706638241, -1.275000000000053868 ) ) ;
#5205 = DIRECTION ( 'NONE',  ( 0.000000000000000000, 0.000000000000000000, 1.000000000000000000 ) ) ;
#5206 = CARTESIAN_POINT ( 'NONE',  ( 4.622313124798573369, 65.03518628210144925, 11.61527771782819940 ) ) ;
#5207 = CARTESIAN_POINT ( 'NONE',  ( -58.30877896937849414, 211.6261429550004891, -6.530955311639245586 ) ) ;
#5208 = CARTESIAN_POINT ( 'NONE',  ( 15.20136072254643977, 225.4630380732105550, 1.553813268098316769 ) ) ;
#5209 = CARTESIAN_POINT ( 'NONE',  ( -43.46502896937849414, 213.8393509191290889, -2.350049139982142155 ) ) ;
#5210 = DIRECTION ( 'NONE',  ( -0.000000000000000000, 1.000000000000000000, -0.000000000000000000 ) ) ;
#5211 = CARTESIAN_POINT ( 'NONE',  ( 28.00273236506578201, 5.196152422706630247, 164.4627369319599097 ) ) ;
#5212 = CARTESIAN_POINT ( 'NONE',  ( -8.962234695871565293, 127.2398137178985564, -8.715434833792128799 ) ) ;
#5213 = CARTESIAN_POINT ( 'NONE',  ( -32.98288769728824121, 203.5309553116391612, -1.857196546604028775 ) ) ;
#5214 = CARTESIAN_POINT ( 'NONE',  ( -43.67038769728823411, 207.6069050685337913, 8.469044688360781947 ) ) ;
#5215 = PRESENTATION_LAYER_ASSIGNMENT (  '', '', ( #24602 ) ) ;
#5216 =( REPRESENTATION_RELATIONSHIP ('NONE','NONE', #4304, #201 ) REPRESENTATION_RELATIONSHIP_WITH_TRANSFORMATION ( #34030 )SHAPE_REPRESENTATION_RELATIONSHIP( ) );
#5217 = CARTESIAN_POINT ( 'NONE',  ( 20.99999999999999645, 6.646953231504538984, -3.065624999385470062 ) ) ;
#5218 = CARTESIAN_POINT ( 'NONE',  ( 13.62178482187501416, 196.8031250006145285, 23.59362340125806767 ) ) ;
#5219 = CARTESIAN_POINT ( 'NONE',  ( -10.83675517735179028, 97.33981371789856496, 11.08355503943118947 ) ) ;
#5220 = CARTESIAN_POINT ( 'NONE',  ( -33.56919563604517265, 216.5000000000000000, -0.1155267958017906493 ) ) ;
#5221 = ADVANCED_FACE ( 'NONE', ( #22263 ), #24905, .T. ) ;
#5222 = ORIENTED_EDGE ( 'NONE', *, *, #15718, .T. ) ;
#5223 = CARTESIAN_POINT ( 'NONE',  ( 27.93736555800505172, -5.196152422706632912, 163.7155909083910501 ) ) ;
#5224 = CARTESIAN_POINT ( 'NONE',  ( -6.932735513423968321, 124.5476862821014663, -10.69584247140445221 ) ) ;
#5225 = CARTESIAN_POINT ( 'NONE',  ( -11.08355503943142573, 57.56018628210145494, 10.83675517735155402 ) ) ;
#5226 = CARTESIAN_POINT ( 'NONE',  ( 15.02283181144952628, 7.347880794884122694E-16, 50.52293445648592751 ) ) ;
#5227 = CARTESIAN_POINT ( 'NONE',  ( 33.97620792891898134, -5.407089921784861808, 162.5002714581805492 ) ) ;
#5228 = CARTESIAN_POINT ( 'NONE',  ( 2.908627838312118019, 83.72268628210143504, 15.53471296425195369 ) ) ;
#5229 =( BOUNDED_CURVE ( )  B_SPLINE_CURVE ( 2, ( #5794, #12230, #35721, #18122, #6933, #35908, #3513 ),
 .UNSPECIFIED., .F., .F. ) 
 B_SPLINE_CURVE_WITH_KNOTS ( ( 3, 2, 2, 3 ),
 ( 0.3043478260869552088, 0.3115942028985494994, 0.3188405797101437900, 0.3260869565217381361 ),
 .UNSPECIFIED. ) 
 CURVE ( )  GEOMETRIC_REPRESENTATION_ITEM ( )  RATIONAL_B_SPLINE_CURVE ( ( 1.000000000000024647, 0.8660254037844140607, 1.000000000000000000, 0.8660254037844387076, 1.000000000000000000, 0.8660254037844571373, 0.9999999999999815703 ) ) 
 REPRESENTATION_ITEM ( '' )  );
#5230 = AXIS2_PLACEMENT_3D ( 'NONE', #5165, #5353, #37001 ) ;
#5231 = EDGE_CURVE ( 'NONE', #8744, #16385, #16578, .T. ) ;
#5232 = CARTESIAN_POINT ( 'NONE',  ( 10.31873187879411269, -3.604726614523240613, -5.503124999385529570 ) ) ;
#5233 = CARTESIAN_POINT ( 'NONE',  ( 3.474262827703335166, 19.03518628210144570, 8.843639120294326972 ) ) ;
#5234 = CARTESIAN_POINT ( 'NONE',  ( 30.69389748721466304, -6.928203230275506996, 160.8017552964788592 ) ) ;
#5235 = CARTESIAN_POINT ( 'NONE',  ( -67.02455436395489130, 205.1570982666397356, 4.673758765035198159 ) ) ;
#5236 = CARTESIAN_POINT ( 'NONE',  ( -4.944772684328673229, 56.98518628210144499, 11.48171059495397728 ) ) ;
#5237 = CARTESIAN_POINT ( 'NONE',  ( 27.00000000000000355, 197.9750000000000227, -3.306546357697854128E-15 ) ) ;
#5238 = CARTESIAN_POINT ( 'NONE',  ( 26.99999999999999645, 197.6750000012290229, -15.58845726811990495 ) ) ;
#5240 = CARTESIAN_POINT ( 'NONE',  ( 22.80587116629411781, 3.604726614523243278, -0.3843749993855423153 ) ) ;
#5239 = CARTESIAN_POINT ( 'NONE',  ( -1.715153634034234598, 33.12268628210143362, -9.534712964251941258 ) ) ;
#5241 = CARTESIAN_POINT ( 'NONE',  ( 15.24356964374999990, 248.5093750006145399, 0.000000000000000000 ) ) ;
#5242 = VERTEX_POINT ( 'NONE', #10496 ) ;
#5243 = CARTESIAN_POINT ( 'NONE',  ( 26.99999999999999645, -3.464101615137751278, -4.762500000000000178 ) ) ;
#5244 = CARTESIAN_POINT ( 'NONE',  ( 20.00000000000024869, -5.916079783099657874, -7.999999999999998224 ) ) ;
#5245 = CARTESIAN_POINT ( 'NONE',  ( 30.62771359501211066, -7.209453229046482114, 160.0452699470032485 ) ) ;
#5246 = CARTESIAN_POINT ( 'NONE',  ( 19.68408634441910721, 5.407089921784857367, -1.190624999385520022 ) ) ;
#5247 = CARTESIAN_POINT ( 'NONE',  ( 25.14818170870464797, 0.000000000000000000, 169.0508616136177409 ) ) ;
#5248 = CARTESIAN_POINT ( 'NONE',  ( 15.00000000000000000, 244.1124999999999829, -3.464101615137752166 ) ) ;
#5249 = CARTESIAN_POINT ( 'NONE',  ( 18.00000000000000000, 5.196152422706630247, -0.9187499987709513150 ) ) ;
#5250 = EDGE_CURVE ( 'NONE', #29663, #5512, #24613, .T. ) ;
#5251 = CARTESIAN_POINT ( 'NONE',  ( -7.228626920339070061, 84.87268628210145494, 10.49813415415989404 ) ) ;
#5252 = ORIENTED_EDGE ( 'NONE', *, *, #3926, .F. ) ;
#5253 = ORIENTED_EDGE ( 'NONE', *, *, #34950, .F. ) ;
#5254 = CARTESIAN_POINT ( 'NONE',  ( -27.00000000000000355, 194.7125000012290172, 0.000000000000000000 ) ) ;
#5255 = CARTESIAN_POINT ( 'NONE',  ( 0.000000000000000000, 200.0000000000000000, 0.000000000000000000 ) ) ;
#5256 = CARTESIAN_POINT ( 'NONE',  ( 11.08355503943118769, 30.63981371789855146, 10.83675517735179028 ) ) ;
#5257 = CARTESIAN_POINT ( 'NONE',  ( 18.12178482187500350, -4.985214923628407568, -7.828124999385482674 ) ) ;
#5258 = CARTESIAN_POINT ( 'NONE',  ( 26.75643035624999655, 241.9468750006145683, 3.323476615752267715 ) ) ;
#5259 = CARTESIAN_POINT ( 'NONE',  ( -42.28497103062156270, 206.1606490808709111, -2.350049139982163027 ) ) ;
#5260 = AXIS2_PLACEMENT_3D ( 'NONE', #22579, #31108, #36961 ) ;
#5261 = CYLINDRICAL_SURFACE ( 'NONE', #3436, 5.000000000000000888 ) ;
#5262 = EDGE_CURVE ( 'NONE', #21814, #456, #16018, .T. ) ;
#5263 = CARTESIAN_POINT ( 'NONE',  ( 37.05343001352376575, 7.646167579472024665E-16, 161.8546169715473013 ) ) ;
#5264 = CARTESIAN_POINT ( 'NONE',  ( 2.064181346179061460, 31.50231371789854862, 9.465287035748106703 ) ) ;
#5265 = CARTESIAN_POINT ( 'NONE',  ( -68.01413769728823411, 213.1499508600178672, 5.686928522499718142 ) ) ;
#5266 = CARTESIAN_POINT ( 'NONE',  ( 6.840914352311949109, 95.03981371789855359, 6.594114490232462877 ) ) ;
#5267 = CARTESIAN_POINT ( 'NONE',  ( 5.778771075727756162E-15, 197.7218750006145456, 31.45816453501075927 ) ) ;
#5268 = CARTESIAN_POINT ( 'NONE',  ( -5.770363421894122880, 142.7648137178985621, 14.38691631536194393 ) ) ;
#5269 = CARTESIAN_POINT ( 'NONE',  ( 2.660918448318279950, 70.49768628210145494, -12.46528703574805697 ) ) ;
#5270 = CARTESIAN_POINT ( 'NONE',  ( 19.56230152254411081, -5.196152422706629359, -10.08749999877103853 ) ) ;
#5271 = CARTESIAN_POINT ( 'NONE',  ( 24.00000000000000000, 245.1999999999999886, 5.196152422706629359 ) ) ;
#5272 = CARTESIAN_POINT ( 'NONE',  ( 30.78949644248743311, -7.209453229046475009, 161.8944563553360467 ) ) ;
#5273 = CARTESIAN_POINT ( 'NONE',  ( 25.21678537267883868, 0.000000000000000000, 167.0403568332661450 ) ) ;
#5274 = CARTESIAN_POINT ( 'NONE',  ( 22.80587116629411781, 3.604726614523243278, -5.334374999385495641 ) ) ;
#5275 = CYLINDRICAL_SURFACE ( 'NONE', #14283, 2.649999999999992806 ) ;
#5276 = CARTESIAN_POINT ( 'NONE',  ( -13.62178482187500528, 199.2781250006145228, -23.59362340125807123 ) ) ;
#5277 = CARTESIAN_POINT ( 'NONE',  ( 6.840914352312096547, 80.56018628210146915, -6.594114490232313663 ) ) ;
#5278 = CARTESIAN_POINT ( 'NONE',  ( 21.00000000000000355, 0.000000000000000000, 50.00000000000001421 ) ) ;
#5279 = CARTESIAN_POINT ( 'NONE',  ( -10.69584247140444866, 113.0476862821014663, 6.932735513423972762 ) ) ;
#5280 = CARTESIAN_POINT ( 'NONE',  ( 21.00000000000000000, 240.2687500012290513, 5.999999999999998224 ) ) ;
#5281 = EDGE_LOOP ( 'NONE', ( #11172, #31588, #18795, #2024 ) ) ;
#5282 = CARTESIAN_POINT ( 'NONE',  ( 33.94189035521207387, -5.407089921784855591, 162.1080197958069107 ) ) ;
#5283 = CARTESIAN_POINT ( 'NONE',  ( 26.75643035624999655, -3.323476615752267715, -4.453124999385455141 ) ) ;
#5284 = CARTESIAN_POINT ( 'NONE',  ( 5.778771075727756162E-15, 196.3718750006145513, 31.45816453501076637 ) ) ;
#5285 = CARTESIAN_POINT ( 'NONE',  ( 25.02888728581879718, -3.604726614523244610, 167.6873201206046247 ) ) ;
#5286 = CARTESIAN_POINT ( 'NONE',  ( 31.21356360324042356, 6.928203230275514990, 166.7415661826265421 ) ) ;
#5287 = CARTESIAN_POINT ( 'NONE',  ( 20.99999999999999645, 6.928203230275506996, -0.1124999999999909128 ) ) ;
#5288 = CARTESIAN_POINT ( 'NONE',  ( 15.24356964374999990, 240.8218750006145399, -3.323476615752268604 ) ) ;
#5289 = CARTESIAN_POINT ( 'NONE',  ( -1.926257025242585782E-15, 199.2406250006145285, -31.45816453501076637 ) ) ;
#5290 = CARTESIAN_POINT ( 'NONE',  ( -10.69584247140429412, 117.7523137178986019, -6.932735513424201024 ) ) ;
#5291 = CARTESIAN_POINT ( 'NONE',  ( 12.53471296425194659, 136.6226862821014834, -2.311890736173178418 ) ) ;
#5293 = ORIENTED_EDGE ( 'NONE', *, *, #27550, .F. ) ;
#5292 = ORIENTED_EDGE ( 'NONE', *, *, #29381, .T. ) ;
#5294 = CARTESIAN_POINT ( 'NONE',  ( 21.00000000000000000, 244.2343750006145626, -6.646953231504538984 ) ) ;
#5295 = CARTESIAN_POINT ( 'NONE',  ( 15.00000000000000355, 7.347880794884112834E-16, -8.000000000000000000 ) ) ;
#5296 = EDGE_CURVE ( 'NONE', #23197, #10569, #26255, .T. ) ;
#5297 = CARTESIAN_POINT ( 'NONE',  ( -15.53471296425188442, 107.9773137178985394, -2.908627838312459080 ) ) ;
#5298 = EDGE_CURVE ( 'NONE', #29410, #26583, #5658, .T. ) ;
#5299 = CARTESIAN_POINT ( 'NONE',  ( 15.00000000000000000, 0.000000000000000000, -3.093749998770961795 ) ) ;
#5300 = CARTESIAN_POINT ( 'NONE',  ( 23.87821517812499650, 4.985214923628404904, -2.203124999385491556 ) ) ;
#5301 = CARTESIAN_POINT ( 'NONE',  ( 10.31873187879410558, 0.000000000000000000, -8.746874999385534366 ) ) ;
#5302 = PRODUCT_DEFINITION_SHAPE ( 'NONE', 'NONE',  #37513 ) ;
#5303 = CARTESIAN_POINT ( 'NONE',  ( 13.49999999999999645, 198.6125000012290513, -23.38268590217984766 ) ) ;
#5304 = EDGE_CURVE ( 'NONE', #28188, #17354, #1573, .T. ) ;
#5305 = CARTESIAN_POINT ( 'NONE',  ( -12.46528703574805697, 104.9976862821014691, -2.660918448318280838 ) ) ;
#5306 = CARTESIAN_POINT ( 'NONE',  ( 13.44051670066911441, 5.407089921784856479, -2.465624999385545912 ) ) ;
#5307 = EDGE_CURVE ( 'NONE', #18752, #33087, #9111, .T. ) ;
#5308 = CARTESIAN_POINT ( 'NONE',  ( -44.85044563604516554, 203.6929966515019430, -6.137860380172892150 ) ) ;
#5309 = CARTESIAN_POINT ( 'NONE',  ( 26.75643035624999655, 245.4343750006145228, 3.323476615752267271 ) ) ;
#5310 = CARTESIAN_POINT ( 'NONE',  ( -36.73586230271183695, 207.8500491399821613, 3.954877714930852495 ) ) ;
#5311 = CARTESIAN_POINT ( 'NONE',  ( 10.69584247140445221, 117.6476862821014464, -6.932735513423970097 ) ) ;
#5312 = CARTESIAN_POINT ( 'NONE',  ( 16.56230152254411081, 6.928203230275506996, -3.149999998770972365 ) ) ;
#5313 = CARTESIAN_POINT ( 'NONE',  ( -47.62872103062154849, 203.4690446883607535, 1.626142955000567936 ) ) ;
#5314 = FACE_OUTER_BOUND ( 'NONE', #26570, .T. ) ;
#5315 = LINE ( 'NONE', #16892, #20213 ) ;
#5316 = AXIS2_PLACEMENT_3D ( 'NONE', #7585, #4354, #7957 ) ;
#5317 = CARTESIAN_POINT ( 'NONE',  ( 15.50000000000000533, 109.3101862821014549, 0.1745138560725827404 ) ) ;
#5318 = CARTESIAN_POINT ( 'NONE',  ( 7.228626920339069173, 15.87268628210144961, -10.49813415415989404 ) ) ;
#5319 = CARTESIAN_POINT ( 'NONE',  ( 10.56230152254410903, 0.000000000000000000, -1.687499998771019305 ) ) ;
#5320 = CARTESIAN_POINT ( 'NONE',  ( 9.500000000000005329, 136.9101862821014777, 0.1745138560725188748 ) ) ;
#5321 = CARTESIAN_POINT ( 'NONE',  ( 10.31873187879410558, 3.604726614523236616, -2.878124999385517135 ) ) ;
#5322 = CARTESIAN_POINT ( 'NONE',  ( 24.81477950914817754, 0.000000000000000000, 162.4454087870936121 ) ) ;
#5323 = EDGE_LOOP ( 'NONE', ( #14755, #30529, #11955, #14828 ) ) ;
#5324 = CARTESIAN_POINT ( 'NONE',  ( 28.32999068460662428, 5.407089921784856479, 169.6006407646945604 ) ) ;
#5325 = CARTESIAN_POINT ( 'NONE',  ( -5.529263428287477744, 66.47268628210146346, 7.954856959092191815 ) ) ;
#5326 = CARTESIAN_POINT ( 'NONE',  ( -4.500000000000002665, 244.5000000000000000, -2.500000000000000000 ) ) ;
#5327 = CARTESIAN_POINT ( 'NONE',  ( -13.62178482187498396, 195.3781250006145171, 23.59362340125808188 ) ) ;
#5328 = LINE ( 'NONE', #11204, #35424 ) ;
#5329 = CARTESIAN_POINT ( 'NONE',  ( 27.24356964375000345, 196.0343750006145456, -3.336375036156643733E-15 ) ) ;
#5330 = CARTESIAN_POINT ( 'NONE',  ( 20.99999999999997868, 210.0000000000000000, 0.000000000000000000 ) ) ;
#5331 = CARTESIAN_POINT ( 'NONE',  ( 3.474262827703532341, 55.36481371789856354, -8.843639120294245259 ) ) ;
#5332 = CARTESIAN_POINT ( 'NONE',  ( 24.00000000000000000, -5.196152422706629359, -9.300000000000002487 ) ) ;
#5333 = AXIS2_PLACEMENT_3D ( 'NONE', #14690, #14323, #32305 ) ;
#5334 = EDGE_LOOP ( 'NONE', ( #13000, #35007, #20837, #34063 ) ) ;
#5335 = CARTESIAN_POINT ( 'NONE',  ( 23.99999999999999645, 242.2562500012290627, -5.196152422706631135 ) ) ;
#5336 = CARTESIAN_POINT ( 'NONE',  ( -12.50000000000000355, 61.68981371789855928, 0.1745138560722786503 ) ) ;
#5337 = CARTESIAN_POINT ( 'NONE',  ( 16.56230152254411436, -7.209453229046482114, -7.284374999385498484 ) ) ;
#5338 = CARTESIAN_POINT ( 'NONE',  ( 26.75643035624999655, 7.049594010296217766E-16, -5.878124999385475391 ) ) ;
#5339 = CARTESIAN_POINT ( 'NONE',  ( -12.53471296425189152, 34.37731371789855217, -2.311890736173453753 ) ) ;
#5340 = EDGE_LOOP ( 'NONE', ( #9591, #12794, #30107, #31044 ) ) ;
#5341 = AXIS2_PLACEMENT_3D ( 'NONE', #11867, #26088, #19687 ) ;
#5342 = CARTESIAN_POINT ( 'NONE',  ( 22.80587116629411781, -3.604726614523238837, -0.9093749993854999270 ) ) ;
#5343 = CARTESIAN_POINT ( 'NONE',  ( -2.311890736173176641, 5.522686282101451738, -12.53471296425194836 ) ) ;
#5344 = CARTESIAN_POINT ( 'NONE',  ( -30.00669563604516910, 209.8844732041982013, -6.500000000000000888 ) ) ;
#5345 = CARTESIAN_POINT ( 'NONE',  ( -40.49627896937849414, 203.4690446883607535, -1.626142955000504209 ) ) ;
#5346 = CARTESIAN_POINT ( 'NONE',  ( -47.00000000000000711, 244.5000000000000000, 5.000000000000000000 ) ) ;
#5347 = SURFACE_SIDE_STYLE ('',( #31319 ) ) ;
#5348 = CARTESIAN_POINT ( 'NONE',  ( -77.35272773637332477, 226.7246823105297153, -0.4999999999999908962 ) ) ;
#5349 = CARTESIAN_POINT ( 'NONE',  ( -36.54538769728824121, 211.3212981617418222, -4.469044688360751749 ) ) ;
#5350 = CARTESIAN_POINT ( 'NONE',  ( -46.04538769728823411, 211.8571965466039444, -6.469044688360768625 ) ) ;
#5351 = ORIENTED_EDGE ( 'NONE', *, *, #19209, .T. ) ;
#5352 = CIRCLE ( 'NONE', #18095, 7.500000000000000000 ) ;
#5353 = DIRECTION ( 'NONE',  ( -0.000000000000000000, -1.000000000000000000, -0.000000000000000000 ) ) ;
#5354 = CARTESIAN_POINT ( 'NONE',  ( 15.53471296425188797, 20.57731371789854435, 2.908627838312457747 ) ) ;
#5355 = CARTESIAN_POINT ( 'NONE',  ( -31.39211230271183339, 201.5309553116392181, 2.393094931466368980 ) ) ;
#5356 = CARTESIAN_POINT ( 'NONE',  ( 11.48171059495397728, 17.88518628210143646, 4.944772684328674117 ) ) ;
#5357 = CARTESIAN_POINT ( 'NONE',  ( 12.46528703574805874, 45.19768628210143646, 2.660918448318279950 ) ) ;
#5358 = CARTESIAN_POINT ( 'NONE',  ( 10.56230152254410193, 3.464101615137757051, -3.187499999999998668 ) ) ;
#5359 = LINE ( 'NONE', #20866, #4054 ) ;
#5360 = ORIENTED_EDGE ( 'NONE', *, *, #26558, .T. ) ;
#5361 = CARTESIAN_POINT ( 'NONE',  ( 15.46528703574804986, 8.397686282101439303, 3.257655550457285720 ) ) ;
#5362 = CARTESIAN_POINT ( 'NONE',  ( 13.62178482187501416, 195.9031250006145513, 23.59362340125806767 ) ) ;
#5363 = CARTESIAN_POINT ( 'NONE',  ( 27.24356964374999635, 199.2218750006145456, -15.72908226750539029 ) ) ;
#5364 = CYLINDRICAL_SURFACE ( 'NONE', #36533, 5.999999999999994671 ) ;
#5365 = PLANE ( 'NONE',  #35980 ) ;
#5366 = CARTESIAN_POINT ( 'NONE',  ( 19.39230484541326049, 240.0638461906613941, -5.999999999999997335 ) ) ;
#5367 = CARTESIAN_POINT ( 'NONE',  ( 23.87821517812500005, 247.3093750006145228, 4.985214923628404016 ) ) ;
#5368 = CARTESIAN_POINT ( 'NONE',  ( -0.1745138560723084320, 109.9898137178985706, -9.500000000000005329 ) ) ;
#5369 = CARTESIAN_POINT ( 'NONE',  ( 20.99999999999999645, 241.8718750006145228, 6.646953231504538984 ) ) ;
#5370 = ORIENTED_EDGE ( 'NONE', *, *, #5769, .F. ) ;
#5371 = CARTESIAN_POINT ( 'NONE',  ( -66.43080436395490551, 203.5000000000000000, -0.1155267958017335561 ) ) ;
#5372 = DIRECTION ( 'NONE',  ( 0.000000000000000000, 0.000000000000000000, 1.000000000000000000 ) ) ;
#5373 = CARTESIAN_POINT ( 'NONE',  ( 26.99999999999999645, 248.9687500012290116, -3.464101615137755275 ) ) ;
#5374 = CARTESIAN_POINT ( 'NONE',  ( -8.715434833792127023, 124.9398137178985593, 8.962234695871568846 ) ) ;
#5375 = CARTESIAN_POINT ( 'NONE',  ( 16.56230152254411436, 7.209453229046482114, -0.3093749993854842950 ) ) ;
#5376 = CARTESIAN_POINT ( 'NONE',  ( 27.66324925258708589, 5.407089921784856479, 161.9797513242927209 ) ) ;
#5377 = CARTESIAN_POINT ( 'NONE',  ( 13.49999999999999645, 195.8000000000000114, -23.38268590217984766 ) ) ;
#5378 = ORIENTED_EDGE ( 'NONE', *, *, #33334, .F. ) ;
#5379 = ORIENTED_EDGE ( 'NONE', *, *, #31383, .T. ) ;
#5380 = ORIENTED_EDGE ( 'NONE', *, *, #8349, .T. ) ;
#5381 = CARTESIAN_POINT ( 'NONE',  ( 26.99999999999999645, 7.347880794884117764E-16, -4.668749998770954868 ) ) ;
#5382 = CARTESIAN_POINT ( 'NONE',  ( 18.12178482187500350, -4.985214923628407568, -3.665624999385469707 ) ) ;
#5383 = CARTESIAN_POINT ( 'NONE',  ( 15.00000000000000000, 3.464101615137752610, -6.337500000000001243 ) ) ;
#5384 = CARTESIAN_POINT ( 'NONE',  ( 15.00000000000000355, 7.347880794884112834E-16, 50.26196565745150480 ) ) ;
#5385 = CARTESIAN_POINT ( 'NONE',  ( 15.24356964374999990, 248.3593750006145342, -3.323476615752268604 ) ) ;
#5386 = CARTESIAN_POINT ( 'NONE',  ( -10.49813415415989581, 50.37268628210145494, -7.228626920339068285 ) ) ;
#5387 =( BOUNDED_CURVE ( )  B_SPLINE_CURVE ( 2, ( #5809, #11504, #14724, #122, #20422, #29493, #6187 ),
 .UNSPECIFIED., .F., .F. ) 
 B_SPLINE_CURVE_WITH_KNOTS ( ( 3, 2, 2, 3 ),
 ( 0.4565217391304337569, 0.4637681159420281030, 0.4710144927536223936, 0.4782608695652167397 ),
 .UNSPECIFIED. ) 
 CURVE ( )  GEOMETRIC_REPRESENTATION_ITEM ( )  RATIONAL_B_SPLINE_CURVE ( ( 1.000000000000018430, 0.8660254037844202779, 1.000000000000000000, 0.8660254037844387076, 1.000000000000000000, 0.8660254037844510311, 0.9999999999999876765 ) ) 
 REPRESENTATION_ITEM ( '' )  );
#5388 = CARTESIAN_POINT ( 'NONE',  ( -65.23586230271183695, 206.8500491399821328, 5.686928522499748340 ) ) ;
#5389 = CARTESIAN_POINT ( 'NONE',  ( 14.68278727570621633, 216.3172127243001910, 0.6964482669446712126 ) ) ;
#5390 = CARTESIAN_POINT ( 'NONE',  ( -39.11086230271183695, 212.1499508600178387, -3.954877714930852495 ) ) ;
#5391 = CARTESIAN_POINT ( 'NONE',  ( 34.05180404138307182, 5.196152422706631135, 164.7616631013996766 ) ) ;
#5392 = CARTESIAN_POINT ( 'NONE',  ( -7.228626920338836470, 99.92731371789855643, -10.49813415416005213 ) ) ;
#5393 = CARTESIAN_POINT ( 'NONE',  ( -68.21205436395490551, 213.2096571498974242, 3.378800118222489601 ) ) ;
#5394 = CARTESIAN_POINT ( 'NONE',  ( -50.39955436395490551, 216.3070033484980002, -6.137860380172975638 ) ) ;
#5395 = CARTESIAN_POINT ( 'NONE',  ( 20.99999999999999645, -6.646953231504538984, -4.640624999385471128 ) ) ;
#5396 = CARTESIAN_POINT ( 'NONE',  ( 15.00000000000017408, -3.464101615137856083, -1.762499999999983968 ) ) ;
#5397 = CARTESIAN_POINT ( 'NONE',  ( -0.1745138560722442889, 91.58981371789856496, -15.50000000000000533 ) ) ;
#5398 = CARTESIAN_POINT ( 'NONE',  ( -32.97544563604516554, 214.8429017333602360, 4.673758765035156415 ) ) ;
#5399 = ORIENTED_EDGE ( 'NONE', *, *, #16506, .T. ) ;
#5400 = CARTESIAN_POINT ( 'NONE',  ( 21.00000000000000000, 242.0687500012289775, 5.999999999999998224 ) ) ;
#5401 = CARTESIAN_POINT ( 'NONE',  ( 2.311890736173175753, 111.3226862821014720, 12.53471296425194836 ) ) ;
#5402 = CARTESIAN_POINT ( 'NONE',  ( -5.770363421893818234, 69.63518628210144357, -14.38691631536207005 ) ) ;
#5403 = CYLINDRICAL_SURFACE ( 'NONE', #33800, 5.999999999999998224 ) ;
#5404 =( BOUNDED_SURFACE ( )  B_SPLINE_SURFACE ( 1, 2, ( 
 ( #4034, #27162, #27723, #19023, #30580, #4596, #16173, #1185, #12759, #1753, #18267, #29811, #31816, #28090, #4782, #19214, #25949, #14579, #29151, #26131, #7823, #34658, #14392, #2122, #13699, #3192, #3009, #14768, #20465, #5852, #10469, #16356, #25250, #13503, #163, #36426, #30760, #4962, #22047, #27904, #22234, #1935, #33598, #10655, #34848, #11362, #20088, #25061, #36800, #36614, #8703, #22933, #33785, #32005, #17430, #8886, #19400, #31632, #34478, #5662, #8521, #17242, #30944, #20277, #7637, #6035, #37492, #16544, #28784, #2821, #11543, #11729, #23115, #28969, #23301, #17622, #23482, #6606, #21029, #35402, #6793, #4139, #26313, #718, #14953, #35034, #29916, #9452, #9079, #23672, #15522, #35783, #6997, #9266, #32943, #9825, #26882, #913, #30108, #12482, #35217, #20838, #21403, #24237, #24050, #32381, #29722, #9640, #27076, #26501, #12291, #29536, #26689, #3576, #12098, #32195, #6229, #1102, #18368, #17803, #12670, #6419, #32565, #15136, #11915, #20649, #23863, #350, #531, #29345, #17992, #18567, #35596, #3384, #18181 ),
 ( #21217, #3756, #32757, #15330, #3946, #16087, #27446, #27823, #24969, #27262, #1477, #21592, #30296, #4322, #33883, #13241, #1666, #33696, #16461, #15900, #33140, #10571, #27637, #7366, #22149, #18937, #7184, #35973, #4692, #30856, #7925, #4881, #24607, #13421, #30676, #30490, #4511, #19499, #19318, #31046, #36719, #7735, #1286, #18754, #24790, #13051, #28005, #15711, #10010, #21776, #12857, #36156, #10202, #33326, #24425, #36341, #13616, #10386, #21962, #33507, #7552, #19126, #36528, #16275, #1852, #10759, #2037, #25164, #22331, #37271, #34252, #11318, #17011, #2593, #36897, #25904, #2220, #16648, #5430, #8474, #19867, #37085, #23068, #31410, #28552, #22886, #14164, #34436, #31591, #20046, #5614, #16830, #17199, #25718, #2408, #8845, #31772, #14350, #10945, #28738, #2777, #22519, #11500, #20417, #28191, #5804, #5067, #17386, #13802, #37451, #28372, #34615, #8658, #8114, #25351, #8295, #20228, #13981, #28927, #14531, #23256, #25533, #11682, #26087, #2963, #117, #34065, #34801, #11132, #22710, #19686, #31225, #5254, #3334, #35355 ) ),
 .UNSPECIFIED., .F., .F., .F. ) 
 B_SPLINE_SURFACE_WITH_KNOTS ( ( 2, 2 ),
 ( 3, 2, 2, 2, 2, 2, 2, 2, 2, 2, 2, 2, 2, 2, 2, 2, 2, 2, 2, 2, 2, 2, 2, 2, 2, 2, 2, 2, 2, 2, 2, 2, 2, 2, 2, 2, 2, 2, 2, 2, 2, 2, 2, 2, 2, 2, 2, 2, 2, 2, 2, 2, 2, 2, 2, 2, 2, 2, 2, 2, 2, 2, 2, 2, 2, 2, 2, 3 ),
 ( 0.000000000000000000, 1.000000000000000000 ),
 ( 0.000000000000000000, 0.01388888888888888812, 0.02777777777777777624, 0.04166666666666666435, 0.05555555555555555247, 0.06944444444444444753, 0.08333333333333332871, 0.09722222222222222376, 0.1111111111111111049, 0.1250000000000000000, 0.1388888888888888951, 0.1527777777777777901, 0.1666666666666666574, 0.1805555555555555525, 0.1944444444444444475, 0.2083333333333333426, 0.2222222222222222099, 0.2361111111111111049, 0.2500000000000000000, 0.2638888888888888951, 0.2777777777777777901, 0.2916666666666666852, 0.3055555555555555802, 0.3194444444444444198, 0.3333333333333333148, 0.3472222222222222099, 0.3611111111111111049, 0.3750000000000000000, 0.3888888888888888951, 0.4027777777777777901, 0.4166666666666666852, 0.4305555555555555802, 0.4444444444444444198, 0.4583333333333333148, 0.4722222222222222099, 0.4861111111111111049, 0.5000000000000000000, 0.5138888888888888395, 0.5277777777777777901, 0.5416666666666666297, 0.5555555555555555802, 0.5694444444444444198, 0.5833333333333333703, 0.5972222222222222099, 0.6111111111111111605, 0.6250000000000000000, 0.6388888888888888395, 0.6527777777777777901, 0.6666666666666666297, 0.6805555555555555802, 0.6944444444444444198, 0.7083333333333333703, 0.7222222222222222099, 0.7361111111111111605, 0.7500000000000000000, 0.7638888888888888395, 0.7777777777777777901, 0.7916666666666666297, 0.8055555555555555802, 0.8194444444444444198, 0.8333333333333333703, 0.8472222222222222099, 0.8611111111111111605, 0.8750000000000000000, 0.8888888888888888395, 0.9027777777777777901, 0.9166666666666666297, 0.9258785558287927486 ),
 .UNSPECIFIED. ) 
 GEOMETRIC_REPRESENTATION_ITEM ( )  RATIONAL_B_SPLINE_SURFACE ( (
 ( 1.000000000000000000, 0.8660254037844387076, 1.000000000000000000, 0.8660254037844387076, 1.000000000000000000, 0.8660254037844387076, 1.000000000000000000, 0.8660254037844387076, 1.000000000000000000, 0.8660254037844387076, 1.000000000000000000, 0.8660254037844387076, 1.000000000000000000, 0.8660254037844387076, 1.000000000000000000, 0.8660254037844387076, 1.000000000000000000, 0.8660254037844387076, 1.000000000000000000, 0.8660254037844387076, 1.000000000000000000, 0.8660254037844387076, 1.000000000000000000, 0.8660254037844387076, 1.000000000000000000, 0.8660254037844387076, 1.000000000000000000, 0.8660254037844387076, 1.000000000000000000, 0.8660254037844387076, 1.000000000000000000, 0.8660254037844387076, 1.000000000000000000, 0.8660254037844387076, 1.000000000000000000, 0.8660254037844387076, 1.000000000000000000, 0.8660254037844387076, 1.000000000000000000, 0.8660254037844387076, 1.000000000000000000, 0.8660254037844387076, 1.000000000000000000, 0.8660254037844387076, 1.000000000000000000, 0.8660254037844387076, 1.000000000000000000, 0.8660254037844387076, 1.000000000000000000, 0.8660254037844387076, 1.000000000000000000, 0.8660254037844387076, 1.000000000000000000, 0.8660254037844387076, 1.000000000000000000, 0.8660254037844387076, 1.000000000000000000, 0.8660254037844387076, 1.000000000000000000, 0.8660254037844387076, 1.000000000000000000, 0.8660254037844387076, 1.000000000000000000, 0.8660254037844387076, 1.000000000000000000, 0.8660254037844387076, 1.000000000000000000, 0.8660254037844387076, 1.000000000000000000, 0.8660254037844387076, 1.000000000000000000, 0.8660254037844387076, 1.000000000000000000, 0.8660254037844387076, 1.000000000000000000, 0.8660254037844387076, 1.000000000000000000, 0.8660254037844387076, 1.000000000000000000, 0.8660254037844387076, 1.000000000000000000, 0.8660254037844387076, 1.000000000000000000, 0.8660254037844387076, 1.000000000000000000, 0.8660254037844387076, 1.000000000000000000, 0.8660254037844387076, 1.000000000000000000, 0.8660254037844387076, 1.000000000000000000, 0.8660254037844387076, 1.000000000000000000, 0.8660254037844387076, 1.000000000000000000, 0.8660254037844387076, 1.000000000000000000, 0.8660254037844387076, 1.000000000000000000, 0.8660254037844387076, 1.000000000000000000, 0.8660254037844387076, 1.000000000000000000, 0.8660254037844387076, 1.000000000000000000, 0.8660254037844387076, 1.000000000000000000, 0.8660254037844387076, 1.000000000000000000, 0.8660254037844387076, 1.000000000000000000, 0.8660254037844387076, 1.000000000000000000, 0.8660254037844387076, 1.000000000000000000, 0.8660254037844387076, 1.000000000000000000, 0.8660254037844387076, 1.000000000000000000, 0.8660254037844387076, 1.000000000000000000, 0.8660254037844387076, 1.000000000000000000, 0.8660254037844387076, 1.000000000000000000, 0.8660254037844387076, 1.000000000000000000, 0.8660254037844387076, 1.000000000000000000, 0.8660254037844387076, 1.000000000000000000, 0.8660254037844387076, 1.000000000000000000, 0.9111405425767590271, 0.9401542252352144136),
 ( 1.000000000000000000, 0.8660254037844387076, 1.000000000000000000, 0.8660254037844387076, 1.000000000000000000, 0.8660254037844387076, 1.000000000000000000, 0.8660254037844387076, 1.000000000000000000, 0.8660254037844387076, 1.000000000000000000, 0.8660254037844387076, 1.000000000000000000, 0.8660254037844387076, 1.000000000000000000, 0.8660254037844387076, 1.000000000000000000, 0.8660254037844387076, 1.000000000000000000, 0.8660254037844387076, 1.000000000000000000, 0.8660254037844387076, 1.000000000000000000, 0.8660254037844387076, 1.000000000000000000, 0.8660254037844387076, 1.000000000000000000, 0.8660254037844387076, 1.000000000000000000, 0.8660254037844387076, 1.000000000000000000, 0.8660254037844387076, 1.000000000000000000, 0.8660254037844387076, 1.000000000000000000, 0.8660254037844387076, 1.000000000000000000, 0.8660254037844387076, 1.000000000000000000, 0.8660254037844387076, 1.000000000000000000, 0.8660254037844387076, 1.000000000000000000, 0.8660254037844387076, 1.000000000000000000, 0.8660254037844387076, 1.000000000000000000, 0.8660254037844387076, 1.000000000000000000, 0.8660254037844387076, 1.000000000000000000, 0.8660254037844387076, 1.000000000000000000, 0.8660254037844387076, 1.000000000000000000, 0.8660254037844387076, 1.000000000000000000, 0.8660254037844387076, 1.000000000000000000, 0.8660254037844387076, 1.000000000000000000, 0.8660254037844387076, 1.000000000000000000, 0.8660254037844387076, 1.000000000000000000, 0.8660254037844387076, 1.000000000000000000, 0.8660254037844387076, 1.000000000000000000, 0.8660254037844387076, 1.000000000000000000, 0.8660254037844387076, 1.000000000000000000, 0.8660254037844387076, 1.000000000000000000, 0.8660254037844387076, 1.000000000000000000, 0.8660254037844387076, 1.000000000000000000, 0.8660254037844387076, 1.000000000000000000, 0.8660254037844387076, 1.000000000000000000, 0.8660254037844387076, 1.000000000000000000, 0.8660254037844387076, 1.000000000000000000, 0.8660254037844387076, 1.000000000000000000, 0.8660254037844387076, 1.000000000000000000, 0.8660254037844387076, 1.000000000000000000, 0.8660254037844387076, 1.000000000000000000, 0.8660254037844387076, 1.000000000000000000, 0.8660254037844387076, 1.000000000000000000, 0.8660254037844387076, 1.000000000000000000, 0.8660254037844387076, 1.000000000000000000, 0.8660254037844387076, 1.000000000000000000, 0.8660254037844387076, 1.000000000000000000, 0.8660254037844387076, 1.000000000000000000, 0.8660254037844387076, 1.000000000000000000, 0.8660254037844387076, 1.000000000000000000, 0.8660254037844387076, 1.000000000000000000, 0.8660254037844387076, 1.000000000000000000, 0.8660254037844387076, 1.000000000000000000, 0.8660254037844387076, 1.000000000000000000, 0.8660254037844387076, 1.000000000000000000, 0.8660254037844387076, 1.000000000000000000, 0.8660254037844387076, 1.000000000000000000, 0.8660254037844387076, 1.000000000000000000, 0.8660254037844387076, 1.000000000000000000, 0.8660254037844387076, 1.000000000000000000, 0.9111405425767590271, 0.9401542252352144136) ) ) 
 REPRESENTATION_ITEM ( '' )  SURFACE ( )  );
#5405 = CARTESIAN_POINT ( 'NONE',  ( 24.63014976274829593, 3.604726614523240613, 163.1297293768349164 ) ) ;
#5406 = CARTESIAN_POINT ( 'NONE',  ( -6.092822981423970496, 75.38518628210142936, 14.25334919248782661 ) ) ;
#5407 = CARTESIAN_POINT ( 'NONE',  ( 10.31873187879411091, 0.000000000000000000, -7.340624999385508609 ) ) ;
#5408 = CARTESIAN_POINT ( 'NONE',  ( 8.152565276336714462, 25.64768628210144286, -5.233372021372432847 ) ) ;
#5409 = CARTESIAN_POINT ( 'NONE',  ( 27.00000000000007816, 3.464101615137709533, -4.237500000000011369 ) ) ;
#5410 = CARTESIAN_POINT ( 'NONE',  ( -62.07663769728823411, 204.3130714775002730, 3.149950860017883603 ) ) ;
#5411 = ADVANCED_FACE ( 'NONE', ( #19800 ), #2703, .F. ) ;
#5412 = CARTESIAN_POINT ( 'NONE',  ( 2.660918448318279950, 52.09768628210144215, -12.46528703574805697 ) ) ;
#5413 = CARTESIAN_POINT ( 'NONE',  ( -26.99999999999998934, 197.7875000000000227, 15.58845726811991561 ) ) ;
#5414 = DIRECTION ( 'NONE',  ( 0.9961946980917462113, 0.000000000000000000, -0.08715574274765118534 ) ) ;
#5416 = CARTESIAN_POINT ( 'NONE',  ( 13.44051670066911264, 5.407089921784862696, -2.521874999385525840 ) ) ;
#5415 = CARTESIAN_POINT ( 'NONE',  ( -8.152565276336710909, 30.24768628210144783, 5.233372021372435512 ) ) ;
#5417 = CARTESIAN_POINT ( 'NONE',  ( 18.12178482187500350, 249.4843750006145342, 4.985214923628407568 ) ) ;
#5418 = ORIENTED_EDGE ( 'NONE', *, *, #32767, .T. ) ;
#5419 = CARTESIAN_POINT ( 'NONE',  ( 15.00000000000000178, -3.464101615137757051, -4.012499999999996625 ) ) ;
#5420 = CARTESIAN_POINT ( 'NONE',  ( 20.99999999999999289, 243.5874999999999488, -5.999999999999997335 ) ) ;
#5421 = CARTESIAN_POINT ( 'NONE',  ( 24.39809759768267128, 0.000000000000000000, 160.4773609931656608 ) ) ;
#5422 = CARTESIAN_POINT ( 'NONE',  ( 16.56230152254411436, 7.209453229046475009, -2.503124999385547778 ) ) ;
#5423 = CARTESIAN_POINT ( 'NONE',  ( 34.45175145028584041, -5.407089921784855591, 167.9357587796436064 ) ) ;
#5424 = CARTESIAN_POINT ( 'NONE',  ( 15.00000000000000000, 244.5625000000000000, -3.464101615137752166 ) ) ;
#5425 = CARTESIAN_POINT ( 'NONE',  ( 26.99999999999999645, 7.347880794884117764E-16, -7.874999999999992895 ) ) ;
#5426 = EDGE_CURVE ( 'NONE', #1984, #18726, #26847, .T. ) ;
#5427 = CARTESIAN_POINT ( 'NONE',  ( -7.228626920339070061, 75.67268628210145209, 10.49813415415989404 ) ) ;
#5428 = VERTEX_POINT ( 'NONE', #5733 ) ;
#5429 = ORIENTED_EDGE ( 'NONE', *, *, #4835, .T. ) ;
#5430 = CARTESIAN_POINT ( 'NONE',  ( 27.00000000000000355, 196.7375000012290229, -3.306546357697854128E-15 ) ) ;
#5431 = LINE ( 'NONE', #31592, #26520 ) ;
#5432 = CARTESIAN_POINT ( 'NONE',  ( 13.04141134922778988, 37.82731371789854080, -8.927990412390371944 ) ) ;
#5433 = CARTESIAN_POINT ( 'NONE',  ( 21.00000000000000000, 6.646953231504538984, -8.915624999385478588 ) ) ;
#5434 = CARTESIAN_POINT ( 'NONE',  ( 18.12178482187499640, 243.9343750006145513, -4.985214923628404904 ) ) ;
#5435 = CARTESIAN_POINT ( 'NONE',  ( -45.64955436395490551, 213.3788001182225003, -3.209657149897400252 ) ) ;
#5436 = EDGE_CURVE ( 'NONE', #11055, #31857, #18541, .T. ) ;
#5437 = DIRECTION ( 'NONE',  ( 0.000000000000000000, 0.000000000000000000, 1.000000000000000000 ) ) ;
#5438 = CARTESIAN_POINT ( 'NONE',  ( 33.97620792891898134, -5.407089921784861808, 162.5002714581805492 ) ) ;
#5439 = CARTESIAN_POINT ( 'NONE',  ( 6.594114490232462877, 37.53981371789855359, -6.840914352311949109 ) ) ;
#5440 = CARTESIAN_POINT ( 'NONE',  ( 10.31873187879411091, -3.604726614523240613, -9.103124999385528326 ) ) ;
#5441 = VECTOR ( 'NONE', #18205, 1000.000000000000000 ) ;
#5442 = CARTESIAN_POINT ( 'NONE',  ( 10.56230152254410903, 7.347880794884117764E-16, -10.00000000000000000 ) ) ;
#5443 = CARTESIAN_POINT ( 'NONE',  ( 5.778771075727756162E-15, 197.2718750006145569, 31.45816453501075927 ) ) ;
#5444 = CARTESIAN_POINT ( 'NONE',  ( 12.53471296425189330, 20.57731371789854435, 2.311890736173451977 ) ) ;
#5445 =( BOUNDED_CURVE ( )  B_SPLINE_CURVE ( 2, ( #11562, #2650, #23135, #20294, #5868, #26149, #25145, #22131, #10739 ),
 .UNSPECIFIED., .F., .F. ) 
 B_SPLINE_CURVE_WITH_KNOTS ( ( 3, 2, 2, 2, 3 ),
 ( 0.1458333333333333426, 0.1527777777777777901, 0.1666666666666666574, 0.1805555555555555525, 0.1875000000000000000 ),
 .UNSPECIFIED. ) 
 CURVE ( )  GEOMETRIC_REPRESENTATION_ITEM ( )  RATIONAL_B_SPLINE_CURVE ( ( 0.9330127018922194093, 0.9330127018922194093, 1.000000000000000000, 0.8660254037844387076, 1.000000000000000000, 0.8660254037844387076, 1.000000000000000000, 0.9330127018922194093, 0.9330127018922194093 ) ) 
 REPRESENTATION_ITEM ( '' )  );
#5446 = ORIENTED_EDGE ( 'NONE', *, *, #20976, .T. ) ;
#5447 = CARTESIAN_POINT ( 'NONE',  ( 12.50000000000000355, 63.31018628210144072, 0.1745138560725507937 ) ) ;
#5448 = CARTESIAN_POINT ( 'NONE',  ( 22.56230152254410370, 3.464101615137755275, -9.974999998770998744 ) ) ;
#5449 = CYLINDRICAL_SURFACE ( 'NONE', #30803, 27.00000000000000355 ) ;
#5450 = CARTESIAN_POINT ( 'NONE',  ( 24.36051168362275021, 3.604726614523236616, 160.0477520296136049 ) ) ;
#5451 = CARTESIAN_POINT ( 'NONE',  ( 24.00000000000000000, -5.196152422706629359, -0.6937499987709483396 ) ) ;
#5452 = CARTESIAN_POINT ( 'NONE',  ( 10.31873187879411091, -3.604726614523244610, -9.609374999385535077 ) ) ;
#5453 = CARTESIAN_POINT ( 'NONE',  ( 19.56230152254412502, 5.196152422706637353, -0.1500000000000112355 ) ) ;
#5454 = VECTOR ( 'NONE', #10095, 1000.000000000000000 ) ;
#5455 = CARTESIAN_POINT ( 'NONE',  ( -6.594114490232312775, 78.26018628210144357, -6.840914352312096547 ) ) ;
#5456 = CARTESIAN_POINT ( 'NONE',  ( -50.22894823740646331, 235.3444610600932094, 7.500000000000000000 ) ) ;
#5457 = CARTESIAN_POINT ( 'NONE',  ( 2.311890736173175753, 120.5226862821014606, 12.53471296425194836 ) ) ;
#5458 = CARTESIAN_POINT ( 'NONE',  ( 23.99999999999999645, 248.9500000000000171, -5.196152422706631135 ) ) ;
#5459 = CARTESIAN_POINT ( 'NONE',  ( 13.56230152254410548, 5.196152422706630247, -3.562499998771007093 ) ) ;
#5460 = ORIENTED_EDGE ( 'NONE', *, *, #30351, .F. ) ;
#5461 = CARTESIAN_POINT ( 'NONE',  ( 24.51739202056852207, 3.604726614523236616, 161.8409024861787202 ) ) ;
#5462 = CARTESIAN_POINT ( 'NONE',  ( 23.87821517812499650, 4.985214923628404904, -8.840624999385482852 ) ) ;
#5464 = EDGE_CURVE ( 'NONE', #1229, #34407, #29880, .T. ) ;
#5463 = CARTESIAN_POINT ( 'NONE',  ( 27.24356964375000700, 195.5468750006145342, 15.72908226750537075 ) ) ;
#5465 = CARTESIAN_POINT ( 'NONE',  ( 34.40762885551985306, -5.407089921784861808, 167.4314352137346873 ) ) ;
#5466 = CARTESIAN_POINT ( 'NONE',  ( 28.18902776508177510, 5.196152422706636465, 166.5921030979066586 ) ) ;
#5467 = CARTESIAN_POINT ( 'NONE',  ( 20.99999999999999645, 0.000000000000000000, -8.000000000000000000 ) ) ;
#5468 = CARTESIAN_POINT ( 'NONE',  ( 21.00000000000000000, 249.8875000000000171, -6.928203230275506996 ) ) ;
#5469 = CARTESIAN_POINT ( 'NONE',  ( -1.926257025242585782E-15, 198.7906250006145399, -31.45816453501076637 ) ) ;
#5470 = CARTESIAN_POINT ( 'NONE',  ( -11.61527771782809282, 117.4648137178985650, -4.622313124798832717 ) ) ;
#5471 = CARTESIAN_POINT ( 'NONE',  ( 4.944772684328679446, 125.9851862821014521, -11.48171059495397373 ) ) ;
#5472 = VECTOR ( 'NONE', #9119, 1000.000000000000000 ) ;
#5474 = ORIENTED_EDGE ( 'NONE', *, *, #3801, .T. ) ;
#5473 = VERTEX_POINT ( 'NONE', #34182 ) ;
#5475 = CARTESIAN_POINT ( 'NONE',  ( 18.12178482187499640, 242.9218750006145058, -4.985214923628404904 ) ) ;
#5476 = CARTESIAN_POINT ( 'NONE',  ( -20.68320086892770604, 194.6619763917542798, -17.35526438333879540 ) ) ;
#5477 = CARTESIAN_POINT ( 'NONE',  ( -2.908627838312453306, 96.47731371789852517, 15.53471296425188797 ) ) ;
#5478 = CARTESIAN_POINT ( 'NONE',  ( -0.1745138560725500443, 93.21018628210146062, 12.50000000000000355 ) ) ;
#5479 = CARTESIAN_POINT ( 'NONE',  ( 26.75643035624999655, -3.323476615752267715, -0.9656249993854794100 ) ) ;
#5480 = CARTESIAN_POINT ( 'NONE',  ( 27.00000000000001066, 198.0500000012290513, 15.58845726811988897 ) ) ;
#5481 = CARTESIAN_POINT ( 'NONE',  ( 10.69584247140445221, 117.6476862821014464, -6.932735513423970097 ) ) ;
#5482 = CARTESIAN_POINT ( 'NONE',  ( 10.31873187879411091, -3.604726614523240613, -4.153124999385542360 ) ) ;
#5483 = CARTESIAN_POINT ( 'NONE',  ( 15.24356964374999990, 244.7593750006145115, -3.323476615752268604 ) ) ;
#5484 = CARTESIAN_POINT ( 'NONE',  ( 10.56230152254410903, 0.000000000000000000, -1.687499998771019305 ) ) ;
#5485 = CARTESIAN_POINT ( 'NONE',  ( -58.70461230271182984, 208.1428034533959135, -6.469044688360754414 ) ) ;
#5486 = CARTESIAN_POINT ( 'NONE',  ( -8.715434833791929847, 124.2601862821014578, -8.962234695871762469 ) ) ;
#5487 = CARTESIAN_POINT ( 'NONE',  ( 13.56230152254411436, -5.196152422706632912, -3.412499998771051146 ) ) ;
#5488 = ADVANCED_FACE ( 'NONE', ( #28855 ), #5364, .T. ) ;
#5489 = CARTESIAN_POINT ( 'NONE',  ( -46.44122103062156270, 208.3738570449993404, -6.530955311639226935 ) ) ;
#5490 = CARTESIAN_POINT ( 'NONE',  ( 37.10248660225891371, 7.347880794884125653E-16, 165.2099845943227479 ) ) ;
#5491 = AXIS2_PLACEMENT_3D ( 'NONE', #15956, #21462, #20892 ) ;
#5492 = DIRECTION ( 'NONE',  ( -1.000000000000000000, 0.000000000000000000, 0.000000000000000000 ) ) ;
#5493 = CARTESIAN_POINT ( 'NONE',  ( -5.770363421893818234, 97.23518628210146630, -14.38691631536207005 ) ) ;
#5494 = CARTESIAN_POINT ( 'NONE',  ( 4.944772684328679446, 24.78518628210143859, -11.48171059495397373 ) ) ;
#5495 = CARTESIAN_POINT ( 'NONE',  ( 0.000000000000000000, 195.0000000000000000, 0.000000000000000000 ) ) ;
#5496 = CARTESIAN_POINT ( 'NONE',  ( 37.33780710767756972, 7.347880794884125653E-16, 167.8997102791704492 ) ) ;
#5497 = CARTESIAN_POINT ( 'NONE',  ( -1.715153634034234598, 125.1226862821014691, -9.534712964251941258 ) ) ;
#5498 = CARTESIAN_POINT ( 'NONE',  ( 16.56230152254411436, -7.209453229046475009, -0.9281249993855145153 ) ) ;
#5499 = CARTESIAN_POINT ( 'NONE',  ( 1.255007937094097924E-14, 199.4375000000000284, -27.00000000000000355 ) ) ;
#5500 = ORIENTED_EDGE ( 'NONE', *, *, #4969, .T. ) ;
#5501 = DIRECTION ( 'NONE',  ( 0.000000000000000000, 0.000000000000000000, 1.000000000000000000 ) ) ;
#5502 = CARTESIAN_POINT ( 'NONE',  ( 5.233372021372432847, 55.54768628210144499, 8.152565276336710909 ) ) ;
#5503 = LINE ( 'NONE', #28625, #32722 ) ;
#5504 = EDGE_CURVE ( 'NONE', #19908, #22708, #36220, .T. ) ;
#5505 = CARTESIAN_POINT ( 'NONE',  ( 26.99999999999999645, 7.347880794884117764E-16, -5.175000000000013145 ) ) ;
#5506 = CARTESIAN_POINT ( 'NONE',  ( 20.99999999999997513, 245.8937500012290798, -5.999999999999999112 ) ) ;
#5507 = CARTESIAN_POINT ( 'NONE',  ( 27.24356964375000345, 195.1343750006145399, -3.336375036156643733E-15 ) ) ;
#5508 = CARTESIAN_POINT ( 'NONE',  ( 10.56230152254395627, -3.464101615137665124, -8.849999998770995191 ) ) ;
#5509 = CARTESIAN_POINT ( 'NONE',  ( 25.33691262237273989, 0.000000000000000000, 169.8107417041232452 ) ) ;
#5510 = CARTESIAN_POINT ( 'NONE',  ( -5.233372021372612259, 41.85231371789854649, 8.152565276336593669 ) ) ;
#5511 = CARTESIAN_POINT ( 'NONE',  ( 23.99999999999999645, 5.196152422706631135, -9.149999999999991473 ) ) ;
#5512 = VERTEX_POINT ( 'NONE', #20349 ) ;
#5513 = CARTESIAN_POINT ( 'NONE',  ( 18.12178482187500350, 248.9218750006145342, 4.985214923628407568 ) ) ;
#5514 = CARTESIAN_POINT ( 'NONE',  ( 0.1745138560722779009, 68.58981371789856496, 12.50000000000000355 ) ) ;
#5515 = CARTESIAN_POINT ( 'NONE',  ( 22.80587116629411071, 3.604726614523243278, -8.934374999385493510 ) ) ;
#5516 = CARTESIAN_POINT ( 'NONE',  ( 26.75643035624999655, 7.049594010296217766E-16, -9.028124999385489957 ) ) ;
#5517 = CARTESIAN_POINT ( 'NONE',  ( -14.25334919248795096, 143.9148137178985678, 6.092822981423662299 ) ) ;
#5518 = EDGE_CURVE ( 'NONE', #30233, #22653, #29035, .T. ) ;
#5519 = ORIENTED_EDGE ( 'NONE', *, *, #35989, .T. ) ;
#5520 = CARTESIAN_POINT ( 'NONE',  ( 13.44051670066911264, 5.407089921784862696, -0.2718749993855240632 ) ) ;
#5521 = CYLINDRICAL_SURFACE ( 'NONE', #4041, 5.500000000000005329 ) ;
#5522 = CARTESIAN_POINT ( 'NONE',  ( 28.16820783713129472, 5.407089921784862696, 167.7514543563617622 ) ) ;
#5523 = CARTESIAN_POINT ( 'NONE',  ( -38.51711230271183695, 216.4690446883607535, -1.857196546604089393 ) ) ;
#5524 = CARTESIAN_POINT ( 'NONE',  ( -71.06414469631722852, 221.4078028065942476, 5.000000000000000000 ) ) ;
#5525 = CARTESIAN_POINT ( 'NONE',  ( -77.00000000000002842, 214.0000000000000000, -2.499999999999998668 ) ) ;
#5526 = CARTESIAN_POINT ( 'NONE',  ( -36.14955436395489841, 213.3788001182225003, -3.209657149897400252 ) ) ;
#5527 = CARTESIAN_POINT ( 'NONE',  ( -48.22247103062156270, 206.6499508600178672, 5.571401726697986057 ) ) ;
#5528 = CARTESIAN_POINT ( 'NONE',  ( 34.32634463103817524, 5.196152422706631135, 167.8996764003886994 ) ) ;
#5529 = VERTEX_POINT ( 'NONE', #8037 ) ;
#5530 = CARTESIAN_POINT ( 'NONE',  ( -7.234628195640263826, 196.7575961894323484, -27.00000000000003553 ) ) ;
#5531 = CARTESIAN_POINT ( 'NONE',  ( 20.99999999999999645, 6.928203230275506996, -0.5062499987709455640 ) ) ;
#5532 = CARTESIAN_POINT ( 'NONE',  ( 11.08355503943118769, 12.23981371789853512, 10.83675517735179028 ) ) ;
#5533 = CARTESIAN_POINT ( 'NONE',  ( -35.15252896937850124, 205.6499508600178103, -7.303452534266820173 ) ) ;
#5534 = CARTESIAN_POINT ( 'NONE',  ( -0.1745138560725500443, 10.41018628210144215, 12.50000000000000355 ) ) ;
#5535 = CIRCLE ( 'NONE', #30965, 5.999999999999998224 ) ;
#5536 = EDGE_CURVE ( 'NONE', #10052, #37220, #236, .T. ) ;
#5537 = CARTESIAN_POINT ( 'NONE',  ( 10.69584247140445221, 44.04768628210144499, -6.932735513423970097 ) ) ;
#5538 = CARTESIAN_POINT ( 'NONE',  ( 16.56230152254411436, -6.928203230275514990, -3.937500000000034639 ) ) ;
#5539 = ORIENTED_EDGE ( 'NONE', *, *, #5885, .T. ) ;
#5540 = CARTESIAN_POINT ( 'NONE',  ( -14.25334919248782306, 13.28518628210143149, -6.092822981423979378 ) ) ;
#5541 = AXIS2_PLACEMENT_3D ( 'NONE', #7346, #31024, #33862 ) ;
#5542 = CARTESIAN_POINT ( 'NONE',  ( -27.24356964375000345, 194.8531250006145115, 0.000000000000000000 ) ) ;
#5543 = CARTESIAN_POINT ( 'NONE',  ( -27.24356964374999990, 199.7656250006145342, -15.72908226750537786 ) ) ;
#5544 = CARTESIAN_POINT ( 'NONE',  ( 22.56230152254411792, 7.347880794884125653E-16, -6.525000000000058975 ) ) ;
#5545 = CARTESIAN_POINT ( 'NONE',  ( 26.99999999999999645, 7.347880794884117764E-16, -3.824999999999994849 ) ) ;
#5546 = EDGE_CURVE ( 'NONE', #33961, #26752, #22404, .T. ) ;
#5547 = CARTESIAN_POINT ( 'NONE',  ( 20.99999999999999645, 185.0294372515228645, 0.000000000000000000 ) ) ;
#5548 = DIRECTION ( 'NONE',  ( -0.000000000000000000, -1.000000000000000000, -0.000000000000000000 ) ) ;
#5549 = CARTESIAN_POINT ( 'NONE',  ( 26.75643035624999655, 245.6218750006145513, -3.323476615752271712 ) ) ;
#5550 = CARTESIAN_POINT ( 'NONE',  ( 0.1745138560723095977, 96.18981371789855928, 9.500000000000005329 ) ) ;
#5551 = CARTESIAN_POINT ( 'NONE',  ( 26.75643035624999655, 242.4343750006145513, -7.049594010296217766E-16 ) ) ;
#5552 = VERTEX_POINT ( 'NONE', #799 ) ;
#5553 = CARTESIAN_POINT ( 'NONE',  ( -63.26413769728824121, 213.1499508600178672, 5.686928522499718142 ) ) ;
#5554 = CARTESIAN_POINT ( 'NONE',  ( 25.17429694808911833, 3.464101615137614498, 166.5547119179464346 ) ) ;
#5555 = CARTESIAN_POINT ( 'NONE',  ( 26.99999999999999645, 248.8937500012290229, 3.464101615137751278 ) ) ;
#5556 = ORIENTED_EDGE ( 'NONE', *, *, #24319, .F. ) ;
#5557 = CARTESIAN_POINT ( 'NONE',  ( 8.715434833792128799, 111.1398137178985621, -8.962234695871567070 ) ) ;
#5558 = CARTESIAN_POINT ( 'NONE',  ( 10.31873187879410736, -3.604726614523244610, -2.409374999385539340 ) ) ;
#5559 = CARTESIAN_POINT ( 'NONE',  ( 30.71105627401454896, -7.209453229046475009, 160.9978811270534891 ) ) ;
#5560 = CARTESIAN_POINT ( 'NONE',  ( 26.75643035624999655, 7.049594010296217766E-16, -2.278124999385483740 ) ) ;
#5561 = CARTESIAN_POINT ( 'NONE',  ( -12.53471296425189152, 80.37731371789854506, -2.311890736173453753 ) ) ;
#5562 = CARTESIAN_POINT ( 'NONE',  ( -1.909035429704832693E-15, 195.3874999999999886, -31.17691453623979214 ) ) ;
#5563 = VERTEX_POINT ( 'NONE', #6106 ) ;
#5564 = VERTEX_POINT ( 'NONE', #18257 ) ;
#5565 = ORIENTED_EDGE ( 'NONE', *, *, #31874, .T. ) ;
#5566 = CARTESIAN_POINT ( 'NONE',  ( 15.00000000000000000, 3.464101615137752166, -6.281249998770928045 ) ) ;
#5567 = CARTESIAN_POINT ( 'NONE',  ( 15.24356964374999990, 3.323476615752268604, -3.778124999385444660 ) ) ;
#5568 = FACE_OUTER_BOUND ( 'NONE', #9147, .T. ) ;
#5569 = CARTESIAN_POINT ( 'NONE',  ( 18.12178482187499640, 247.8718750006145228, -4.985214923628404904 ) ) ;
#5570 = CARTESIAN_POINT ( 'NONE',  ( 12.50000000000000355, 54.11018628210144499, 0.1745138560725507937 ) ) ;
#5571 = CARTESIAN_POINT ( 'NONE',  ( -47.62127896937848703, 216.5309553116392181, 1.626142955000506429 ) ) ;
#5572 = CARTESIAN_POINT ( 'NONE',  ( 19.95279056986836963, 210.3927035363167022, -5.999999999999998224 ) ) ;
#5573 = CARTESIAN_POINT ( 'NONE',  ( -46.63169563604517265, 210.1155267958017703, 4.499999999999996447 ) ) ;
#5574 =( NAMED_UNIT ( * ) SI_UNIT ( $, .STERADIAN. ) SOLID_ANGLE_UNIT ( ) );
#5575 = CARTESIAN_POINT ( 'NONE',  ( 27.93736555800505172, -5.196152422706632912, 163.7155909083910501 ) ) ;
#5576 = CARTESIAN_POINT ( 'NONE',  ( -11.61527771782809282, 108.2648137178985621, -4.622313124798832717 ) ) ;
#5577 = CARTESIAN_POINT ( 'NONE',  ( -69.59747103062156270, 212.3500491399821613, -3.839350919129076445 ) ) ;
#5578 = CARTESIAN_POINT ( 'NONE',  ( -48.02455436395490551, 203.6929966515020283, 6.137860380172978303 ) ) ;
#5579 = CARTESIAN_POINT ( 'NONE',  ( 26.75643035624999655, 3.323476615752271268, -4.490624999385483207 ) ) ;
#5580 = CARTESIAN_POINT ( 'NONE',  ( 22.56230152254478583, -3.464101615137372470, -5.212500000000051870 ) ) ;
#5581 = CARTESIAN_POINT ( 'NONE',  ( 13.04141134922778988, 83.82731371789856212, -8.927990412390371944 ) ) ;
#5582 = CARTESIAN_POINT ( 'NONE',  ( -30.60044563604515488, 205.1570982666397072, -4.673758765035155527 ) ) ;
#5583 = ORIENTED_EDGE ( 'NONE', *, *, #175, .F. ) ;
#5584 = CARTESIAN_POINT ( 'NONE',  ( 36.91292286189034400, -3.464101615137475942, 163.0432611271974679 ) ) ;
#5585 = CARTESIAN_POINT ( 'NONE',  ( -11.61527771782819940, 94.93518628210145494, 4.622313124798574258 ) ) ;
#5586 = CARTESIAN_POINT ( 'NONE',  ( 13.04141134922759804, 64.17268628210143788, 8.927990412390657937 ) ) ;
#5587 = CARTESIAN_POINT ( 'NONE',  ( 13.56230152254410370, 5.196152422706630247, -9.862499998771006915 ) ) ;
#5588 = CARTESIAN_POINT ( 'NONE',  ( 37.01094158893428698, -3.604726614523238837, 161.3689720562275340 ) ) ;
#5589 = CARTESIAN_POINT ( 'NONE',  ( -14.25334919248782306, 59.28518628210144925, -6.092822981423979378 ) ) ;
#5590 = CARTESIAN_POINT ( 'NONE',  ( 22.80587116629411071, 3.604726614523238837, -5.728124999385511451 ) ) ;
#5591 = DIRECTION ( 'NONE',  ( 0.000000000000000000, 0.000000000000000000, 1.000000000000000000 ) ) ;
#5592 = CARTESIAN_POINT ( 'NONE',  ( -54.55580436395489841, 216.5000000000000000, 0.1155267958017343610 ) ) ;
#5593 = AXIS2_PLACEMENT_3D ( 'NONE', #34978, #26823, #12424 ) ;
#5594 = CARTESIAN_POINT ( 'NONE',  ( 15.00000000000000000, 243.3062500012290457, 0.000000000000000000 ) ) ;
#5595 = CARTESIAN_POINT ( 'NONE',  ( -7.228626920339069173, 38.87268628210144072, 10.49813415415989581 ) ) ;
#5596 = CARTESIAN_POINT ( 'NONE',  ( -27.00000000000000355, 199.0625000000000000, -15.58845726811989429 ) ) ;
#5597 = CARTESIAN_POINT ( 'NONE',  ( 18.00000000000000000, 240.0249999999999773, -5.196152422706630247 ) ) ;
#5598 = CARTESIAN_POINT ( 'NONE',  ( -8.843639120294326972, 21.33518628210144641, 3.474262827703335166 ) ) ;
#5599 = CARTESIAN_POINT ( 'NONE',  ( 20.99999999999999645, 248.3968750006145569, -6.646953231504538984 ) ) ;
#5600 = VERTEX_POINT ( 'NONE', #21295 ) ;
#5601 = CARTESIAN_POINT ( 'NONE',  ( 26.99999999999999645, 7.347880794884117764E-16, -4.725000000000006750 ) ) ;
#5603 = CARTESIAN_POINT ( 'NONE',  ( 31.19395356112219986, -6.928203230275514990, 166.5174223755558955 ) ) ;
#5602 = PRODUCT ( 'coupler', 'coupler', '', ( #1943 ) ) ;
#5604 = CARTESIAN_POINT ( 'NONE',  ( 24.39482925732963281, 3.604726614523240613, 160.4400036919872150 ) ) ;
#5605 = CARTESIAN_POINT ( 'NONE',  ( 22.80587116629411426, -3.604726614523235284, -3.103124999385563410 ) ) ;
#5606 = CARTESIAN_POINT ( 'NONE',  ( 24.62194742831900030, -3.464101615137761048, 160.2413280175656212 ) ) ;
#5607 =( BOUNDED_CURVE ( )  B_SPLINE_CURVE ( 2, ( #8836, #6550, #15081, #6173, #32321, #26444, #26631 ),
 .UNSPECIFIED., .F., .F. ) 
 B_SPLINE_CURVE_WITH_KNOTS ( ( 3, 2, 2, 3 ),
 ( 0.2826086956521748905, 0.2898550724637692366, 0.2971014492753635827, 0.3043478260869579288 ),
 .UNSPECIFIED. ) 
 CURVE ( )  GEOMETRIC_REPRESENTATION_ITEM ( )  RATIONAL_B_SPLINE_CURVE ( ( 0.9999999999999815703, 0.8660254037844571373, 1.000000000000000000, 0.8660254037844387076, 1.000000000000000000, 0.8660254037844130615, 1.000000000000025535 ) ) 
 REPRESENTATION_ITEM ( '' )  );
#5608 = CARTESIAN_POINT ( 'NONE',  ( 21.00000000000000000, 242.4624999999999773, 6.928203230275506996 ) ) ;
#5609 = LINE ( 'NONE', #28368, #14857 ) ;
#5610 = CARTESIAN_POINT ( 'NONE',  ( -4.622313124798576922, 60.43518628210145494, -11.61527771782819762 ) ) ;
#5611 = ORIENTED_EDGE ( 'NONE', *, *, #15016, .F. ) ;
#5612 = ORIENTED_EDGE ( 'NONE', *, *, #16982, .F. ) ;
#5613 = CARTESIAN_POINT ( 'NONE',  ( 20.99999999999999645, 0.000000000000000000, -8.000000000000000000 ) ) ;
#5614 = CARTESIAN_POINT ( 'NONE',  ( 27.00000000000000355, 196.2875000012290343, -3.306546357697854128E-15 ) ) ;
#5616 = DIRECTION ( 'NONE',  ( -0.1219804832088915297, -0.9925324990730154395, 0.000000000000000000 ) ) ;
#5615 = VECTOR ( 'NONE', #34016, 1000.000000000000000 ) ;
#5617 = CARTESIAN_POINT ( 'NONE',  ( -10.83675517735179028, 42.13981371789854791, 11.08355503943118947 ) ) ;
#5618 = CARTESIAN_POINT ( 'NONE',  ( 23.87821517812499650, 4.985214923628404904, -9.403124999385475746 ) ) ;
#5619 = CARTESIAN_POINT ( 'NONE',  ( 18.12178482187500350, 243.6343750006145115, 4.985214923628407568 ) ) ;
#5620 = CARTESIAN_POINT ( 'NONE',  ( -45.84747103062156981, 212.3500491399821613, -3.839350919129076445 ) ) ;
#5621 = CARTESIAN_POINT ( 'NONE',  ( 21.00000000000000355, 0.000000000000000000, 50.00000000000001421 ) ) ;
#5622 = CARTESIAN_POINT ( 'NONE',  ( 33.85854767620964623, -5.407089921784861808, 161.1554086157566985 ) ) ;
#5623 = CARTESIAN_POINT ( 'NONE',  ( 2.064181346179061460, 13.10231371789855181, 9.465287035748106703 ) ) ;
#5624 = CARTESIAN_POINT ( 'NONE',  ( -67.81622103062156270, 211.6261429550005744, 6.530955311639227823 ) ) ;
#5625 = ADVANCED_FACE ( 'NONE', ( #12562 ), #32644, .F. ) ;
#5626 =( BOUNDED_CURVE ( )  B_SPLINE_CURVE ( 2, ( #25808, #16551, #5153, #33971, #19221 ),
 .UNSPECIFIED., .F., .F. ) 
 B_SPLINE_CURVE_WITH_KNOTS ( ( 3, 2, 3 ),
 ( 0.000000000000000000, 0.01388888888888888985, 0.02083333333333333565 ),
 .UNSPECIFIED. ) 
 CURVE ( )  GEOMETRIC_REPRESENTATION_ITEM ( )  RATIONAL_B_SPLINE_CURVE ( ( 1.000000000000000000, 0.8660254037844387076, 1.000000000000000000, 0.9330127018922192983, 0.9330127018922194093 ) ) 
 REPRESENTATION_ITEM ( '' )  );
#5627 = CARTESIAN_POINT ( 'NONE',  ( 27.08132523266538172, 194.9999999999999432, -1.221504123172654444 ) ) ;
#5628 = CARTESIAN_POINT ( 'NONE',  ( -27.24356964374999635, 197.1968750006145115, 15.72908226750539384 ) ) ;
#5629 = B_SPLINE_CURVE_WITH_KNOTS ( 'NONE', 1,
 ( #32774, #27095 ),
 .UNSPECIFIED., .F., .F.,
 ( 2, 2 ),
 ( 0.000000000000000000, 1.000000000000000000 ),
 .UNSPECIFIED. ) ;
#5630 = CARTESIAN_POINT ( 'NONE',  ( -13.04141134922778456, 134.4273137178984996, 8.927990412390377273 ) ) ;
#5631 = ADVANCED_BREP_SHAPE_REPRESENTATION ( '', ( #20231, #17215 ), #9874 ) ;
#5632 = ORIENTED_EDGE ( 'NONE', *, *, #12144, .T. ) ;
#5633 = CARTESIAN_POINT ( 'NONE',  ( -12.46528703574805697, 58.99768628210144783, -2.660918448318280838 ) ) ;
#5634 = CARTESIAN_POINT ( 'NONE',  ( 20.99999999999999645, 185.0294372515228645, -5.999999999999999112 ) ) ;
#5635 = CARTESIAN_POINT ( 'NONE',  ( 21.00000000000001066, 247.4124999999999943, 5.999999999999998224 ) ) ;
#5636 = CARTESIAN_POINT ( 'NONE',  ( 31.39250523762275691, 7.209453229046482114, 168.7868784227583205 ) ) ;
#5637 = CARTESIAN_POINT ( 'NONE',  ( 18.00000000000000000, 5.196152422706630247, -3.618749998770959486 ) ) ;
#5638 =( GEOMETRIC_REPRESENTATION_CONTEXT ( 3 ) GLOBAL_UNCERTAINTY_ASSIGNED_CONTEXT ( ( #13508 ) ) GLOBAL_UNIT_ASSIGNED_CONTEXT ( ( #28887, #11461, #29253 ) ) REPRESENTATION_CONTEXT ( 'NONE', 'WORKASPACE' ) );
#5639 = CARTESIAN_POINT ( 'NONE',  ( 19.68408634441910721, 5.407089921784862696, -8.896874999385516958 ) ) ;
#5640 = CARTESIAN_POINT ( 'NONE',  ( 27.00000000000000355, 197.1875000012290400, -3.306546357697854128E-15 ) ) ;
#5641 = CARTESIAN_POINT ( 'NONE',  ( 8.843639120294328748, 81.13518628210145778, -3.474262827703334722 ) ) ;
#5642 = CARTESIAN_POINT ( 'NONE',  ( 16.56230152254411081, -6.928203230275506996, -1.124999998771007759 ) ) ;
#5643 = ADVANCED_FACE ( 'NONE', ( #23748 ), #15596, .F. ) ;
#5644 = CARTESIAN_POINT ( 'NONE',  ( 8.962234695871762469, 89.76018628210144357, -8.715434833791931624 ) ) ;
#5645 = CARTESIAN_POINT ( 'NONE',  ( 26.99999999999999645, 249.7750000000000057, -7.347880794884117764E-16 ) ) ;
#5646 = CARTESIAN_POINT ( 'NONE',  ( 20.99999999999999645, 0.000000000000000000, -8.000000000000000000 ) ) ;
#5647 = ORIENTED_EDGE ( 'NONE', *, *, #8088, .F. ) ;
#5648 = CARTESIAN_POINT ( 'NONE',  ( 27.67632261399923976, -5.407089921784859143, 162.1291805290064474 ) ) ;
#5649 = CARTESIAN_POINT ( 'NONE',  ( 26.75643035624999655, -3.323476615752267715, -7.153124999385460647 ) ) ;
#5650 = CARTESIAN_POINT ( 'NONE',  ( 15.06230152254410548, 0.000000000000000000, 0.000000000000000000 ) ) ;
#5651 = CARTESIAN_POINT ( 'NONE',  ( 34.49914238540488043, 5.407089921784862696, 168.4774396467310282 ) ) ;
#5652 = CARTESIAN_POINT ( 'NONE',  ( 31.09590335053109555, 6.928203230275514990, 165.3967033402026914 ) ) ;
#5653 = LINE ( 'NONE', #34651, #18679 ) ;
#5654 = CARTESIAN_POINT ( 'NONE',  ( 15.24356964374999990, 241.2718750006145569, -3.323476615752268604 ) ) ;
#5655 = CARTESIAN_POINT ( 'NONE',  ( 5.778771075727756162E-15, 198.5656250006145456, 31.45816453501076637 ) ) ;
#5656 = EDGE_CURVE ( 'NONE', #23999, #27522, #28648, .T. ) ;
#5657 = CARTESIAN_POINT ( 'NONE',  ( 4.944772684328420986, 114.0148137178985621, 11.48171059495408208 ) ) ;
#5658 = CIRCLE ( 'NONE', #15356, 25.00000000000000000 ) ;
#5659 = CARTESIAN_POINT ( 'NONE',  ( 12.53471296425194659, 127.4226862821014663, -2.311890736173178418 ) ) ;
#5661 = EDGE_LOOP ( 'NONE', ( #4559, #32064, #23894, #12330 ) ) ;
#5660 = ORIENTED_EDGE ( 'NONE', *, *, #12641, .T. ) ;
#5662 = CARTESIAN_POINT ( 'NONE',  ( -27.24356964374999635, 197.5906250006145228, 15.72908226750539384 ) ) ;
#5663 = CARTESIAN_POINT ( 'NONE',  ( 21.00000000000000000, 242.8843750006145399, -6.646953231504538984 ) ) ;
#5664 = CARTESIAN_POINT ( 'NONE',  ( 19.39230484541326760, 243.7924038105676630, 5.999999999999999112 ) ) ;
#5665 = CARTESIAN_POINT ( 'NONE',  ( -8.632099005475794229, 97.05231371789855643, 13.23911966647199812 ) ) ;
#5666 = CARTESIAN_POINT ( 'NONE',  ( 15.24356964375000167, -3.323476615752272600, -2.915624999385482141 ) ) ;
#5667 = PRESENTATION_LAYER_ASSIGNMENT (  '', '', ( #9309 ) ) ;
#5668 = CARTESIAN_POINT ( 'NONE',  ( -26.99999999999998934, 197.0000000012290400, 15.58845726811991561 ) ) ;
#5669 = CARTESIAN_POINT ( 'NONE',  ( -0.1745138560723084320, 73.18981371789854506, -9.500000000000005329 ) ) ;
#5670 = CARTESIAN_POINT ( 'NONE',  ( 19.68408634441910721, -5.407089921784855591, -3.590624999385533478 ) ) ;
#5671 = CIRCLE ( 'NONE', #6276, 5.500000000000005329 ) ;
#5672 = CARTESIAN_POINT ( 'NONE',  ( 18.12178482187499640, 241.5718750006145399, -4.985214923628404904 ) ) ;
#5673 = CARTESIAN_POINT ( 'NONE',  ( 10.69584247140429589, 57.95231371789854791, 6.932735513424201024 ) ) ;
#5674 = EDGE_CURVE ( 'NONE', #22116, #2263, #17878, .T. ) ;
#5675 = CARTESIAN_POINT ( 'NONE',  ( -4.944772684328673229, 121.3851862821014578, 11.48171059495397728 ) ) ;
#5676 = CARTESIAN_POINT ( 'NONE',  ( 10.56230152254411259, 3.464101615137752166, -4.424999998771030008 ) ) ;
#5677 = CARTESIAN_POINT ( 'NONE',  ( -44.85788769728821990, 216.4690446883607535, 1.857196546604031662 ) ) ;
#5678 = LINE ( 'NONE', #19749, #16152 ) ;
#5679 = DIRECTION ( 'NONE',  ( 0.000000000000000000, -1.000000000000000000, 0.000000000000000000 ) ) ;
#5680 = CARTESIAN_POINT ( 'NONE',  ( 15.53471296425195369, 99.82268628210142936, -2.908627838312120684 ) ) ;
#5681 = CARTESIAN_POINT ( 'NONE',  ( -8.715434833791929847, 13.86018628210145032, -8.962234695871762469 ) ) ;
#5682 = CARTESIAN_POINT ( 'NONE',  ( 20.99999999999999645, 185.0294372515228645, 5.999999999999999112 ) ) ;
#5683 = EDGE_CURVE ( 'NONE', #32891, #37310, #2571, .T. ) ;
#5684 = CARTESIAN_POINT ( 'NONE',  ( 7.954856959092191815, 137.7726862821014606, 5.529263428287477744 ) ) ;
#5685 = CARTESIAN_POINT ( 'NONE',  ( 36.74950584413092258, 7.347880794884125653E-16, 161.1753960670511674 ) ) ;
#5686 = ORIENTED_EDGE ( 'NONE', *, *, #3559, .F. ) ;
#5687 = CARTESIAN_POINT ( 'NONE',  ( 31.41701779027052766, -7.209453229046475009, 169.0670581815966216 ) ) ;
#5688 = CIRCLE ( 'NONE', #33550, 7.500000000000000000 ) ;
#5689 = CARTESIAN_POINT ( 'NONE',  ( -8.843639120294326972, 67.33518628210143220, 3.474262827703335166 ) ) ;
#5690 = CARTESIAN_POINT ( 'NONE',  ( 10.69584247140445221, 16.44768628210144357, -6.932735513423970097 ) ) ;
#5691 = CARTESIAN_POINT ( 'NONE',  ( 26.75643035624999655, -3.323476615752267715, -0.8531249993854884694 ) ) ;
#5692 = EDGE_CURVE ( 'NONE', #34895, #529, #35482, .T. ) ;
#5693 = LINE ( 'NONE', #37339, #24704 ) ;
#5694 = STYLED_ITEM ( 'NONE', ( #22290 ), #22840 ) ;
#5695 = LINE ( 'NONE', #31121, #17912 ) ;
#5696 = CARTESIAN_POINT ( 'NONE',  ( -47.00000000000000711, 244.5000000000000000, 2.500000000000001776 ) ) ;
#5697 = CARTESIAN_POINT ( 'NONE',  ( -3.656739830522513390, 194.9999999999999716, 27.01108501465073886 ) ) ;
#5698 = CARTESIAN_POINT ( 'NONE',  ( 9.534712964251900402, 38.97731371789853938, 1.715153634034445540 ) ) ;
#5699 = CARTESIAN_POINT ( 'NONE',  ( -27.24356964375000345, 198.9593750006145285, 0.000000000000000000 ) ) ;
#5700 = ORIENTED_EDGE ( 'NONE', *, *, #4108, .F. ) ;
#5701 = VERTEX_POINT ( 'NONE', #3269 ) ;
#5702 = CARTESIAN_POINT ( 'NONE',  ( 18.12178482187499640, 248.7718750006145001, -4.985214923628404904 ) ) ;
#5703 = CARTESIAN_POINT ( 'NONE',  ( -2.311890736173447980, 41.27731371789855785, 12.53471296425189330 ) ) ;
#5704 = CARTESIAN_POINT ( 'NONE',  ( 22.80587116629411426, 7.646167579472024665E-16, -8.071874999385524774 ) ) ;
#5705 = CARTESIAN_POINT ( 'NONE',  ( 21.00000000000000000, -6.646953231504538984, -9.140624999385492444 ) ) ;
#5706 = CARTESIAN_POINT ( 'NONE',  ( 2.311890736173452865, 18.27731371789853299, -12.53471296425189152 ) ) ;
#5707 = EDGE_CURVE ( 'NONE', #10453, #29410, #9344, .T. ) ;
#5708 = ORIENTED_EDGE ( 'NONE', *, *, #9030, .F. ) ;
#5709 = CARTESIAN_POINT ( 'NONE',  ( 10.31873187879410736, -3.604726614523244610, -4.659374999385518024 ) ) ;
#5710 = CARTESIAN_POINT ( 'NONE',  ( 13.62178482187501416, 199.5031250006145456, 23.59362340125806767 ) ) ;
#5711 = CARTESIAN_POINT ( 'NONE',  ( 24.86873860851999041, 0.000000000000000000, 165.8568123628610920 ) ) ;
#5712 = CARTESIAN_POINT ( 'NONE',  ( -41.88169563604517265, 210.1155267958017703, 6.500000000000000888 ) ) ;
#5713 = CARTESIAN_POINT ( 'NONE',  ( 10.56230152254411081, 0.000000000000000000, -0.3374999987710014526 ) ) ;
#5714 = CARTESIAN_POINT ( 'NONE',  ( -13.08024444877374748, 195.0000000000000000, 23.89571502063673591 ) ) ;
#5715 = ADVANCED_FACE ( 'NONE', ( #29993 ), #4024, .T. ) ;
#5716 = CARTESIAN_POINT ( 'NONE',  ( -60.68377896937850835, 208.9097554298617183, 4.530955311639234040 ) ) ;
#5717 = CARTESIAN_POINT ( 'NONE',  ( -46.24330436395489841, 210.1155267958017134, -6.500000000000000888 ) ) ;
#5718 = CARTESIAN_POINT ( 'NONE',  ( 28.22540379330944660, -5.407089921784859143, 168.4052071269844930 ) ) ;
#5719 = ORIENTED_EDGE ( 'NONE', *, *, #21771, .T. ) ;
#5720 = CARTESIAN_POINT ( 'NONE',  ( -7.234628195640289583, 197.7700961906613770, -27.00000000000001421 ) ) ;
#5721 = CARTESIAN_POINT ( 'NONE',  ( 13.56230152254410726, 5.196152422706636465, -1.425000000000037348 ) ) ;
#5722 = CARTESIAN_POINT ( 'NONE',  ( 5.770363421894130873, 27.76481371789854791, -14.38691631536193860 ) ) ;
#5723 = CARTESIAN_POINT ( 'NONE',  ( -66.23288769728823411, 201.5309553116392181, -2.393094931466246855 ) ) ;
#5724 = CARTESIAN_POINT ( 'NONE',  ( 12.50000000000000355, 8.110186282101444988, 0.1745138560725507937 ) ) ;
#5725 = CARTESIAN_POINT ( 'NONE',  ( -0.1745138560725500443, 47.21018628210143930, 12.50000000000000355 ) ) ;
#5726 = CARTESIAN_POINT ( 'NONE',  ( 22.56230152254412147, 3.464101615137759271, -4.687500000000039080 ) ) ;
#5727 =( BOUNDED_CURVE ( )  B_SPLINE_CURVE ( 2, ( #15743, #1135, #10045, #21255, #1325, #32604, #21622, #18600, #26723 ),
 .UNSPECIFIED., .F., .F. ) 
 B_SPLINE_CURVE_WITH_KNOTS ( ( 3, 2, 2, 2, 3 ),
 ( 0.02083333333333333565, 0.02777777777777777624, 0.04166666666666666435, 0.05555555555555555247, 0.06250000000000000000 ),
 .UNSPECIFIED. ) 
 CURVE ( )  GEOMETRIC_REPRESENTATION_ITEM ( )  RATIONAL_B_SPLINE_CURVE ( ( 0.9330127018922194093, 0.9330127018922194093, 1.000000000000000000, 0.8660254037844387076, 1.000000000000000000, 0.8660254037844387076, 1.000000000000000000, 0.9330127018922194093, 0.9330127018922194093 ) ) 
 REPRESENTATION_ITEM ( '' )  );
#5728 = VERTEX_POINT ( 'NONE', #26767 ) ;
#5729 = CARTESIAN_POINT ( 'NONE',  ( -39.71205436395490551, 214.6737587650351884, 4.842901733360205796 ) ) ;
#5730 = EDGE_CURVE ( 'NONE', #31332, #31979, #16874, .T. ) ;
#5731 = CARTESIAN_POINT ( 'NONE',  ( -3.253724281355068545E-15, 198.6500000012290172, -27.00000000000000000 ) ) ;
#5732 = CARTESIAN_POINT ( 'NONE',  ( 27.24356964375000700, 196.8968750006145285, 15.72908226750537075 ) ) ;
#5733 = CARTESIAN_POINT ( 'NONE',  ( 5.438367727407757775E-14, 198.0875000000000057, -27.00000000000000355 ) ) ;
#5734 = DIRECTION ( 'NONE',  ( 0.000000000000000000, 0.000000000000000000, -1.000000000000000000 ) ) ;
#5735 = LINE ( 'NONE', #8965, #3110 ) ;
#5736 = FACE_OUTER_BOUND ( 'NONE', #16157, .T. ) ;
#5737 = CARTESIAN_POINT ( 'NONE',  ( 15.24356964375000167, 244.9468750006145399, 3.323476615752272600 ) ) ;
#5738 = CARTESIAN_POINT ( 'NONE',  ( -6.840914352311947333, 90.43981371789854506, -6.594114490232462877 ) ) ;
#5739 = CARTESIAN_POINT ( 'NONE',  ( 18.12178482187500350, 241.8343750006145285, 4.985214923628407568 ) ) ;
#5740 = ORIENTED_EDGE ( 'NONE', *, *, #30304, .T. ) ;
#5741 = CARTESIAN_POINT ( 'NONE',  ( -50.99330436395489841, 210.1155267958017134, -6.500000000000000888 ) ) ;
#5742 = CARTESIAN_POINT ( 'NONE',  ( 34.13024420985595953, 5.196152422706631135, 165.6582383296822343 ) ) ;
#5743 = CARTESIAN_POINT ( 'NONE',  ( 23.99999999999999645, 246.3062500012290457, -5.196152422706631135 ) ) ;
#5744 = VERTEX_POINT ( 'NONE', #20535 ) ;
#5745 = CARTESIAN_POINT ( 'NONE',  ( -12.50000000000000355, 98.48981371789855643, 0.1745138560722786503 ) ) ;
#5746 = CARTESIAN_POINT ( 'NONE',  ( 16.56230152254411436, -7.209453229046482114, -0.5343749993854981506 ) ) ;
#5747 = CARTESIAN_POINT ( 'NONE',  ( 33.74578993402985816, -5.407089921784855591, 159.8665817251004739 ) ) ;
#5748 = VECTOR ( 'NONE', #24135, 1000.000000000000000 ) ;
#5749 = CARTESIAN_POINT ( 'NONE',  ( 15.24356964374999990, 0.000000000000000000, -2.503124999385486493 ) ) ;
#5750 = CARTESIAN_POINT ( 'NONE',  ( -4.622313124798826500, 69.16481371789855359, 11.61527771782809637 ) ) ;
#5751 = CARTESIAN_POINT ( 'NONE',  ( -13.62178482187498396, 199.0343750006145456, 23.59362340125808188 ) ) ;
#5752 = ORIENTED_EDGE ( 'NONE', *, *, #7976, .F. ) ;
#5753 = AXIS2_PLACEMENT_3D ( 'NONE', #20449, #14938, #3177 ) ;
#5754 = EDGE_LOOP ( 'NONE', ( #5802, #16177, #4061 ) ) ;
#5755 = ORIENTED_EDGE ( 'NONE', *, *, #776, .F. ) ;
#5756 = CARTESIAN_POINT ( 'NONE',  ( 21.00000000000000000, 6.928203230275506996, -7.256249998770945453 ) ) ;
#5757 = CARTESIAN_POINT ( 'NONE',  ( 26.75643035624999655, -3.323476615752267271, -2.653124999385471305 ) ) ;
#5758 = DIRECTION ( 'NONE',  ( 0.000000000000000000, 0.000000000000000000, -1.000000000000000000 ) ) ;
#5759 = CARTESIAN_POINT ( 'NONE',  ( 15.24356964374999990, 247.4593750006145285, -3.323476615752268604 ) ) ;
#5760 = CARTESIAN_POINT ( 'NONE',  ( -12.53471296425194836, 67.62268628210145494, 2.311890736173176641 ) ) ;
#5761 = CARTESIAN_POINT ( 'NONE',  ( -49.60044563604517265, 205.1570982666397072, -4.673758765035155527 ) ) ;
#5762 = CARTESIAN_POINT ( 'NONE',  ( 14.04484906357430773, 216.9551509364345350, -0.1802446458350883129 ) ) ;
#5763 = CARTESIAN_POINT ( 'NONE',  ( -38.12127896937850835, 214.5309553116392749, 1.090244570138288127 ) ) ;
#5764 = SURFACE_STYLE_USAGE ( .BOTH. , #34577 ) ;
#5765 = CARTESIAN_POINT ( 'NONE',  ( 24.90629303914032988, -3.464101615137757051, 163.4914132213143034 ) ) ;
#5766 = CARTESIAN_POINT ( 'NONE',  ( 10.49813415416005213, 111.4273137178985564, -7.228626920338837358 ) ) ;
#5767 = CARTESIAN_POINT ( 'NONE',  ( -55.74330436395489841, 210.1155267958017703, -4.499999999999996447 ) ) ;
#5769 = EDGE_CURVE ( 'NONE', #27974, #14162, #11976, .T. ) ;
#5768 = CARTESIAN_POINT ( 'NONE',  ( -41.69122103062156270, 207.8379586601371329, -8.530955311639223382 ) ) ;
#5770 = CARTESIAN_POINT ( 'NONE',  ( 15.24356964374999990, 0.000000000000000000, -5.203124999385494220 ) ) ;
#5771 = CARTESIAN_POINT ( 'NONE',  ( 27.00000000000031619, -3.464101615137567869, -1.612499999999994049 ) ) ;
#5772 = CARTESIAN_POINT ( 'NONE',  ( 8.632099005475788900, 83.25231371789854506, -13.23911966647199812 ) ) ;
#5773 = CARTESIAN_POINT ( 'NONE',  ( -31.78794563604516554, 205.3262412349647832, 4.842901733360250205 ) ) ;
#5774 = CIRCLE ( 'NONE', #3370, 1.499999999999990452 ) ;
#5775 = VERTEX_POINT ( 'NONE', #4211 ) ;
#5776 = LINE ( 'NONE', #28523, #7756 ) ;
#5777 = CARTESIAN_POINT ( 'NONE',  ( 6.932735513423970097, 110.7476862821014549, 10.69584247140445044 ) ) ;
#5778 = CARTESIAN_POINT ( 'NONE',  ( -8.632099005475501130, 50.94768628210145067, -13.23911966647218996 ) ) ;
#5779 = AXIS2_PLACEMENT_3D ( 'NONE', #3845, #13319, #24327 ) ;
#5780 = CYLINDRICAL_SURFACE ( 'NONE', #25925, 24.80000000000000426 ) ;
#5781 = CARTESIAN_POINT ( 'NONE',  ( 24.51575785039200284, 0.000000000000000000, 161.8222238355895399 ) ) ;
#5782 = CARTESIAN_POINT ( 'NONE',  ( 15.46528703574804986, 72.79768628210145209, 3.257655550457285720 ) ) ;
#5783 = CARTESIAN_POINT ( 'NONE',  ( 19.68408634441910721, -5.407089921784855591, -9.890624999385533300 ) ) ;
#5784 = CARTESIAN_POINT ( 'NONE',  ( 14.99999999999992184, 3.464101615137706425, -4.087499999999989697 ) ) ;
#5785 = CARTESIAN_POINT ( 'NONE',  ( -44.65997103062156981, 215.5714017266979852, 3.350049139982118618 ) ) ;
#5786 = CARTESIAN_POINT ( 'NONE',  ( 18.00000000000000000, 249.0250000000000057, -5.196152422706630247 ) ) ;
#5787 = CARTESIAN_POINT ( 'NONE',  ( 8.715434833791931624, 46.06018628210144072, 8.962234695871760692 ) ) ;
#5788 = CARTESIAN_POINT ( 'NONE',  ( -1.926257025242585782E-15, 199.7468750006145513, -31.45816453501075927 ) ) ;
#5789 = CARTESIAN_POINT ( 'NONE',  ( 28.08117253353866971, 5.196152422706630247, 165.3593121602424674 ) ) ;
#5790 = CARTESIAN_POINT ( 'NONE',  ( 3.796722387233379514, 6.385186282101440902, -8.710071997420127943 ) ) ;
#5791 = CARTESIAN_POINT ( 'NONE',  ( 20.99999999999999645, 248.1718750006145342, 6.646953231504538984 ) ) ;
#5792 = ORIENTED_EDGE ( 'NONE', *, *, #36303, .F. ) ;
#5793 = CARTESIAN_POINT ( 'NONE',  ( 18.00000000000000000, 5.196152422706630247, -5.025000000000002132 ) ) ;
#5794 = CARTESIAN_POINT ( 'NONE',  ( 15.00000000000000000, 0.000000000000000000, -3.149999999999986144 ) ) ;
#5795 = CARTESIAN_POINT ( 'NONE',  ( 30.58849351077567036, -7.209453229046482114, 159.5969823328619555 ) ) ;
#5796 = CARTESIAN_POINT ( 'NONE',  ( 19.68408634441910721, 5.407089921784857367, -3.890624999385555505 ) ) ;
#5797 = CARTESIAN_POINT ( 'NONE',  ( 31.35818766391586365, 7.209453229046475009, 168.3946267603846820 ) ) ;
#5798 = CARTESIAN_POINT ( 'NONE',  ( 23.99999999999999645, 241.3000000000000114, -5.196152422706631135 ) ) ;
#5799 = DIRECTION ( 'NONE',  ( 0.000000000000000000, 0.000000000000000000, 1.000000000000000000 ) ) ;
#5800 = CARTESIAN_POINT ( 'NONE',  ( -10.49813415415989404, 59.57268628210145778, -7.228626920339069173 ) ) ;
#5801 = ORIENTED_EDGE ( 'NONE', *, *, #19380, .T. ) ;
#5802 = ORIENTED_EDGE ( 'NONE', *, *, #27416, .F. ) ;
#5803 = CARTESIAN_POINT ( 'NONE',  ( 37.18092677073180141, 7.347880794884125653E-16, 166.1065598226053055 ) ) ;
#5804 = CARTESIAN_POINT ( 'NONE',  ( 5.727106289114498080E-15, 195.7250000012290343, 31.17691453623979214 ) ) ;
#5805 = FACE_OUTER_BOUND ( 'NONE', #34773, .T. ) ;
#5806 = CARTESIAN_POINT ( 'NONE',  ( 15.24356964374999990, 0.000000000000000000, -6.890624999385474680 ) ) ;
#5807 = PRODUCT_DEFINITION_CONTEXT ( 'detailed design', #32784, 'design' ) ;
#5808 = CARTESIAN_POINT ( 'NONE',  ( -5.770363421894122880, 41.56481371789855217, 14.38691631536194393 ) ) ;
#5809 = CARTESIAN_POINT ( 'NONE',  ( 37.02404643378602600, 7.347880794884125653E-16, 164.3134093660401618 ) ) ;
#5810 = CIRCLE ( 'NONE', #13102, 6.000000000000005329 ) ;
#5811 = CARTESIAN_POINT ( 'NONE',  ( 21.00000000000000000, 241.1968750006145399, -6.646953231504538984 ) ) ;
#5812 = CARTESIAN_POINT ( 'NONE',  ( -39.90997103062156270, 213.8393509191290889, 2.350049139982164359 ) ) ;
#5813 = DIRECTION ( 'NONE',  ( 0.000000000000000000, 0.000000000000000000, 1.000000000000000000 ) ) ;
#5814 = CARTESIAN_POINT ( 'NONE',  ( 25.37693404997765256, -3.464101615137757051, 168.8708645910097346 ) ) ;
#5815 = CARTESIAN_POINT ( 'NONE',  ( -1.715153634034442431, 22.87731371789854151, 9.534712964251900402 ) ) ;
#5816 = CARTESIAN_POINT ( 'NONE',  ( -59.10788769728823411, 216.4690446883607535, 1.857196546604031662 ) ) ;
#5817 = APPLICATION_PROTOCOL_DEFINITION ( 'draft international standard', 'automotive_design', 1998, #17071 ) ;
#5818 = PRODUCT_RELATED_PRODUCT_CATEGORY ( 'part', '', ( #34976 ) ) ;
#5819 = CARTESIAN_POINT ( 'NONE',  ( 26.61936306680777875, 195.0000000000000000, 5.364276260378865402 ) ) ;
#5820 = CARTESIAN_POINT ( 'NONE',  ( -13.62178482187500528, 196.6343750006145399, -23.59362340125807123 ) ) ;
#5821 = CARTESIAN_POINT ( 'NONE',  ( 3.257655550456945548, 123.5023137178985451, 15.46528703574811736 ) ) ;
#5822 = AXIS2_PLACEMENT_3D ( 'NONE', #13334, #18853, #7838 ) ;
#5823 = ORIENTED_EDGE ( 'NONE', *, *, #13538, .T. ) ;
#5824 = CARTESIAN_POINT ( 'NONE',  ( 10.69584247140445221, 44.04768628210144499, -6.932735513423970097 ) ) ;
#5825 = CARTESIAN_POINT ( 'NONE',  ( 22.56230152254310894, -3.464101615138333923, -8.249999998771022192 ) ) ;
#5826 = EDGE_CURVE ( 'NONE', #27950, #35077, #28466, .T. ) ;
#5827 = DIRECTION ( 'NONE',  ( 1.000000000000000000, 0.000000000000000000, 0.000000000000000000 ) ) ;
#5828 = CARTESIAN_POINT ( 'NONE',  ( 24.43895185209563792, 3.604726614523236616, 160.9443272578961626 ) ) ;
#5829 = CARTESIAN_POINT ( 'NONE',  ( 26.99999999999999645, 3.464101615137755275, -3.281249998770945808 ) ) ;
#5830 = CARTESIAN_POINT ( 'NONE',  ( 19.68408634441911786, -5.407089921784861808, -8.596874999385523353 ) ) ;
#5831 = CARTESIAN_POINT ( 'NONE',  ( 24.61867908796596183, 0.000000000000000000, 160.2039707163872038 ) ) ;
#5832 =( BOUNDED_CURVE ( )  B_SPLINE_CURVE ( 2, ( #18866, #12786, #35709, #1404, #36269, #33435, #7476 ),
 .UNSPECIFIED., .F., .F. ) 
 B_SPLINE_CURVE_WITH_KNOTS ( ( 3, 2, 2, 3 ),
 ( 0.7826086956521763893, 0.7898550724637706244, 0.7971014492753649705, 0.8043478260869593166 ),
 .UNSPECIFIED. ) 
 CURVE ( )  GEOMETRIC_REPRESENTATION_ITEM ( )  RATIONAL_B_SPLINE_CURVE ( ( 0.9999999999999548139, 0.8660254037844838937, 1.000000000000000000, 0.8660254037844387076, 1.000000000000000000, 0.8660254037843874153, 1.000000000000051292 ) ) 
 REPRESENTATION_ITEM ( '' )  );
#5833 = CARTESIAN_POINT ( 'NONE',  ( 2.064181346179272847, 70.49768628210145494, -9.465287035748065847 ) ) ;
#5834 = DIRECTION ( 'NONE',  ( -0.000000000000000000, -1.000000000000000000, -0.000000000000000000 ) ) ;
#5835 = CYLINDRICAL_SURFACE ( 'NONE', #2084, 5.999999999999994671 ) ;
#5836 = CARTESIAN_POINT ( 'NONE',  ( 12.46528703574805874, 91.19768628210145778, 2.660918448318279950 ) ) ;
#5837 = CARTESIAN_POINT ( 'NONE',  ( 0.000000000000000000, 143.0000000000000000, 0.000000000000000000 ) ) ;
#5838 = CARTESIAN_POINT ( 'NONE',  ( 27.00000000000001421, 198.5000000012290684, 15.58845726811988897 ) ) ;
#5839 = ORIENTED_EDGE ( 'NONE', *, *, #36547, .T. ) ;
#5840 = CARTESIAN_POINT ( 'NONE',  ( 27.71554269823568362, -5.407089921784859143, 162.5774681431477404 ) ) ;
#5841 = CARTESIAN_POINT ( 'NONE',  ( 23.87821517812500005, -4.985214923628404016, -8.090624999385454430 ) ) ;
#5842 = CARTESIAN_POINT ( 'NONE',  ( 13.62178482187501416, 196.4093750006145456, 23.59362340125806767 ) ) ;
#5843 = CARTESIAN_POINT ( 'NONE',  ( 28.28586808984062628, 5.407089921784862696, 169.0963171987856128 ) ) ;
#5844 = CARTESIAN_POINT ( 'NONE',  ( 37.05999817766942783, -3.464101615137755275, 164.7243396790030090 ) ) ;
#5845 = DIRECTION ( 'NONE',  ( 0.08715574274765150453, 0.000000000000000000, 0.9961946980917461003 ) ) ;
#5846 = CARTESIAN_POINT ( 'NONE',  ( 26.99999999999999645, 248.9125000000000227, -3.464101615137755275 ) ) ;
#5847 = CARTESIAN_POINT ( 'NONE',  ( 5.778771075727756162E-15, 199.4656250006145797, 31.45816453501076637 ) ) ;
#5848 = CARTESIAN_POINT ( 'NONE',  ( -4.944772684328424539, 118.6148137178985564, -11.48171059495408031 ) ) ;
#5849 = CARTESIAN_POINT ( 'NONE',  ( 2.311890736173175753, 129.7226862821014493, 12.53471296425194659 ) ) ;
#5851 = ORIENTED_EDGE ( 'NONE', *, *, #11736, .T. ) ;
#5850 = ORIENTED_EDGE ( 'NONE', *, *, #27087, .F. ) ;
#5852 = CARTESIAN_POINT ( 'NONE',  ( 27.24356964374999635, 198.7156250006145513, -15.72908226750539029 ) ) ;
#5853 = CARTESIAN_POINT ( 'NONE',  ( 26.75643035624999655, 241.8343750006145001, 3.323476615752267715 ) ) ;
#5854 = FACE_BOUND ( 'NONE', #17149, .T. ) ;
#5855 = CARTESIAN_POINT ( 'NONE',  ( -14.38691631536193860, 89.86481371789855643, -5.770363421894132649 ) ) ;
#5856 = CARTESIAN_POINT ( 'NONE',  ( 21.00000000000000000, -6.646953231504538984, -3.740624999385479654 ) ) ;
#5857 = CARTESIAN_POINT ( 'NONE',  ( 26.75643035624999655, 246.8968750006145285, 3.323476615752267715 ) ) ;
#5858 = CARTESIAN_POINT ( 'NONE',  ( -13.50000000000000533, 196.8875000012290286, -23.38268590217984411 ) ) ;
#5859 = CARTESIAN_POINT ( 'NONE',  ( -5.529263428287297444, 81.52731371789856496, -7.954856959092311719 ) ) ;
#5860 = CARTESIAN_POINT ( 'NONE',  ( 13.44051670066911264, 5.407089921784856479, -3.365624999385530280 ) ) ;
#5861 = CARTESIAN_POINT ( 'NONE',  ( 20.99999999999999645, 242.4343750006145228, -6.646953231504538984 ) ) ;
#5862 = CARTESIAN_POINT ( 'NONE',  ( 12.50000000000000355, 47.88981371789854791, -0.1745138560722771515 ) ) ;
#5863 = CARTESIAN_POINT ( 'NONE',  ( 22.60769515458672529, 246.7736538117967200, -6.000000000000004441 ) ) ;
#5864 = CARTESIAN_POINT ( 'NONE',  ( 0.1745138560725515708, 107.0101862821014578, -12.50000000000000355 ) ) ;
#5865 = CARTESIAN_POINT ( 'NONE',  ( 10.56230152254410903, 3.464101615137752166, -3.524999998771006560 ) ) ;
#5866 = CARTESIAN_POINT ( 'NONE',  ( -35.15997103062156270, 215.5714017266979852, 3.350049139982118618 ) ) ;
#5867 = CARTESIAN_POINT ( 'NONE',  ( 19.95811700914455500, 239.9653672772770392, -5.908847589363869446 ) ) ;
#5868 = CARTESIAN_POINT ( 'NONE',  ( -27.00000000000000355, 198.7625000012290286, 0.000000000000000000 ) ) ;
#5869 = CARTESIAN_POINT ( 'NONE',  ( -6.092822981423970496, 102.9851862821014805, 14.25334919248782661 ) ) ;
#5870 = AXIS2_PLACEMENT_3D ( 'NONE', #12967, #15624, #3866 ) ;
#5871 = CARTESIAN_POINT ( 'NONE',  ( 12.53471296425194659, 7.822686282101448896, -2.311890736173178418 ) ) ;
#5872 = CARTESIAN_POINT ( 'NONE',  ( 27.95370725966311554, 5.196152422706636465, 163.9023774130589288 ) ) ;
#5873 = DIRECTION ( 'NONE',  ( -1.000000000000000000, -6.123233995736766036E-17, 0.000000000000000000 ) ) ;
#5874 = CARTESIAN_POINT ( 'NONE',  ( -8.152565276336710909, 131.4476862821014436, 5.233372021372435512 ) ) ;
#5875 = DIRECTION ( 'NONE',  ( -0.000000000000000000, -0.000000000000000000, 1.000000000000000000 ) ) ;
#5876 = CARTESIAN_POINT ( 'NONE',  ( 26.75643035624999655, 242.3218750006145399, -7.049594010296217766E-16 ) ) ;
#5877 = ORIENTED_EDGE ( 'NONE', *, *, #30573, .T. ) ;
#5878 = DIRECTION ( 'NONE',  ( 1.000000000000000000, 0.000000000000000000, 0.000000000000000000 ) ) ;
#5879 = CARTESIAN_POINT ( 'NONE',  ( 9.465287035748067623, 63.59768628210142793, 2.064181346179272847 ) ) ;
#5880 = CARTESIAN_POINT ( 'NONE',  ( 23.87821517812499650, 4.985214923628404904, -1.190624999385464511 ) ) ;
#5881 = DIRECTION ( 'NONE',  ( 0.000000000000000000, 0.000000000000000000, 1.000000000000000000 ) ) ;
#5882 = DIRECTION ( 'NONE',  ( 0.000000000000000000, 0.000000000000000000, 1.000000000000000000 ) ) ;
#5883 = CARTESIAN_POINT ( 'NONE',  ( 27.24356964374999635, 196.0718750006145683, -15.72908226750539029 ) ) ;
#5884 = CARTESIAN_POINT ( 'NONE',  ( 24.00000000000000000, 246.1000000000000227, 5.196152422706629359 ) ) ;
#5885 = EDGE_CURVE ( 'NONE', #4551, #972, #7440, .T. ) ;
#5886 = CYLINDRICAL_SURFACE ( 'NONE', #9092, 6.000000000000001776 ) ;
#5887 = CARTESIAN_POINT ( 'NONE',  ( 8.152565276336593669, 39.55231371789854933, 5.233372021372610483 ) ) ;
#5888 = CARTESIAN_POINT ( 'NONE',  ( -1.926257025242585782E-15, 199.7468750006145513, -31.45816453501076637 ) ) ;
#5889 = ORIENTED_EDGE ( 'NONE', *, *, #4516, .T. ) ;
#5890 = ORIENTED_EDGE ( 'NONE', *, *, #6458, .F. ) ;
#5891 =( BOUNDED_CURVE ( )  B_SPLINE_CURVE ( 2, ( #23506, #25781, #2841, #20297, #29173, #36636, #34499 ),
 .UNSPECIFIED., .F., .F. ) 
 B_SPLINE_CURVE_WITH_KNOTS ( ( 3, 2, 2, 3 ),
 ( 0.02173913043478289606, 0.02898550724637719705, 0.03623188405797149458, 0.04347826086956579211 ),
 .UNSPECIFIED. ) 
 CURVE ( )  GEOMETRIC_REPRESENTATION_ITEM ( )  RATIONAL_B_SPLINE_CURVE ( ( 0.9999999999999946709, 0.8660254037844440367, 1.000000000000000000, 0.8660254037844387076, 1.000000000000000000, 0.8660254037844280495, 1.000000000000010658 ) ) 
 REPRESENTATION_ITEM ( '' )  );
#5892 = CARTESIAN_POINT ( 'NONE',  ( 21.00000000000000000, 248.5093750006144830, 6.646953231504538984 ) ) ;
#5893 = CARTESIAN_POINT ( 'NONE',  ( 12.46528703574811558, 47.60231371789855359, -2.660918448318005947 ) ) ;
#5894 = CARTESIAN_POINT ( 'NONE',  ( 10.31873187879410558, 0.000000000000000000, -8.746874999385534366 ) ) ;
#5895 = CARTESIAN_POINT ( 'NONE',  ( 18.12178482187499640, 4.985214923628404904, -9.778124999385489957 ) ) ;
#5896 = CARTESIAN_POINT ( 'NONE',  ( 4.622313124798831829, 9.364813717898545775, -11.61527771782809282 ) ) ;
#5897 = ORIENTED_EDGE ( 'NONE', *, *, #34903, .T. ) ;
#5898 = CARTESIAN_POINT ( 'NONE',  ( 10.31873187879410381, 3.604726614523240613, -4.734374999385511096 ) ) ;
#5899 = CARTESIAN_POINT ( 'NONE',  ( 20.99999999999997513, 245.8937500012290798, -5.999999999999999112 ) ) ;
#5900 = CARTESIAN_POINT ( 'NONE',  ( 28.08976766865841057, 5.407089921784862696, 166.8548791280792045 ) ) ;
#5901 = CARTESIAN_POINT ( 'NONE',  ( -35.15252896937850124, 206.6499508600178387, -5.571401726697954970 ) ) ;
#5902 = CARTESIAN_POINT ( 'NONE',  ( 15.00000000000000178, 245.5937500012290400, 3.464101615137757051 ) ) ;
#5903 = ADVANCED_FACE ( 'NONE', ( #24316 ), #36604, .T. ) ;
#5904 = CARTESIAN_POINT ( 'NONE',  ( -26.80567346611835333, 195.0000000000000853, 4.049898097028912680 ) ) ;
#5905 = CARTESIAN_POINT ( 'NONE',  ( -63.85044563604516554, 206.6211998817775566, -3.209657149897419348 ) ) ;
#5906 = CARTESIAN_POINT ( 'NONE',  ( -36.34747103062156981, 213.3500491399821328, -5.571401726697985168 ) ) ;
#5907 = CARTESIAN_POINT ( 'NONE',  ( 25.14818170870464797, 0.000000000000000000, 169.0508616136177409 ) ) ;
#5908 = VERTEX_POINT ( 'NONE', #30570 ) ;
#5909 = CYLINDRICAL_SURFACE ( 'NONE', #25789, 5.999999999999998224 ) ;
#5910 = CARTESIAN_POINT ( 'NONE',  ( 4.999999999999997335, 216.0000000000000000, 7.347880794884120722E-16 ) ) ;
#5911 = CARTESIAN_POINT ( 'NONE',  ( -10.83675517735179028, 23.73981371789854222, 11.08355503943118947 ) ) ;
#5912 = CARTESIAN_POINT ( 'NONE',  ( -54.75372103062156270, 218.5309553116391896, -2.162041339862839084 ) ) ;
#5913 = CARTESIAN_POINT ( 'NONE',  ( -6.932735513423968321, 4.947686282101432909, -10.69584247140445221 ) ) ;
#5914 = CARTESIAN_POINT ( 'NONE',  ( 12.50000000000000355, 54.11018628210144499, 0.1745138560725507937 ) ) ;
#5915 = CARTESIAN_POINT ( 'NONE',  ( 13.56230152254411792, -5.196152422706638241, -3.975000000000061817 ) ) ;
#5916 = VERTEX_POINT ( 'NONE', #4587 ) ;
#5917 = CARTESIAN_POINT ( 'NONE',  ( -37.53497103062156981, 204.4285982733020148, -3.350049139982115509 ) ) ;
#5918 = DIRECTION ( 'NONE',  ( 1.000000000000000000, 0.000000000000000000, 0.000000000000000000 ) ) ;
#5919 = CARTESIAN_POINT ( 'NONE',  ( 13.62178482187501416, 196.8593750006145342, 23.59362340125806767 ) ) ;
#5920 = DIRECTION ( 'NONE',  ( -0.000000000000000000, -0.000000000000000000, -1.000000000000000000 ) ) ;
#5921 = CARTESIAN_POINT ( 'NONE',  ( 26.99999999999999645, 7.347880794884117764E-16, -4.218749998770948473 ) ) ;
#5922 = DIRECTION ( 'NONE',  ( 0.000000000000000000, 1.000000000000000000, 0.000000000000000000 ) ) ;
#5923 = CARTESIAN_POINT ( 'NONE',  ( -44.35000000000001563, 244.5000000000000000, 2.500000000000000000 ) ) ;
#5924 = CARTESIAN_POINT ( 'NONE',  ( 26.75643035624999655, 245.9968750006145513, 3.323476615752267715 ) ) ;
#5925 = CARTESIAN_POINT ( 'NONE',  ( -6.594114490232462877, 97.33981371789856496, 6.840914352311949109 ) ) ;
#5926 = CARTESIAN_POINT ( 'NONE',  ( 15.24356964374999990, 239.9218750006145626, -3.323476615752268604 ) ) ;
#5927 = CIRCLE ( 'NONE', #9568, 7.500000000000000000 ) ;
#5928 = ORIENTED_EDGE ( 'NONE', *, *, #6629, .T. ) ;
#5929 = CARTESIAN_POINT ( 'NONE',  ( -60.69122103062155560, 208.3738570449993404, -6.530955311639226935 ) ) ;
#5930 = CARTESIAN_POINT ( 'NONE',  ( 4.999999999999997335, 216.0000000000000000, 7.347880794884120722E-16 ) ) ;
#5931 = CARTESIAN_POINT ( 'NONE',  ( 21.00000000000000000, 247.0187500012290513, 6.928203230275506996 ) ) ;
#5932 = VERTEX_POINT ( 'NONE', #27712 ) ;
#5933 = CARTESIAN_POINT ( 'NONE',  ( 11.48171059495408208, 102.5148137178985621, -4.944772684328420986 ) ) ;
#5934 = CARTESIAN_POINT ( 'NONE',  ( 22.80587116629411426, 7.646167579472024665E-16, -1.771874999385525395 ) ) ;
#5935 = CARTESIAN_POINT ( 'NONE',  ( 30.63261610554165770, -7.209453229046475009, 160.1013058987709030 ) ) ;
#5936 =( BOUNDED_SURFACE ( )  B_SPLINE_SURFACE ( 1, 2, ( 
 ( #37338, #26344, #22775, #35062, #6263, #28996, #11388, #8548, #17088, #26532, #34508, #34323, #19940, #8735, #8369, #11572, #14240, #29184, #20306, #5691, #20114, #14799, #3226, #34878, #28811, #31479, #3038, #31847, #5880, #2848, #380, #11947, #14609, #26160, #23516, #193, #9112, #20677, #32224, #17841, #29376, #3414, #32411, #29755, #21250, #18400, #35814, #15362, #3786, #9300, #15930, #23896, #12517, #27479, #32789, #20872, #12323, #15550, #6452, #24081, #35626, #18214, #18024, #36003, #26915, #35438, #9856, #6824, #943, #21061, #21435, #9672, #6639, #29949, #27290, #32599, #33169, #3977, #27108, #1132, #29569, #12698, #24270, #32975, #7029, #3606, #12129, #7214, #18595, #15173, #30139, #4169, #15739, #753, #1320, #12888, #24453, #26720, #9485, #10040, #21617, #18786, #30327, #4351, #23705, #35247, #28037, #16677, #31257, #28224, #30520, #2252, #22362, #4540, #4725, #5283, #5098, #16863, #1505, #2069, #1693, #24819, #27848, #16116, #13832, #13081, #25378, #22546, #33725, #27668, #36372, #21805, #24635, #13267, #36186, #10230, #1881, #33358, #13452, #7393, #36748, #16301, #10418, #18966, #31075, #25196, #13643, #21993, #33540, #7767, #25002, #36558, #7580, #33911, #7953, #30885, #10599, #10789, #19156, #30704, #22179, #19346, #4908, #16489, #19528, #36927, #10975, #34095, #8145, #19717, #31621, #20076, #25563, #32184, #2621, #28770, #6218, #37481, #37115, #28583, #31804, #22736, #2810, #14380, #34467, #11163, #14757, #5649, #14197, #14567, #23103, #17232, #37301, #151, #25938, #22922, #11532, #6024, #11350, #11903, #34646, #8691, #20265, #34285, #2997, #26300, #25748, #23290, #20638, #8510, #8328, #338, #5841, #17419, #26119, #28959, #11715, #34835, #8875, #20453, #31995, #17610, #29141, #3181, #23470, #35023, #9067, #28400, #19899, #2438, #14012, #31440, #5462, #17045, #18169, #29710, #12279, #3935, #35205, #33128, #12846, #12471, #23661, #24225, #24039, #18357, #6407, #21018, #15510, #1090, #20827, #9254, #12660, #3744, #9440, #35771, #32552, #32368, #520, #6783, #32934, #10000, #6987, #17980, #18556, #9815, #29524, #6595, #21581 ),
 ( #21392, #17791, #30096, #1275, #35584, #3564, #15126, #12087, #29334, #26677, #3371, #14941, #15317, #26488, #26870, #708, #27065, #900, #23853, #35391, #4129, #15701, #29906, #9629, #21206, #32746, #27252, #24413, #35962, #27995, #13603, #36518, #21952, #33685, #22508, #7171, #30665, #19115, #18744, #33497, #36331, #27434, #24780, #16264, #13412, #30846, #10377, #7543, #4311, #10933, #18928, #4682, #30285, #27814, #15890, #7356, #10562, #1467, #1842, #24960, #4870, #2025, #10190, #24596, #25153, #22139, #7725, #36708, #19308, #13041, #36147, #16450, #22320, #36887, #33872, #21766, #7913, #10747, #33316, #19487, #30480, #31034, #4501, #16078, #5055, #27627, #1657, #16638, #13231, #28179, #2210, #13791, #25339, #28727, #11120, #19857, #16820, #289, #8284, #8101, #31214, #34426, #11855, #22875, #28362, #31763, #37259, #5419, #2398, #26076, #20215, #23058, #34241, #26254, #2765, #8463, #31578, #13972, #17373, #2950, #25891, #11307, #34604, #34055, #19675, #20033, #5601, #5243, #17187, #25707, #25521, #14153, #14337, #37440, #5793, #11489, #8646, #37074, #22697, #31400, #28914, #17000, #14520, #28540, #2583, #104, #11668, #23243, #34790, #8834, #20406, #31947, #5979, #17560, #29094, #3137, #14705, #32319, #32693, #9395, #17931, #23801, #1038, #6360, #6931, #35339, #20969, #32502, #29284, #35536, #21344, #9206, #18309, #15647, #6548, #18121, #29475, #9581, #3323, #1747, #18502, #29664, #14894, #29849, #3699, #23992, #12042, #26629, #12421, #21155, #32883, #3885, #6736, #15459, #27011, #15267, #26820, #850, #27717, #12609, #24175, #35720, #9767, #30041, #4075, #3511, #23424, #34975, #9018, #20589, #32131, #6169, #17743, #20775, #658, #12229, #26442, #15079, #474, #23610, #35155, #2305, #37169, #25429, #2117, #36795, #8002, #28085, #22228, #17095, #36982, #22782, #25056, #16725, #13694, #10650, #34331, #11025, #34145, #19575, #33960, #13881, #19207, #19767, #5511, #31487, #31305, #28634, #5332, #24872, #33593, #11209, #31127, #25244, #16350, #13314, #10838, #16910, #33779, #14063, #19947, #7818, #5144, #28271, #22412, #22599, #30754, #19395, #8192 ) ),
 .UNSPECIFIED., .F., .F., .F. ) 
 B_SPLINE_SURFACE_WITH_KNOTS ( ( 2, 2 ),
 ( 3, 2, 2, 2, 2, 2, 2, 2, 2, 2, 2, 2, 2, 2, 2, 2, 2, 2, 2, 2, 2, 2, 2, 2, 2, 2, 2, 2, 2, 2, 2, 2, 2, 2, 2, 2, 2, 2, 2, 2, 2, 2, 2, 2, 2, 2, 2, 2, 2, 2, 2, 2, 2, 2, 2, 2, 2, 2, 2, 2, 2, 2, 2, 2, 2, 2, 2, 2, 2, 2, 2, 2, 2, 2, 2, 2, 2, 2, 2, 2, 2, 2, 2, 2, 2, 2, 2, 2, 2, 2, 2, 2, 2, 2, 2, 2, 2, 2, 2, 2, 2, 2, 2, 2, 2, 2, 2, 2, 2, 2, 2, 2, 2, 2, 2, 2, 2, 2, 2, 2, 2, 2, 2, 2, 2, 2, 2, 2, 2, 2, 2, 2, 2, 2, 3 ),
 ( 0.000000000000000000, 1.000000000000000000 ),
 ( 0.000000000000000000, 0.007246376811594202987, 0.01449275362318840597, 0.02173913043478260809, 0.02898550724637681195, 0.03623188405797101580, 0.04347826086956521618, 0.05072463768115942351, 0.05797101449275362389, 0.06521739130434782428, 0.07246376811594203160, 0.07971014492753622505, 0.08695652173913043237, 0.09420289855072463969, 0.1014492753623188470, 0.1086956521739130405, 0.1159420289855072478, 0.1231884057971014551, 0.1304347826086956486, 0.1376811594202898559, 0.1449275362318840632, 0.1521739130434782705, 0.1594202898550724501, 0.1666666666666666574, 0.1739130434782608647, 0.1811594202898550721, 0.1884057971014492794, 0.1956521739130434867, 0.2028985507246376940, 0.2101449275362318736, 0.2173913043478260809, 0.2246376811594202882, 0.2318840579710144956, 0.2391304347826087029, 0.2463768115942029102, 0.2536231884057971175, 0.2608695652173912971, 0.2681159420289855322, 0.2753623188405797118, 0.2826086956521738913, 0.2898550724637681264, 0.2971014492753623060, 0.3043478260869565410, 0.3115942028985507206, 0.3188405797101449002, 0.3260869565217391353, 0.3333333333333333148, 0.3405797101449275499, 0.3478260869565217295, 0.3550724637681159646, 0.3623188405797101441, 0.3695652173913043237, 0.3768115942028985588, 0.3840579710144927383, 0.3913043478260869734, 0.3985507246376811530, 0.4057971014492753881, 0.4130434782608695676, 0.4202898550724637472, 0.4275362318840579823, 0.4347826086956521618, 0.4420289855072463969, 0.4492753623188405765, 0.4565217391304347561, 0.4637681159420289911, 0.4710144927536231707, 0.4782608695652174058, 0.4855072463768115854, 0.4927536231884058204, 0.5000000000000000000, 0.5072463768115942351, 0.5144927536231883591, 0.5217391304347825942, 0.5289855072463768293, 0.5362318840579710644, 0.5434782608695651884, 0.5507246376811594235, 0.5579710144927536586, 0.5652173913043477826, 0.5724637681159420177, 0.5797101449275362528, 0.5869565217391304879, 0.5942028985507246119, 0.6014492753623188470, 0.6086956521739130821, 0.6159420289855072062, 0.6231884057971014412, 0.6304347826086956763, 0.6376811594202898004, 0.6449275362318840354, 0.6521739130434782705, 0.6594202898550725056, 0.6666666666666666297, 0.6739130434782608647, 0.6811594202898550998, 0.6884057971014492239, 0.6956521739130434590, 0.7028985507246376940, 0.7101449275362319291, 0.7173913043478260532, 0.7246376811594202882, 0.7318840579710145233, 0.7391304347826086474, 0.7463768115942028825, 0.7536231884057971175, 0.7608695652173913526, 0.7681159420289854767, 0.7753623188405797118, 0.7826086956521739468, 0.7898550724637680709, 0.7971014492753623060, 0.8043478260869565410, 0.8115942028985507761, 0.8188405797101449002, 0.8260869565217391353, 0.8333333333333333703, 0.8405797101449274944, 0.8478260869565217295, 0.8550724637681159646, 0.8623188405797101996, 0.8695652173913043237, 0.8768115942028985588, 0.8840579710144927938, 0.8913043478260869179, 0.8985507246376811530, 0.9057971014492753881, 0.9130434782608695121, 0.9202898550724637472, 0.9275362318840579823, 0.9347826086956522174, 0.9420289855072463414, 0.9492753623188405765, 0.9565217391304348116, 0.9637681159420289356, 0.9662082973083874204 ),
 .UNSPECIFIED. ) 
 GEOMETRIC_REPRESENTATION_ITEM ( )  RATIONAL_B_SPLINE_SURFACE ( (
 ( 1.000000000000000000, 0.8660254037844387076, 1.000000000000000000, 0.8660254037844387076, 1.000000000000000000, 0.8660254037844387076, 1.000000000000000000, 0.8660254037844387076, 1.000000000000000000, 0.8660254037844387076, 1.000000000000000000, 0.8660254037844387076, 1.000000000000000000, 0.8660254037844387076, 1.000000000000000000, 0.8660254037844387076, 1.000000000000000000, 0.8660254037844387076, 1.000000000000000000, 0.8660254037844387076, 1.000000000000000000, 0.8660254037844387076, 1.000000000000000000, 0.8660254037844387076, 1.000000000000000000, 0.8660254037844387076, 1.000000000000000000, 0.8660254037844387076, 1.000000000000000000, 0.8660254037844387076, 1.000000000000000000, 0.8660254037844387076, 1.000000000000000000, 0.8660254037844387076, 1.000000000000000000, 0.8660254037844387076, 1.000000000000000000, 0.8660254037844387076, 1.000000000000000000, 0.8660254037844387076, 1.000000000000000000, 0.8660254037844387076, 1.000000000000000000, 0.8660254037844387076, 1.000000000000000000, 0.8660254037844387076, 1.000000000000000000, 0.8660254037844387076, 1.000000000000000000, 0.8660254037844387076, 1.000000000000000000, 0.8660254037844387076, 1.000000000000000000, 0.8660254037844387076, 1.000000000000000000, 0.8660254037844387076, 1.000000000000000000, 0.8660254037844387076, 1.000000000000000000, 0.8660254037844387076, 1.000000000000000000, 0.8660254037844387076, 1.000000000000000000, 0.8660254037844387076, 1.000000000000000000, 0.8660254037844387076, 1.000000000000000000, 0.8660254037844387076, 1.000000000000000000, 0.8660254037844387076, 1.000000000000000000, 0.8660254037844387076, 1.000000000000000000, 0.8660254037844387076, 1.000000000000000000, 0.8660254037844387076, 1.000000000000000000, 0.8660254037844387076, 1.000000000000000000, 0.8660254037844387076, 1.000000000000000000, 0.8660254037844387076, 1.000000000000000000, 0.8660254037844387076, 1.000000000000000000, 0.8660254037844387076, 1.000000000000000000, 0.8660254037844387076, 1.000000000000000000, 0.8660254037844387076, 1.000000000000000000, 0.8660254037844387076, 1.000000000000000000, 0.8660254037844387076, 1.000000000000000000, 0.8660254037844387076, 1.000000000000000000, 0.8660254037844387076, 1.000000000000000000, 0.8660254037844387076, 1.000000000000000000, 0.8660254037844387076, 1.000000000000000000, 0.8660254037844387076, 1.000000000000000000, 0.8660254037844387076, 1.000000000000000000, 0.8660254037844387076, 1.000000000000000000, 0.8660254037844387076, 1.000000000000000000, 0.8660254037844387076, 1.000000000000000000, 0.8660254037844387076, 1.000000000000000000, 0.8660254037844387076, 1.000000000000000000, 0.8660254037844387076, 1.000000000000000000, 0.8660254037844387076, 1.000000000000000000, 0.8660254037844387076, 1.000000000000000000, 0.8660254037844387076, 1.000000000000000000, 0.8660254037844387076, 1.000000000000000000, 0.8660254037844387076, 1.000000000000000000, 0.8660254037844387076, 1.000000000000000000, 0.8660254037844387076, 1.000000000000000000, 0.8660254037844387076, 1.000000000000000000, 0.8660254037844387076, 1.000000000000000000, 0.8660254037844387076, 1.000000000000000000, 0.8660254037844387076, 1.000000000000000000, 0.8660254037844387076, 1.000000000000000000, 0.8660254037844387076, 1.000000000000000000, 0.8660254037844387076, 1.000000000000000000, 0.8660254037844387076, 1.000000000000000000, 0.8660254037844387076, 1.000000000000000000, 0.8660254037844387076, 1.000000000000000000, 0.8660254037844387076, 1.000000000000000000, 0.8660254037844387076, 1.000000000000000000, 0.8660254037844387076, 1.000000000000000000, 0.8660254037844387076, 1.000000000000000000, 0.8660254037844387076, 1.000000000000000000, 0.8660254037844387076, 1.000000000000000000, 0.8660254037844387076, 1.000000000000000000, 0.8660254037844387076, 1.000000000000000000, 0.8660254037844387076, 1.000000000000000000, 0.8660254037844387076, 1.000000000000000000, 0.8660254037844387076, 1.000000000000000000, 0.8660254037844387076, 1.000000000000000000, 0.8660254037844387076, 1.000000000000000000, 0.8660254037844387076, 1.000000000000000000, 0.8660254037844387076, 1.000000000000000000, 0.8660254037844387076, 1.000000000000000000, 0.8660254037844387076, 1.000000000000000000, 0.8660254037844387076, 1.000000000000000000, 0.8660254037844387076, 1.000000000000000000, 0.8660254037844387076, 1.000000000000000000, 0.8660254037844387076, 1.000000000000000000, 0.8660254037844387076, 1.000000000000000000, 0.8660254037844387076, 1.000000000000000000, 0.8660254037844387076, 1.000000000000000000, 0.8660254037844387076, 1.000000000000000000, 0.8660254037844387076, 1.000000000000000000, 0.8660254037844387076, 1.000000000000000000, 0.8660254037844387076, 1.000000000000000000, 0.8660254037844387076, 1.000000000000000000, 0.8660254037844387076, 1.000000000000000000, 0.8660254037844387076, 1.000000000000000000, 0.8660254037844387076, 1.000000000000000000, 0.8660254037844387076, 1.000000000000000000, 0.8660254037844387076, 1.000000000000000000, 0.8660254037844387076, 1.000000000000000000, 0.8660254037844387076, 1.000000000000000000, 0.8660254037844387076, 1.000000000000000000, 0.8660254037844387076, 1.000000000000000000, 0.8660254037844387076, 1.000000000000000000, 0.8660254037844387076, 1.000000000000000000, 0.8660254037844387076, 1.000000000000000000, 0.8660254037844387076, 1.000000000000000000, 0.8660254037844387076, 1.000000000000000000, 0.8660254037844387076, 1.000000000000000000, 0.8660254037844387076, 1.000000000000000000, 0.8660254037844387076, 1.000000000000000000, 0.8660254037844387076, 1.000000000000000000, 0.8660254037844387076, 1.000000000000000000, 0.8660254037844387076, 1.000000000000000000, 0.8660254037844387076, 1.000000000000000000, 0.8660254037844387076, 1.000000000000000000, 0.8660254037844387076, 1.000000000000000000, 0.8660254037844387076, 1.000000000000000000, 0.8660254037844387076, 1.000000000000000000, 0.8660254037844387076, 1.000000000000000000, 0.8660254037844387076, 1.000000000000000000, 0.8660254037844387076, 1.000000000000000000, 0.9548847207714155072, 0.9401541335272467492),
 ( 1.000000000000000000, 0.8660254037844387076, 1.000000000000000000, 0.8660254037844387076, 1.000000000000000000, 0.8660254037844387076, 1.000000000000000000, 0.8660254037844387076, 1.000000000000000000, 0.8660254037844387076, 1.000000000000000000, 0.8660254037844387076, 1.000000000000000000, 0.8660254037844387076, 1.000000000000000000, 0.8660254037844387076, 1.000000000000000000, 0.8660254037844387076, 1.000000000000000000, 0.8660254037844387076, 1.000000000000000000, 0.8660254037844387076, 1.000000000000000000, 0.8660254037844387076, 1.000000000000000000, 0.8660254037844387076, 1.000000000000000000, 0.8660254037844387076, 1.000000000000000000, 0.8660254037844387076, 1.000000000000000000, 0.8660254037844387076, 1.000000000000000000, 0.8660254037844387076, 1.000000000000000000, 0.8660254037844387076, 1.000000000000000000, 0.8660254037844387076, 1.000000000000000000, 0.8660254037844387076, 1.000000000000000000, 0.8660254037844387076, 1.000000000000000000, 0.8660254037844387076, 1.000000000000000000, 0.8660254037844387076, 1.000000000000000000, 0.8660254037844387076, 1.000000000000000000, 0.8660254037844387076, 1.000000000000000000, 0.8660254037844387076, 1.000000000000000000, 0.8660254037844387076, 1.000000000000000000, 0.8660254037844387076, 1.000000000000000000, 0.8660254037844387076, 1.000000000000000000, 0.8660254037844387076, 1.000000000000000000, 0.8660254037844387076, 1.000000000000000000, 0.8660254037844387076, 1.000000000000000000, 0.8660254037844387076, 1.000000000000000000, 0.8660254037844387076, 1.000000000000000000, 0.8660254037844387076, 1.000000000000000000, 0.8660254037844387076, 1.000000000000000000, 0.8660254037844387076, 1.000000000000000000, 0.8660254037844387076, 1.000000000000000000, 0.8660254037844387076, 1.000000000000000000, 0.8660254037844387076, 1.000000000000000000, 0.8660254037844387076, 1.000000000000000000, 0.8660254037844387076, 1.000000000000000000, 0.8660254037844387076, 1.000000000000000000, 0.8660254037844387076, 1.000000000000000000, 0.8660254037844387076, 1.000000000000000000, 0.8660254037844387076, 1.000000000000000000, 0.8660254037844387076, 1.000000000000000000, 0.8660254037844387076, 1.000000000000000000, 0.8660254037844387076, 1.000000000000000000, 0.8660254037844387076, 1.000000000000000000, 0.8660254037844387076, 1.000000000000000000, 0.8660254037844387076, 1.000000000000000000, 0.8660254037844387076, 1.000000000000000000, 0.8660254037844387076, 1.000000000000000000, 0.8660254037844387076, 1.000000000000000000, 0.8660254037844387076, 1.000000000000000000, 0.8660254037844387076, 1.000000000000000000, 0.8660254037844387076, 1.000000000000000000, 0.8660254037844387076, 1.000000000000000000, 0.8660254037844387076, 1.000000000000000000, 0.8660254037844387076, 1.000000000000000000, 0.8660254037844387076, 1.000000000000000000, 0.8660254037844387076, 1.000000000000000000, 0.8660254037844387076, 1.000000000000000000, 0.8660254037844387076, 1.000000000000000000, 0.8660254037844387076, 1.000000000000000000, 0.8660254037844387076, 1.000000000000000000, 0.8660254037844387076, 1.000000000000000000, 0.8660254037844387076, 1.000000000000000000, 0.8660254037844387076, 1.000000000000000000, 0.8660254037844387076, 1.000000000000000000, 0.8660254037844387076, 1.000000000000000000, 0.8660254037844387076, 1.000000000000000000, 0.8660254037844387076, 1.000000000000000000, 0.8660254037844387076, 1.000000000000000000, 0.8660254037844387076, 1.000000000000000000, 0.8660254037844387076, 1.000000000000000000, 0.8660254037844387076, 1.000000000000000000, 0.8660254037844387076, 1.000000000000000000, 0.8660254037844387076, 1.000000000000000000, 0.8660254037844387076, 1.000000000000000000, 0.8660254037844387076, 1.000000000000000000, 0.8660254037844387076, 1.000000000000000000, 0.8660254037844387076, 1.000000000000000000, 0.8660254037844387076, 1.000000000000000000, 0.8660254037844387076, 1.000000000000000000, 0.8660254037844387076, 1.000000000000000000, 0.8660254037844387076, 1.000000000000000000, 0.8660254037844387076, 1.000000000000000000, 0.8660254037844387076, 1.000000000000000000, 0.8660254037844387076, 1.000000000000000000, 0.8660254037844387076, 1.000000000000000000, 0.8660254037844387076, 1.000000000000000000, 0.8660254037844387076, 1.000000000000000000, 0.8660254037844387076, 1.000000000000000000, 0.8660254037844387076, 1.000000000000000000, 0.8660254037844387076, 1.000000000000000000, 0.8660254037844387076, 1.000000000000000000, 0.8660254037844387076, 1.000000000000000000, 0.8660254037844387076, 1.000000000000000000, 0.8660254037844387076, 1.000000000000000000, 0.8660254037844387076, 1.000000000000000000, 0.8660254037844387076, 1.000000000000000000, 0.8660254037844387076, 1.000000000000000000, 0.8660254037844387076, 1.000000000000000000, 0.8660254037844387076, 1.000000000000000000, 0.8660254037844387076, 1.000000000000000000, 0.8660254037844387076, 1.000000000000000000, 0.8660254037844387076, 1.000000000000000000, 0.8660254037844387076, 1.000000000000000000, 0.8660254037844387076, 1.000000000000000000, 0.8660254037844387076, 1.000000000000000000, 0.8660254037844387076, 1.000000000000000000, 0.8660254037844387076, 1.000000000000000000, 0.8660254037844387076, 1.000000000000000000, 0.8660254037844387076, 1.000000000000000000, 0.8660254037844387076, 1.000000000000000000, 0.8660254037844387076, 1.000000000000000000, 0.8660254037844387076, 1.000000000000000000, 0.8660254037844387076, 1.000000000000000000, 0.8660254037844387076, 1.000000000000000000, 0.8660254037844387076, 1.000000000000000000, 0.8660254037844387076, 1.000000000000000000, 0.8660254037844387076, 1.000000000000000000, 0.8660254037844387076, 1.000000000000000000, 0.8660254037844387076, 1.000000000000000000, 0.8660254037844387076, 1.000000000000000000, 0.8660254037844387076, 1.000000000000000000, 0.8660254037844387076, 1.000000000000000000, 0.8660254037844387076, 1.000000000000000000, 0.8660254037844387076, 1.000000000000000000, 0.8660254037844387076, 1.000000000000000000, 0.8660254037844387076, 1.000000000000000000, 0.9548847207714155072, 0.9401541335272467492) ) ) 
 REPRESENTATION_ITEM ( '' )  SURFACE ( )  );
#5937 = CARTESIAN_POINT ( 'NONE',  ( 18.12178482187499640, 4.985214923628404904, -2.128124999385472282 ) ) ;
#5938 = CARTESIAN_POINT ( 'NONE',  ( -12.50000000000000355, 61.68981371789855928, 0.1745138560722786503 ) ) ;
#5939 = CARTESIAN_POINT ( 'NONE',  ( -27.24356964374999635, 197.1968750006145115, 15.72908226750539384 ) ) ;
#5940 = EDGE_LOOP ( 'NONE', ( #8655, #3007, #28913, #16752 ) ) ;
#5941 = ORIENTED_EDGE ( 'NONE', *, *, #9197, .F. ) ;
#5942 = ORIENTED_EDGE ( 'NONE', *, *, #16906, .T. ) ;
#5943 = CARTESIAN_POINT ( 'NONE',  ( 26.75643035624999655, -3.323476615752267271, -5.353124999385477700 ) ) ;
#5944 = CARTESIAN_POINT ( 'NONE',  ( 33.61057809361597748, 5.196152422706637353, 159.7184274410858507 ) ) ;
#5945 = CARTESIAN_POINT ( 'NONE',  ( 23.87821517812499650, 247.3468750006144887, -4.985214923628404904 ) ) ;
#5946 = CARTESIAN_POINT ( 'NONE',  ( -12.50000000000000355, 40.31018628210144783, -0.1745138560725492671 ) ) ;
#5947 = CARTESIAN_POINT ( 'NONE',  ( -51.38169563604516554, 210.1155267958017703, 6.500000000000000888 ) ) ;
#5948 = DIRECTION ( 'NONE',  ( -0.000000000000000000, -0.000000000000000000, 1.000000000000000000 ) ) ;
#5949 = VECTOR ( 'NONE', #32868, 1000.000000000000000 ) ;
#5950 = CARTESIAN_POINT ( 'NONE',  ( -32.38169563604516554, 210.1155267958017703, 4.499999999999996447 ) ) ;
#5951 = SURFACE_STYLE_FILL_AREA ( #23029 ) ;
#5952 = CARTESIAN_POINT ( 'NONE',  ( 24.74287602148848464, 3.464101615137752166, 161.6235481623922681 ) ) ;
#5953 = CARTESIAN_POINT ( 'NONE',  ( 4.944772684328420986, 95.61481371789857064, 11.48171059495408208 ) ) ;
#5954 = CARTESIAN_POINT ( 'NONE',  ( -56.73288769728824832, 205.5309553116392465, -1.321298161741839117 ) ) ;
#5955 = CARTESIAN_POINT ( 'NONE',  ( -43.47247103062156981, 205.6499508600178956, 7.303452534266880569 ) ) ;
#5956 =( BOUNDED_CURVE ( )  B_SPLINE_CURVE ( 2, ( #37036, #22659, #34204, #12145, #28507, #14117, #26736 ),
 .UNSPECIFIED., .F., .F. ) 
 B_SPLINE_CURVE_WITH_KNOTS ( ( 3, 2, 2, 3 ),
 ( 0.1956521739130427651, 0.2028985507246371112, 0.2101449275362314573, 0.2173913043478258034 ),
 .UNSPECIFIED. ) 
 CURVE ( )  GEOMETRIC_REPRESENTATION_ITEM ( )  RATIONAL_B_SPLINE_CURVE ( ( 1.000000000000013323, 0.8660254037844252739, 1.000000000000000000, 0.8660254037844387076, 1.000000000000000000, 0.8660254037844438146, 0.9999999999999948930 ) ) 
 REPRESENTATION_ITEM ( '' )  );
#5957 = CARTESIAN_POINT ( 'NONE',  ( 15.24356964374999990, 0.000000000000000000, -4.303124999385482319 ) ) ;
#5958 = DIRECTION ( 'NONE',  ( 0.8660254037844187236, -0.5000000000000346390, 0.000000000000000000 ) ) ;
#5959 = CARTESIAN_POINT ( 'NONE',  ( -13.23911966647199812, 80.95231371789854791, -8.632099005475788900 ) ) ;
#5960 = CARTESIAN_POINT ( 'NONE',  ( -62.26711230271183695, 218.4690446883607535, -2.393094931466363651 ) ) ;
#5961 = EDGE_LOOP ( 'NONE', ( #12843, #35401, #13130, #13842 ) ) ;
#5962 = DIRECTION ( 'NONE',  ( -0.6427875693915772182, 0.000000000000000000, 0.7660444769304640689 ) ) ;
#5963 = CARTESIAN_POINT ( 'NONE',  ( -12.50000000000000355, 104.7101862821014606, -0.1745138560725492671 ) ) ;
#5964 = CARTESIAN_POINT ( 'NONE',  ( 5.770363421893814682, 37.43518628210144072, 14.38691631536207183 ) ) ;
#5965 = CARTESIAN_POINT ( 'NONE',  ( 25.01527935017339743, -2.343145750507547032, 50.00000000000000000 ) ) ;
#5966 = CARTESIAN_POINT ( 'NONE',  ( 24.66936984698473623, 3.604726614523240613, 163.5780169909762094 ) ) ;
#5967 = CARTESIAN_POINT ( 'NONE',  ( -8.927990412390661490, 75.67268628210143788, 13.04141134922759804 ) ) ;
#5968 = CARTESIAN_POINT ( 'NONE',  ( 22.56230152254410370, 0.000000000000000000, -10.00000000000000000 ) ) ;
#5969 = CARTESIAN_POINT ( 'NONE',  ( 14.39393478667391690, 5.957546110389989380, -10.12707779971139210 ) ) ;
#5970 = CARTESIAN_POINT ( 'NONE',  ( 20.99999999999999645, 210.0000000000000284, 0.000000000000000000 ) ) ;
#5971 = CARTESIAN_POINT ( 'NONE',  ( -48.81622103062156270, 211.6261429550005744, 6.530955311639227823 ) ) ;
#5972 = CARTESIAN_POINT ( 'NONE',  ( 26.99999999999999645, 241.2812500012290400, -7.347880794884117764E-16 ) ) ;
#5973 = CARTESIAN_POINT ( 'NONE',  ( -10.49813415415989581, 31.97268628210143859, -7.228626920339068285 ) ) ;
#5974 = CARTESIAN_POINT ( 'NONE',  ( -27.00000000000000355, 195.5000000000000000, 0.000000000000000000 ) ) ;
#5975 = CARTESIAN_POINT ( 'NONE',  ( 15.52041717089296213, 5.908847349338256727, -9.999738233010948107 ) ) ;
#5976 = CARTESIAN_POINT ( 'NONE',  ( -5.233372021372430183, 14.14768628210144286, -8.152565276336710909 ) ) ;
#5977 = CARTESIAN_POINT ( 'NONE',  ( 20.99999999999999645, 246.8218750006145399, 6.646953231504538984 ) ) ;
#5978 = EDGE_LOOP ( 'NONE', ( #17658, #1037, #2510, #14766 ) ) ;
#5979 = CARTESIAN_POINT ( 'NONE',  ( 24.00000000000000000, -5.196152422706629359, -5.700000000000010836 ) ) ;
#5980 = LINE ( 'NONE', #12043, #8814 ) ;
#5981 = ADVANCED_FACE ( 'NONE', ( #27528 ), #21849, .T. ) ;
#5982 = CARTESIAN_POINT ( 'NONE',  ( 30.90960795051509891, 6.928203230275506996, 163.2673371742559141 ) ) ;
#5983 = CARTESIAN_POINT ( 'NONE',  ( 10.31873187879411091, -3.604726614523240613, -4.153124999385542360 ) ) ;
#5984 = CARTESIAN_POINT ( 'NONE',  ( 37.41131328218130392, 7.646167579472015790E-16, 165.9452414505865079 ) ) ;
#5985 = CARTESIAN_POINT ( 'NONE',  ( 21.00000000000000000, 240.4375000000000000, -6.928203230275506996 ) ) ;
#5986 = FACE_OUTER_BOUND ( 'NONE', #23300, .T. ) ;
#5987 = EDGE_CURVE ( 'NONE', #22652, #8155, #814, .T. ) ;
#5988 = CARTESIAN_POINT ( 'NONE',  ( 11.61527771782819940, 62.73518628210145209, -4.622313124798573369 ) ) ;
#5989 = ORIENTED_EDGE ( 'NONE', *, *, #7419, .T. ) ;
#5990 = EDGE_LOOP ( 'NONE', ( #24725, #23324 ) ) ;
#5991 = CARTESIAN_POINT ( 'NONE',  ( 16.56230152254410726, 0.000000000000000000, -10.00000000000000000 ) ) ;
#5992 = DIRECTION ( 'NONE',  ( -0.000000000000000000, 1.000000000000000000, -0.000000000000000000 ) ) ;
#5993 = CARTESIAN_POINT ( 'NONE',  ( 1.120210788295102201E-13, 196.4000000012290741, -27.00000000000000711 ) ) ;
#5994 = CARTESIAN_POINT ( 'NONE',  ( 26.75643035624999655, -3.323476615752267715, -7.153124999385460647 ) ) ;
#5995 = CARTESIAN_POINT ( 'NONE',  ( -0.1745138560722442889, 36.38981371789855501, -15.50000000000000533 ) ) ;
#5996 = CARTESIAN_POINT ( 'NONE',  ( 18.12178482187499640, 4.985214923628404904, -10.22812499938549635 ) ) ;
#5997 = EDGE_CURVE ( 'NONE', #12534, #11333, #16163, .T. ) ;
#5998 = CARTESIAN_POINT ( 'NONE',  ( 21.00000000000000000, 240.7468750006145228, -6.646953231504538984 ) ) ;
#5999 = CARTESIAN_POINT ( 'NONE',  ( -38.52455436395490551, 206.6211998817774997, 3.209657149897401585 ) ) ;
#6000 = DIRECTION ( 'NONE',  ( 1.000000000000000000, 0.000000000000000000, 0.000000000000000000 ) ) ;
#6001 = CARTESIAN_POINT ( 'NONE',  ( 27.55375985076035761, -5.407089921784865361, 160.7282817348149706 ) ) ;
#6002 = CARTESIAN_POINT ( 'NONE',  ( -8.843639120294245259, 25.46481371789855075, -3.474262827703533230 ) ) ;
#6003 = CARTESIAN_POINT ( 'NONE',  ( -58.51413769728823411, 213.1499508600178672, 5.686928522499718142 ) ) ;
#6004 = CARTESIAN_POINT ( 'NONE',  ( -42.07961230271182984, 212.3930949314663792, 8.469044688360751749 ) ) ;
#6005 = CARTESIAN_POINT ( 'NONE',  ( 0.000000000000000000, 210.0000000000000284, 0.000000000000000000 ) ) ;
#6006 = CARTESIAN_POINT ( 'NONE',  ( -20.86978604919638869, 194.8588513911398081, -17.51182792271053046 ) ) ;
#6007 = CARTESIAN_POINT ( 'NONE',  ( 14.25334919248795451, 130.1148137178985564, -6.092822981423661410 ) ) ;
#6008 = VERTEX_POINT ( 'NONE', #18829 ) ;
#6009 = CARTESIAN_POINT ( 'NONE',  ( 11.61527771782819940, 53.53518628210144925, -4.622313124798573369 ) ) ;
#6010 = CARTESIAN_POINT ( 'NONE',  ( 19.56230152254410370, 5.196152422706631135, -9.937499998770999099 ) ) ;
#6011 = CARTESIAN_POINT ( 'NONE',  ( 25.23192384099550267, 3.919932473903637860, -7.999999999999996447 ) ) ;
#6012 = CARTESIAN_POINT ( 'NONE',  ( 24.36704836432882004, -3.604726614523240613, 160.1224666319704681 ) ) ;
#6013 = CARTESIAN_POINT ( 'NONE',  ( 26.99999999999999645, -3.464101615137751278, -2.006249998770952558 ) ) ;
#6014 = CARTESIAN_POINT ( 'NONE',  ( 10.31873187879410736, -3.604726614523244610, -8.259374999385515892 ) ) ;
#6015 = CARTESIAN_POINT ( 'NONE',  ( -67.22247103062156270, 206.6499508600178672, 5.571401726697986057 ) ) ;
#6016 = CARTESIAN_POINT ( 'NONE',  ( -9.534712964251941258, 58.42268628210145209, 1.715153634034234154 ) ) ;
#6017 = CARTESIAN_POINT ( 'NONE',  ( 15.00000000000000178, 249.5875000000000341, 3.464101615137757051 ) ) ;
#6018 = FACE_OUTER_BOUND ( 'NONE', #27165, .T. ) ;
#6019 = CARTESIAN_POINT ( 'NONE',  ( 10.69584247140445221, 90.04768628210145209, -6.932735513423970097 ) ) ;
#6020 = CARTESIAN_POINT ( 'NONE',  ( 36.63184559142159458, 7.347880794884125653E-16, 159.8305332246273167 ) ) ;
#6021 = CARTESIAN_POINT ( 'NONE',  ( -27.00000000000000355, 195.0266196731382706, -9.719019365307174141 ) ) ;
#6022 = VERTEX_POINT ( 'NONE', #22222 ) ;
#6023 = CARTESIAN_POINT ( 'NONE',  ( 24.63832061363088854, 0.000000000000000000, 163.2231226297810451 ) ) ;
#6024 = CARTESIAN_POINT ( 'NONE',  ( 26.75643035624999655, 3.323476615752271712, -7.528124999385462424 ) ) ;
#6025 = CARTESIAN_POINT ( 'NONE',  ( -13.62178482187500528, 196.1843750006145228, -23.59362340125807123 ) ) ;
#6026 = CARTESIAN_POINT ( 'NONE',  ( 24.87200694887302888, -3.604726614523244610, 165.8941696640395378 ) ) ;
#6027 = CARTESIAN_POINT ( 'NONE',  ( 31.05668326629465170, 6.928203230275514990, 164.9484157260613699 ) ) ;
#6028 = DIRECTION ( 'NONE',  ( 1.000000000000000000, 0.000000000000000000, 0.000000000000000000 ) ) ;
#6029 = CARTESIAN_POINT ( 'NONE',  ( 18.00000000000000000, 248.1250000000000000, -5.196152422706630247 ) ) ;
#6030 = CARTESIAN_POINT ( 'NONE',  ( -13.62178482187500528, 199.2781250006145228, -23.59362340125807123 ) ) ;
#6031 = CARTESIAN_POINT ( 'NONE',  ( -12.46528703574811558, 125.8023137178985706, 2.660918448318003726 ) ) ;
#6032 = CARTESIAN_POINT ( 'NONE',  ( 8.962234695871762469, 117.3601862821014521, -8.715434833791931624 ) ) ;
#6034 = VERTEX_POINT ( 'NONE', #4397 ) ;
#6033 = VERTEX_POINT ( 'NONE', #1553 ) ;
#6035 = CARTESIAN_POINT ( 'NONE',  ( 27.24356964374999635, 197.3656250006145285, -15.72908226750539029 ) ) ;
#6036 = CARTESIAN_POINT ( 'NONE',  ( 23.87821517812500005, 242.2468750006145228, 4.985214923628404016 ) ) ;
#6037 = CARTESIAN_POINT ( 'NONE',  ( -10.83675517735179028, 88.13981371789856212, 11.08355503943118947 ) ) ;
#6038 = CARTESIAN_POINT ( 'NONE',  ( 15.24356964374999990, 3.323476615752268604, -5.240624999385486760 ) ) ;
#6039 = CARTESIAN_POINT ( 'NONE',  ( 26.75643035624999655, 247.4218750006145058, -3.323476615752271712 ) ) ;
#6040 = VECTOR ( 'NONE', #32491, 1000.000000000000000 ) ;
#6041 = CARTESIAN_POINT ( 'NONE',  ( -27.00000000000000355, 196.4750000012290343, -15.58845726811989429 ) ) ;
#6042 = CARTESIAN_POINT ( 'NONE',  ( -9.500000000000005329, 70.88981371789854791, 0.1745138560723101806 ) ) ;
#6043 = CARTESIAN_POINT ( 'NONE',  ( 13.44051670066911264, 5.407089921784856479, -6.065624999385538452 ) ) ;
#6044 = CARTESIAN_POINT ( 'NONE',  ( 26.75643035624999655, 242.3593750006145342, -3.323476615752271268 ) ) ;
#6045 = CARTESIAN_POINT ( 'NONE',  ( 2.660918448318002838, 40.70231371789854791, 12.46528703574811558 ) ) ;
#6046 = CARTESIAN_POINT ( 'NONE',  ( 0.000000000000000000, 143.0000000000000000, -5.000000000000000888 ) ) ;
#6047 = CARTESIAN_POINT ( 'NONE',  ( -10.69584247140444866, 94.64768628210146062, 6.932735513423972762 ) ) ;
#6048 = CARTESIAN_POINT ( 'NONE',  ( 13.56230152254410548, 5.196152422706630247, -4.012499998771012599 ) ) ;
#6049 = CARTESIAN_POINT ( 'NONE',  ( -66.23288769728823411, 205.5309553116392465, -1.321298161741839117 ) ) ;
#6050 = CARTESIAN_POINT ( 'NONE',  ( 27.00000000000047251, 3.464101615137479495, -7.331249998770944742 ) ) ;
#6051 = CARTESIAN_POINT ( 'NONE',  ( 25.00000000000001421, 2.343145750507542147, 49.82535622836641664 ) ) ;
#6052 = CARTESIAN_POINT ( 'NONE',  ( -3.257655550457281723, 93.49768628210142651, 15.46528703574804986 ) ) ;
#6053 = CARTESIAN_POINT ( 'NONE',  ( 6.932735513423970097, 18.74768628210144072, 10.69584247140445044 ) ) ;
#6054 = DIRECTION ( 'NONE',  ( -0.000000000000000000, 1.000000000000000000, -0.000000000000000000 ) ) ;
#6055 = CARTESIAN_POINT ( 'NONE',  ( 10.56230152254410903, 7.347880794884117764E-16, -10.00000000000000000 ) ) ;
#6056 = CARTESIAN_POINT ( 'NONE',  ( 3.474262827703335166, 120.2351862821014521, 8.843639120294326972 ) ) ;
#6057 = CARTESIAN_POINT ( 'NONE',  ( 19.39230484541326405, 247.8986538117967200, 5.999999999999995559 ) ) ;
#6058 = CARTESIAN_POINT ( 'NONE',  ( -27.24356964375000345, 194.8857344423842619, -9.915847606754343957 ) ) ;
#6059 = CARTESIAN_POINT ( 'NONE',  ( 18.12178482187499640, 242.4718750006145171, -4.985214923628404904 ) ) ;
#6060 = ORIENTED_EDGE ( 'NONE', *, *, #12969, .T. ) ;
#6061 = CARTESIAN_POINT ( 'NONE',  ( 1.120210788295102201E-13, 195.5000000012290400, -27.00000000000000711 ) ) ;
#6062 = CARTESIAN_POINT ( 'NONE',  ( -8.152565276336710909, 67.04768628210143788, 5.233372021372435512 ) ) ;
#6063 = FACE_OUTER_BOUND ( 'NONE', #11698, .T. ) ;
#6064 = DIRECTION ( 'NONE',  ( -0.000000000000000000, -1.000000000000000000, -0.000000000000000000 ) ) ;
#6065 = FACE_OUTER_BOUND ( 'NONE', #35895, .T. ) ;
#6066 = LINE ( 'NONE', #11021, #10606 ) ;
#6067 = CARTESIAN_POINT ( 'NONE',  ( 24.98146486726017912, 0.000000000000000000, 164.3506311484184437 ) ) ;
#6068 = DIRECTION ( 'NONE',  ( -1.000000000000000000, 0.000000000000000000, 0.000000000000000000 ) ) ;
#6069 = CARTESIAN_POINT ( 'NONE',  ( 9.500000000000005329, 38.68981371789855217, -0.1745138560723090149 ) ) ;
#6070 = CARTESIAN_POINT ( 'NONE',  ( -27.24356964375000345, 199.3718750006145513, -15.72908226750537786 ) ) ;
#6071 = VERTEX_POINT ( 'NONE', #1742 ) ;
#6072 = ORIENTED_EDGE ( 'NONE', *, *, #18466, .F. ) ;
#6073 = CARTESIAN_POINT ( 'NONE',  ( 26.75643035624999655, 248.6218750006145228, -7.049594010296217766E-16 ) ) ;
#6074 = VECTOR ( 'NONE', #305, 1000.000000000000000 ) ;
#6075 = CARTESIAN_POINT ( 'NONE',  ( -6.932735513424201912, 41.85231371789854649, 10.69584247140429412 ) ) ;
#6076 = CARTESIAN_POINT ( 'NONE',  ( 10.31873187879411091, 3.604726614523240613, -8.784374999385505589 ) ) ;
#6077 = CARTESIAN_POINT ( 'NONE',  ( 15.24356964374999990, 0.000000000000000000, -0.1406249993854691294 ) ) ;
#6078 = CARTESIAN_POINT ( 'NONE',  ( 10.49813415416005213, 19.42731371789854933, -7.228626920338837358 ) ) ;
#6079 = CARTESIAN_POINT ( 'NONE',  ( 22.56230152254411792, 7.347880794884125653E-16, -1.125000000000042633 ) ) ;
#6080 = ORIENTED_EDGE ( 'NONE', *, *, #2517, .T. ) ;
#6081 = CARTESIAN_POINT ( 'NONE',  ( 19.68408634441910721, 5.407089921784862696, -3.046874999385523530 ) ) ;
#6082 = ORIENTED_EDGE ( 'NONE', *, *, #11242, .F. ) ;
#6083 = CARTESIAN_POINT ( 'NONE',  ( -27.24356964374999990, 199.3156250006145171, -15.72908226750537786 ) ) ;
#6084 = CARTESIAN_POINT ( 'NONE',  ( 37.40967911200478824, 3.604726614523243278, 165.9265627999972992 ) ) ;
#6085 = AXIS2_PLACEMENT_3D ( 'NONE', #5613, #32141, #17198 ) ;
#6086 = CARTESIAN_POINT ( 'NONE',  ( -68.00669563604516554, 209.8844732041981729, -8.500000000000003553 ) ) ;
#6087 = CARTESIAN_POINT ( 'NONE',  ( 15.24356964375000167, 249.3343750006145001, 3.323476615752272600 ) ) ;
#6088 = FACE_OUTER_BOUND ( 'NONE', #36886, .T. ) ;
#6089 = CARTESIAN_POINT ( 'NONE',  ( -52.56919563604517265, 214.5000000000000284, -0.1155267958017627827 ) ) ;
#6091 = EDGE_CURVE ( 'NONE', #25480, #21774, #23611, .T. ) ;
#6090 = CARTESIAN_POINT ( 'NONE',  ( -34.76413769728823411, 213.1499508600178672, 5.686928522499718142 ) ) ;
#6092 = CARTESIAN_POINT ( 'NONE',  ( 31.34102887711597774, 6.928203230275506996, 168.1985009298100522 ) ) ;
#6093 = ORIENTED_EDGE ( 'NONE', *, *, #10076, .F. ) ;
#6094 = CARTESIAN_POINT ( 'NONE',  ( 28.31976137920325698, -5.196152422706638241, 168.0863951450442642 ) ) ;
#6095 = CARTESIAN_POINT ( 'NONE',  ( 15.46528703574811736, 20.00231371789855217, -3.257655550456947768 ) ) ;
#6096 = CARTESIAN_POINT ( 'NONE',  ( -56.93080436395490551, 201.5000000000000000, -0.1155267958017054536 ) ) ;
#6097 = CARTESIAN_POINT ( 'NONE',  ( -6.594114490232312775, 133.4601862821014606, -6.840914352312096547 ) ) ;
#6098 = CARTESIAN_POINT ( 'NONE',  ( 4.944772684328679446, 52.38518628210145067, -11.48171059495397373 ) ) ;
#6100 = ADVANCED_FACE ( 'NONE', ( #27894 ), #1924, .F. ) ;
#6099 = CARTESIAN_POINT ( 'NONE',  ( 19.56230152254412147, -5.196152422706635576, -4.800000000000082423 ) ) ;
#6101 = ORIENTED_EDGE ( 'NONE', *, *, #79, .T. ) ;
#6102 = CARTESIAN_POINT ( 'NONE',  ( -39.31622103062156270, 211.6261429550005744, 6.530955311639228711 ) ) ;
#6103 = CARTESIAN_POINT ( 'NONE',  ( 18.00000000000000000, 242.2749999999999773, -5.196152422706630247 ) ) ;
#6104 = CARTESIAN_POINT ( 'NONE',  ( 9.534712964251941258, 17.02268628210144996, -1.715153634034235708 ) ) ;
#6105 = CARTESIAN_POINT ( 'NONE',  ( -27.24356964375000345, 196.2593750006145399, 0.000000000000000000 ) ) ;
#6106 = CARTESIAN_POINT ( 'NONE',  ( 36.87697111800645899, 7.347880794884117764E-16, 162.6323308142347059 ) ) ;
#6107 = CARTESIAN_POINT ( 'NONE',  ( 23.99999999999999645, 5.196152422706631135, -4.143749998770957177 ) ) ;
#6108 = DIRECTION ( 'NONE',  ( -0.000000000000000000, -1.000000000000000000, -0.000000000000000000 ) ) ;
#6109 = EDGE_CURVE ( 'NONE', #14431, #19996, #15875, .T. ) ;
#6110 = CARTESIAN_POINT ( 'NONE',  ( 31.32141883499775403, -6.928203230275506996, 167.9743571227394341 ) ) ;
#6111 = CARTESIAN_POINT ( 'NONE',  ( 26.75643035624999655, 246.0718750006145115, -3.323476615752271712 ) ) ;
#6112 = CARTESIAN_POINT ( 'NONE',  ( -6.840914352311947333, 99.63981371789857633, -6.594114490232462877 ) ) ;
#6113 = CARTESIAN_POINT ( 'NONE',  ( 18.12178482187499640, 239.8843750006145115, -4.985214923628404904 ) ) ;
#6114 = AXIS2_PLACEMENT_3D ( 'NONE', #6558, #18704, #6945 ) ;
#6115 = VECTOR ( 'NONE', #25968, 1000.000000000000000 ) ;
#6116 = ORIENTED_EDGE ( 'NONE', *, *, #34481, .F. ) ;
#6117 = CARTESIAN_POINT ( 'NONE',  ( -54.55580436395489841, 216.5000000000000000, 0.1155267958017343610 ) ) ;
#6118 = ADVANCED_FACE ( 'NONE', ( #19762 ), #25791, .F. ) ;
#6119 = CARTESIAN_POINT ( 'NONE',  ( 21.00000000000000000, 246.7937500012290570, -6.928203230275506996 ) ) ;
#6120 = CARTESIAN_POINT ( 'NONE',  ( 12.53471296425189330, 94.17731371789855643, 2.311890736173451533 ) ) ;
#6121 = CARTESIAN_POINT ( 'NONE',  ( 19.68408634441910721, 5.407089921784862696, -2.596874999385518024 ) ) ;
#6122 = CARTESIAN_POINT ( 'NONE',  ( 24.36704836432882004, -3.604726614523240613, 160.1224666319704681 ) ) ;
#6123 = CARTESIAN_POINT ( 'NONE',  ( 21.00000000000000000, 6.646953231504538984, -3.065624999385470062 ) ) ;
#6124 = CARTESIAN_POINT ( 'NONE',  ( 11.61527771782809637, 66.86481371789855643, 4.622313124798827388 ) ) ;
#6125 = CARTESIAN_POINT ( 'NONE',  ( 27.24356964374999635, 198.7718750006145569, -15.72908226750539029 ) ) ;
#6126 = EDGE_CURVE ( 'NONE', #12454, #24665, #22407, .T. ) ;
#6127 = ORIENTED_EDGE ( 'NONE', *, *, #12350, .T. ) ;
#6128 = VERTEX_POINT ( 'NONE', #10832 ) ;
#6129 = CARTESIAN_POINT ( 'NONE',  ( 18.12178482187500350, -4.985214923628407568, -4.115624999385475213 ) ) ;
#6130 = CARTESIAN_POINT ( 'NONE',  ( 13.56230152254410726, 5.196152422706636465, -0.9750000000000591527 ) ) ;
#6131 = CARTESIAN_POINT ( 'NONE',  ( 15.24356964374999990, 247.4968750006145228, 0.000000000000000000 ) ) ;
#6132 = CARTESIAN_POINT ( 'NONE',  ( -10.49813415415989581, 31.97268628210143859, -7.228626920339068285 ) ) ;
#6133 = CARTESIAN_POINT ( 'NONE',  ( -46.82961230271183695, 211.8571965466040581, 6.469044688360755302 ) ) ;
#6134 = CARTESIAN_POINT ( 'NONE',  ( 15.90209636607630195, 223.5944096904683818, -3.170162721593450694 ) ) ;
#6135 = CARTESIAN_POINT ( 'NONE',  ( -33.56919563604517265, 214.5000000000000284, -0.1155267958017627827 ) ) ;
#6136 =( LENGTH_UNIT ( ) NAMED_UNIT ( * ) SI_UNIT ( .MILLI., .METRE. ) );
#6137 = CARTESIAN_POINT ( 'NONE',  ( 36.72335912141372205, 3.464101615137755275, 160.8765376588480080 ) ) ;
#6138 = AXIS2_PLACEMENT_3D ( 'NONE', #2891, #23188, #6309 ) ;
#6139 = CARTESIAN_POINT ( 'NONE',  ( -12.53471296425189152, 107.9773137178985536, -2.311890736173453753 ) ) ;
#6140 = CARTESIAN_POINT ( 'NONE',  ( -57.92038769728823411, 208.6787018382581778, 4.469044688360752637 ) ) ;
#6141 = CARTESIAN_POINT ( 'NONE',  ( -64.64955436395490551, 214.8429017333601792, -4.673758765035196383 ) ) ;
#6142 = CARTESIAN_POINT ( 'NONE',  ( 15.24356964375000167, -3.323476615752272600, -3.365624999385477878 ) ) ;
#6143 = LINE ( 'NONE', #14316, #17394 ) ;
#6144 = CARTESIAN_POINT ( 'NONE',  ( 5.770363421894130873, 73.76481371789856212, -14.38691631536193860 ) ) ;
#6145 = CARTESIAN_POINT ( 'NONE',  ( -60.48586230271183695, 205.8500491399821613, 7.418979330068642852 ) ) ;
#6146 = VECTOR ( 'NONE', #20023, 1000.000000000000000 ) ;
#6147 = EDGE_CURVE ( 'NONE', #22401, #20504, #9295, .T. ) ;
#6148 = VERTEX_POINT ( 'NONE', #8187 ) ;
#6149 = CARTESIAN_POINT ( 'NONE',  ( 20.99999999999999645, -6.928203230275506996, -0.7312499987709595306 ) ) ;
#6150 = CARTESIAN_POINT ( 'NONE',  ( 12.50000000000000355, 100.1101862821014521, 0.1745138560725507937 ) ) ;
#6151 = CARTESIAN_POINT ( 'NONE',  ( 0.1745138560725837118, 51.81018628210144783, -15.50000000000000533 ) ) ;
#6153 = ADVANCED_FACE ( 'NONE', ( #17461 ), #33955, .T. ) ;
#6152 = CARTESIAN_POINT ( 'NONE',  ( 23.99999999999999645, 5.196152422706631135, -5.943749998770952558 ) ) ;
#6154 = CARTESIAN_POINT ( 'NONE',  ( 24.44058602227215005, -3.604726614523244610, 160.9630059084853997 ) ) ;
#6155 = CARTESIAN_POINT ( 'NONE',  ( 5.770363421893814682, 65.03518628210144925, 14.38691631536207183 ) ) ;
#6156 = CARTESIAN_POINT ( 'NONE',  ( 5.778771075727756162E-15, 199.4656250006145797, 31.45816453501076637 ) ) ;
#6157 = EDGE_CURVE ( 'NONE', #22829, #3698, #5328, .T. ) ;
#6158 = CARTESIAN_POINT ( 'NONE',  ( 13.44051670066910908, 5.407089921784856479, -7.865624999385534721 ) ) ;
#6159 =( BOUNDED_CURVE ( )  B_SPLINE_CURVE ( 2, ( #33491, #9810, #24954, #36324, #21388, #32929, #7166 ),
 .UNSPECIFIED., .F., .F. ) 
 B_SPLINE_CURVE_WITH_KNOTS ( ( 3, 2, 2, 3 ),
 ( 0.8043478260869539875, 0.8115942028985483336, 0.8188405797101425687, 0.8260869565217369148 ),
 .UNSPECIFIED. ) 
 CURVE ( )  GEOMETRIC_REPRESENTATION_ITEM ( )  RATIONAL_B_SPLINE_CURVE ( ( 1.000000000000047296, 0.8660254037843915231, 1.000000000000000000, 0.8660254037844387076, 1.000000000000000000, 0.8660254037844797859, 0.9999999999999589217 ) ) 
 REPRESENTATION_ITEM ( '' )  );
#6160 = CARTESIAN_POINT ( 'NONE',  ( 15.00000000000000355, 7.347880794884112834E-16, -8.000000000000000000 ) ) ;
#6161 = CARTESIAN_POINT ( 'NONE',  ( -44.06622103062156981, 211.6261429550005744, 6.530955311639227823 ) ) ;
#6162 = CYLINDRICAL_SURFACE ( 'NONE', #12988, 27.00000000000000355 ) ;
#6163 = CARTESIAN_POINT ( 'NONE',  ( 0.1745138560725515708, 42.61018628210144499, -12.50000000000000355 ) ) ;
#6164 = CARTESIAN_POINT ( 'NONE',  ( -27.00000000000000355, 195.0263594417697846, -9.827195513778322677 ) ) ;
#6165 = CARTESIAN_POINT ( 'NONE',  ( 21.00000000000000000, 240.2125000000000057, 5.999999999999998224 ) ) ;
#6166 = CARTESIAN_POINT ( 'NONE',  ( -9.500000000000005329, 12.71018628210143753, -0.1745138560725176813 ) ) ;
#6167 = CARTESIAN_POINT ( 'NONE',  ( 26.75643035624999655, 246.4468750006144830, 3.323476615752267271 ) ) ;
#6168 = ORIENTED_EDGE ( 'NONE', *, *, #36051, .F. ) ;
#6169 = CARTESIAN_POINT ( 'NONE',  ( 26.99999999999999645, -3.464101615137751278, -7.912500000000003197 ) ) ;
#6170 = AXIS2_PLACEMENT_3D ( 'NONE', #17783, #23283, #25931 ) ;
#6171 = CARTESIAN_POINT ( 'NONE',  ( 15.24356964374999990, 249.7468750006145228, 0.000000000000000000 ) ) ;
#6172 = ADVANCED_FACE ( 'NONE', ( #28445 ), #22963, .T. ) ;
#6173 = CARTESIAN_POINT ( 'NONE',  ( 16.56230152254410370, -6.928203230275506996, -3.374999998770986664 ) ) ;
#6174 = CARTESIAN_POINT ( 'NONE',  ( 10.31873187879410914, 0.000000000000000000, -3.740624999385516958 ) ) ;
#6175 = CARTESIAN_POINT ( 'NONE',  ( 37.53224187524366329, 3.604726614523238837, 167.3274615941888044 ) ) ;
#6176 = CARTESIAN_POINT ( 'NONE',  ( 18.00000000000000000, 240.0249999999999773, -5.196152422706630247 ) ) ;
#6177 = CARTESIAN_POINT ( 'NONE',  ( 33.62038311478219299, 5.196152422706631135, 159.8304993458455385 ) ) ;
#6178 = CARTESIAN_POINT ( 'NONE',  ( -10.69584247140444866, 76.24768628210144072, 6.932735513423972762 ) ) ;
#6179 = ORIENTED_EDGE ( 'NONE', *, *, #12556, .F. ) ;
#6180 = VERTEX_POINT ( 'NONE', #31665 ) ;
#6181 = LINE ( 'NONE', #11317, #36962 ) ;
#6182 = FACE_OUTER_BOUND ( 'NONE', #36847, .T. ) ;
#6183 = CARTESIAN_POINT ( 'NONE',  ( 26.97716818855048260, 0.000000000000000000, 49.47706554351410801 ) ) ;
#6184 = CARTESIAN_POINT ( 'NONE',  ( 18.12178482187499640, 4.985214923628404904, -6.065624999385454963 ) ) ;
#6185 = CARTESIAN_POINT ( 'NONE',  ( -12.46528703574805697, 86.59768628210144925, -2.660918448318280838 ) ) ;
#6186 = CARTESIAN_POINT ( 'NONE',  ( -15.50000000000000533, 24.88981371789854080, 0.1745138560722471477 ) ) ;
#6187 = CARTESIAN_POINT ( 'NONE',  ( 25.05010001456683710, 0.000000000000000000, 165.1351344719413419 ) ) ;
#6188 = CARTESIAN_POINT ( 'NONE',  ( 23.87821517812499650, 241.6093750006145342, -4.985214923628404904 ) ) ;
#6189 =( BOUNDED_CURVE ( )  B_SPLINE_CURVE ( 2, ( #20385, #5580, #34583, #17351, #11832, #37236, #31926 ),
 .UNSPECIFIED., .F., .F. ) 
 B_SPLINE_CURVE_WITH_KNOTS ( ( 3, 2, 2, 3 ),
 ( 0.4999999999999986122, 0.5072463768115930138, 0.5144927536231872489, 0.5217391304347815950 ),
 .UNSPECIFIED. ) 
 CURVE ( )  GEOMETRIC_REPRESENTATION_ITEM ( )  RATIONAL_B_SPLINE_CURVE ( ( 1.000000000000025535, 0.8660254037844129504, 1.000000000000000000, 0.8660254037844387076, 1.000000000000000000, 0.8660254037844571373, 0.9999999999999815703 ) ) 
 REPRESENTATION_ITEM ( '' )  );
#6190 = CARTESIAN_POINT ( 'NONE',  ( -63.65252896937850124, 207.6499508600178387, -3.839350919129087547 ) ) ;
#6191 = FACE_OUTER_BOUND ( 'NONE', #33107, .T. ) ;
#6192 = CARTESIAN_POINT ( 'NONE',  ( 24.36214585379926589, -3.604726614523244610, 160.0664306802028136 ) ) ;
#6193 = CARTESIAN_POINT ( 'NONE',  ( -5.529263428287297444, 17.12731371789855217, -7.954856959092311719 ) ) ;
#6194 = CARTESIAN_POINT ( 'NONE',  ( -54.75372103062154849, 216.5309553116391612, -1.626142955000564383 ) ) ;
#6195 = CARTESIAN_POINT ( 'NONE',  ( -33.76711230271183695, 218.4690446883607535, -2.393094931466363651 ) ) ;
#6196 = CARTESIAN_POINT ( 'NONE',  ( 10.56230152254410726, 0.000000000000000000, -4.387499998770999277 ) ) ;
#6197 = CARTESIAN_POINT ( 'NONE',  ( 13.62178482187499640, 195.6593750006145456, -23.59362340125807123 ) ) ;
#6198 = CARTESIAN_POINT ( 'NONE',  ( -14.25334919248795096, 125.5148137178985763, 6.092822981423662299 ) ) ;
#6199 = CARTESIAN_POINT ( 'NONE',  ( -52.76711230271183695, 216.4690446883607535, -1.857196546604089393 ) ) ;
#6200 = EDGE_CURVE ( 'NONE', #32805, #32692, #5177, .T. ) ;
#6201 = ORIENTED_EDGE ( 'NONE', *, *, #4531, .F. ) ;
#6202 = CARTESIAN_POINT ( 'NONE',  ( -11.48171059495397373, 50.08518628210144641, -4.944772684328680334 ) ) ;
#6203 = DIRECTION ( 'NONE',  ( 0.000000000000000000, 0.000000000000000000, -1.000000000000000000 ) ) ;
#6204 = CARTESIAN_POINT ( 'NONE',  ( 23.34314575050773044, -3.999999999999902744, 49.89769604716121876 ) ) ;
#6205 = CARTESIAN_POINT ( 'NONE',  ( 24.94717877699287811, 0.000000000000000000, 166.7533875911436780 ) ) ;
#6206 = CARTESIAN_POINT ( 'NONE',  ( 18.00000000000000355, -5.196152422706632912, -2.118749998770957710 ) ) ;
#6207 = CARTESIAN_POINT ( 'NONE',  ( 22.80587116629412137, 7.646167579472024665E-16, -8.971874999385509142 ) ) ;
#6208 = CARTESIAN_POINT ( 'NONE',  ( -64.84747103062156270, 213.3500491399821328, -5.571401726697985168 ) ) ;
#6209 = CARTESIAN_POINT ( 'NONE',  ( 16.56230152254411436, 7.209453229046475009, -2.053124999385520066 ) ) ;
#6210 = CARTESIAN_POINT ( 'NONE',  ( -3.796722387233375073, 56.98518628210145209, 8.710071997420127943 ) ) ;
#6211 = CARTESIAN_POINT ( 'NONE',  ( 18.00000000000000000, 249.4749999999999943, -5.196152422706630247 ) ) ;
#6212 = FACE_OUTER_BOUND ( 'NONE', #22994, .T. ) ;
#6213 = CARTESIAN_POINT ( 'NONE',  ( -8.715434833791929847, 96.66018628210146346, -8.962234695871762469 ) ) ;
#6214 = CARTESIAN_POINT ( 'NONE',  ( 7.234628195640322446, 199.6825961894323598, 26.99999999999999645 ) ) ;
#6215 = CARTESIAN_POINT ( 'NONE',  ( -13.49999999999998401, 195.2375000012290229, 23.38268590217985476 ) ) ;
#6216 = ORIENTED_EDGE ( 'NONE', *, *, #17958, .F. ) ;
#6217 = DIRECTION ( 'NONE',  ( -1.000000000000000000, 0.000000000000000000, 0.000000000000000000 ) ) ;
#6218 = CARTESIAN_POINT ( 'NONE',  ( 23.87821517812500005, -4.985214923628404016, -6.740624999385463667 ) ) ;
#6219 = LINE ( 'NONE', #29907, #13849 ) ;
#6220 = CARTESIAN_POINT ( 'NONE',  ( 31.17679477432231394, -7.209453229046482114, 166.3212965449812657 ) ) ;
#6221 = CARTESIAN_POINT ( 'NONE',  ( 33.96355885174396860, 5.196152422706637353, 163.7530159683574311 ) ) ;
#6222 = CARTESIAN_POINT ( 'NONE',  ( 24.00000000000000000, -5.196152422706629359, -6.993749998770947940 ) ) ;
#6223 = CARTESIAN_POINT ( 'NONE',  ( 15.00000000000000178, 248.6875000000000284, 3.464101615137757051 ) ) ;
#6224 = CARTESIAN_POINT ( 'NONE',  ( 27.24356964375000345, 195.9781250006145399, -3.336375036156643733E-15 ) ) ;
#6225 = CARTESIAN_POINT ( 'NONE',  ( -11.61527771782809282, 108.2648137178985621, -4.622313124798832717 ) ) ;
#6226 = CARTESIAN_POINT ( 'NONE',  ( 4.622313124798573369, 129.4351862821014549, 11.61527771782819940 ) ) ;
#6228 = ORIENTED_EDGE ( 'NONE', *, *, #27306, .F. ) ;
#6227 = ORIENTED_EDGE ( 'NONE', *, *, #3340, .F. ) ;
#6229 = CARTESIAN_POINT ( 'NONE',  ( 13.62178482187501416, 195.4531250006145342, 23.59362340125806767 ) ) ;
#6230 = CARTESIAN_POINT ( 'NONE',  ( 15.24356964374999990, 242.0593750006145513, -3.323476615752268604 ) ) ;
#6231 = CARTESIAN_POINT ( 'NONE',  ( 14.38691631536194393, 85.26481371789857633, 5.770363421894124656 ) ) ;
#6232 = CIRCLE ( 'NONE', #2328, 1.499999999999990452 ) ;
#6233 = CARTESIAN_POINT ( 'NONE',  ( 18.12178482187499640, 4.985214923628404904, -4.378124999385474503 ) ) ;
#6234 = CARTESIAN_POINT ( 'NONE',  ( 15.24356964374999990, 247.1593750006145171, 0.000000000000000000 ) ) ;
#6235 = CARTESIAN_POINT ( 'NONE',  ( 1.715153634034233487, 102.1226862821014549, 9.534712964251941258 ) ) ;
#6236 = PRODUCT_DEFINITION_SHAPE ( 'NONE', 'NONE',  #37054 ) ;
#6237 = CARTESIAN_POINT ( 'NONE',  ( -27.00000000000000355, 196.9625000012290172, 0.000000000000000000 ) ) ;
#6238 = CARTESIAN_POINT ( 'NONE',  ( 8.843639120294245259, 66.86481371789854222, 3.474262827703527901 ) ) ;
#6239 = CARTESIAN_POINT ( 'NONE',  ( 10.31873187879410736, 0.000000000000000000, -6.440624999385525129 ) ) ;
#6240 = ADVANCED_FACE ( 'NONE', ( #2666 ), #26361, .T. ) ;
#6241 = CARTESIAN_POINT ( 'NONE',  ( 18.12178482187499640, 241.1218750006145228, -4.985214923628404904 ) ) ;
#6242 = CARTESIAN_POINT ( 'NONE',  ( 12.46528703574811558, 47.60231371789855359, -2.660918448318005503 ) ) ;
#6243 = EDGE_CURVE ( 'NONE', #35635, #20463, #5695, .T. ) ;
#6244 = CARTESIAN_POINT ( 'NONE',  ( 19.56230152254411792, -5.196152422706629359, -1.537499998771035825 ) ) ;
#6245 = CARTESIAN_POINT ( 'NONE',  ( 6.932735513423970097, 101.5476862821014379, 10.69584247140445044 ) ) ;
#6246 = CARTESIAN_POINT ( 'NONE',  ( 13.56230152254411614, -5.196152422706632912, -6.562499998771037291 ) ) ;
#6247 = EDGE_CURVE ( 'NONE', #26373, #1047, #32351, .T. ) ;
#6248 = CARTESIAN_POINT ( 'NONE',  ( -67.42038769728826253, 208.6787018382581778, 4.469044688360752637 ) ) ;
#6249 = CARTESIAN_POINT ( 'NONE',  ( 12.50000000000000355, 136.9101862821014777, 0.1745138560725507937 ) ) ;
#6250 = CARTESIAN_POINT ( 'NONE',  ( 15.00000000000000000, 241.0187500012290229, -3.464101615137752610 ) ) ;
#6251 = CARTESIAN_POINT ( 'NONE',  ( 15.50000000000000533, 81.71018628210144641, 0.1745138560725827404 ) ) ;
#6252 = PRODUCT_RELATED_PRODUCT_CATEGORY ( 'part', '', ( #28294 ) ) ;
#6253 = DIRECTION ( 'NONE',  ( -0.000000000000000000, -0.000000000000000000, 1.000000000000000000 ) ) ;
#6254 = CYLINDRICAL_SURFACE ( 'NONE', #4320, 5.000000000000000000 ) ;
#6255 = CARTESIAN_POINT ( 'NONE',  ( 20.99999999999995381, 244.3187500012290627, 5.999999999999998224 ) ) ;
#6256 = CARTESIAN_POINT ( 'NONE',  ( 8.843639120294328748, 108.7351862821014663, -3.474262827703334722 ) ) ;
#6257 = FACE_BOUND ( 'NONE', #4216, .T. ) ;
#6258 = CARTESIAN_POINT ( 'NONE',  ( -13.04141134922759804, 13.57268628210145422, -8.927990412390657937 ) ) ;
#6259 = CARTESIAN_POINT ( 'NONE',  ( 13.62178482187499640, 196.1093750006145342, -23.59362340125807123 ) ) ;
#6260 = CARTESIAN_POINT ( 'NONE',  ( 15.24356964375000167, 241.6843750006144944, 3.323476615752272600 ) ) ;
#6261 = ORIENTED_EDGE ( 'NONE', *, *, #32163, .T. ) ;
#6262 = CARTESIAN_POINT ( 'NONE',  ( 24.91286120328598841, 0.000000000000000000, 166.3611359287700395 ) ) ;
#6263 = CARTESIAN_POINT ( 'NONE',  ( 23.87821517812499650, 4.985214923628404904, -0.2906249993854803648 ) ) ;
#6264 = CARTESIAN_POINT ( 'NONE',  ( 15.00000000000000000, 0.000000000000000000, -7.649999999999989697 ) ) ;
#6265 = CARTESIAN_POINT ( 'NONE',  ( 13.56230152254410548, 5.196152422706636465, -7.725000000000036948 ) ) ;
#6266 = PLANE ( 'NONE',  #10014 ) ;
#6267 = DIRECTION ( 'NONE',  ( 0.000000000000000000, 0.000000000000000000, 1.000000000000000000 ) ) ;
#6268 = CARTESIAN_POINT ( 'NONE',  ( 10.31873187879411091, 0.000000000000000000, -0.1406249993855246405 ) ) ;
#6269 = CARTESIAN_POINT ( 'NONE',  ( -8.843639120294245259, 43.86481371789854933, -3.474262827703533230 ) ) ;
#6270 = CARTESIAN_POINT ( 'NONE',  ( 13.62178482187501416, 199.1093750006145342, 23.59362340125806767 ) ) ;
#6271 = ORIENTED_EDGE ( 'NONE', *, *, #889, .F. ) ;
#6272 = CARTESIAN_POINT ( 'NONE',  ( 18.00000000000000000, 240.0812500012290513, -5.196152422706630247 ) ) ;
#6273 = CARTESIAN_POINT ( 'NONE',  ( -10.69584247140429412, 44.15231371789854364, -6.932735513424201024 ) ) ;
#6274 = CARTESIAN_POINT ( 'NONE',  ( 21.00000000000000000, -6.646953231504538984, -8.690624999385464733 ) ) ;
#6275 = CARTESIAN_POINT ( 'NONE',  ( -0.1745138560722763466, 8.789813717898553591, -12.50000000000000355 ) ) ;
#6276 = AXIS2_PLACEMENT_3D ( 'NONE', #21708, #24542, #32879 ) ;
#6277 = DIRECTION ( 'NONE',  ( 0.000000000000000000, 1.000000000000000000, -3.273063162220408568E-16 ) ) ;
#6278 = VERTEX_POINT ( 'NONE', #31481 ) ;
#6279 = CARTESIAN_POINT ( 'NONE',  ( 22.80587116629411426, 3.604726614523243278, -2.634374999385521221 ) ) ;
#6280 = ORIENTED_EDGE ( 'NONE', *, *, #1154, .T. ) ;
#6281 = CARTESIAN_POINT ( 'NONE',  ( 27.24356964375000345, 198.6781250006145569, -3.336375036156643733E-15 ) ) ;
#6282 = CARTESIAN_POINT ( 'NONE',  ( 24.94391043663983965, 3.604726614523240613, 166.7160302899652322 ) ) ;
#6283 = CARTESIAN_POINT ( 'NONE',  ( -34.75669563604516554, 209.8844732041982013, -6.500000000000000888 ) ) ;
#6284 = CARTESIAN_POINT ( 'NONE',  ( 23.87821517812499650, 249.1468750006145285, -4.985214923628404904 ) ) ;
#6285 = DIRECTION ( 'NONE',  ( 0.000000000000000000, 0.000000000000000000, -1.000000000000000000 ) ) ;
#6286 = CARTESIAN_POINT ( 'NONE',  ( -61.47544563604516554, 213.3788001182224718, 3.209657149897419348 ) ) ;
#6287 = CARTESIAN_POINT ( 'NONE',  ( -37.13913769728823411, 206.8500491399821044, -5.686928522499717253 ) ) ;
#6288 = CARTESIAN_POINT ( 'NONE',  ( 37.48648511030114605, -3.604726614523235284, 166.8044593776906197 ) ) ;
#6289 = ORIENTED_EDGE ( 'NONE', *, *, #9460, .F. ) ;
#6290 = CARTESIAN_POINT ( 'NONE',  ( 37.29858702344112231, 7.347880794884125653E-16, 167.4514226650291562 ) ) ;
#6291 = CARTESIAN_POINT ( 'NONE',  ( 14.25334919248782661, 137.4851862821014379, 6.092822981423971385 ) ) ;
#6292 = CIRCLE ( 'NONE', #23241, 3.500000000000002220 ) ;
#6293 = CARTESIAN_POINT ( 'NONE',  ( -65.44122103062156270, 207.8379586601371329, -8.530955311639223382 ) ) ;
#6294 = PRODUCT_DEFINITION_FORMATION_WITH_SPECIFIED_SOURCE ( 'ANY', '', #5602, .NOT_KNOWN. ) ;
#6295 = CARTESIAN_POINT ( 'NONE',  ( -8.843639120294326972, 122.5351862821014493, 3.474262827703335166 ) ) ;
#6296 = VECTOR ( 'NONE', #8068, 1000.000000000000000 ) ;
#6297 = CARTESIAN_POINT ( 'NONE',  ( -2.311890736173176641, 33.12268628210144072, -12.53471296425194836 ) ) ;
#6298 = VECTOR ( 'NONE', #12788, 1000.000000000000000 ) ;
#6300 = EDGE_CURVE ( 'NONE', #12051, #34283, #28629, .T. ) ;
#6299 = CARTESIAN_POINT ( 'NONE',  ( 22.56230152254412147, 3.464101615137759271, -5.587500000000029665 ) ) ;
#6301 = VERTEX_POINT ( 'NONE', #5506 ) ;
#6302 = CARTESIAN_POINT ( 'NONE',  ( -37.93080436395489841, 203.5000000000000000, -0.1155267958017335561 ) ) ;
#6303 = CARTESIAN_POINT ( 'NONE',  ( 15.50000000000000533, 127.7101862821014606, 0.1745138560725827404 ) ) ;
#6304 = CARTESIAN_POINT ( 'NONE',  ( 1.069080835302379631E-14, 198.8750000012290400, 27.00000000000000000 ) ) ;
#6305 = CARTESIAN_POINT ( 'NONE',  ( -3.474262827703337830, 23.63518628210144357, -8.843639120294326972 ) ) ;
#6306 = CARTESIAN_POINT ( 'NONE',  ( -1.926257025242585782E-15, 195.6968750006145683, -31.45816453501075927 ) ) ;
#6307 = DIRECTION ( 'NONE',  ( 0.000000000000000000, -1.000000000000000000, 0.000000000000000000 ) ) ;
#6308 = CARTESIAN_POINT ( 'NONE',  ( 21.00000000000000355, 0.000000000000000000, 50.00000000000001421 ) ) ;
#6309 = DIRECTION ( 'NONE',  ( 0.000000000000000000, 0.000000000000000000, 1.000000000000000000 ) ) ;
#6310 = CARTESIAN_POINT ( 'NONE',  ( 18.12178482187500350, 244.5343750006145456, 4.985214923628407568 ) ) ;
#6311 = CARTESIAN_POINT ( 'NONE',  ( 7.954856959092311719, 102.2273137178985678, -5.529263428287300108 ) ) ;
#6312 = CARTESIAN_POINT ( 'NONE',  ( -71.54107125509844423, 209.3291073423510795, 5.000000000000000000 ) ) ;
#6313 = ORIENTED_EDGE ( 'NONE', *, *, #24239, .T. ) ;
#6314 = CARTESIAN_POINT ( 'NONE',  ( -60.49330436395489841, 210.1155267958017134, -6.500000000000000888 ) ) ;
#6315 = CARTESIAN_POINT ( 'NONE',  ( 18.00000000000000355, 246.5312500012290400, 5.196152422706632912 ) ) ;
#6316 = CARTESIAN_POINT ( 'NONE',  ( 6.932735513424201024, 92.45231371789854791, -10.69584247140429412 ) ) ;
#6317 = CARTESIAN_POINT ( 'NONE',  ( 16.56230152254411436, 7.209453229046482114, -0.7593749993855121172 ) ) ;
#6318 = CARTESIAN_POINT ( 'NONE',  ( 36.82628035898769525, 3.604726614523238837, 159.2582845396456719 ) ) ;
#6319 = CARTESIAN_POINT ( 'NONE',  ( 18.12178482187500350, -4.985214923628407568, -1.078124999385476901 ) ) ;
#6320 = CARTESIAN_POINT ( 'NONE',  ( -11.48171059495408208, 61.11481371789854933, 4.944772684328421875 ) ) ;
#6321 = CARTESIAN_POINT ( 'NONE',  ( -13.62178482187498396, 198.5843750006145569, 23.59362340125808188 ) ) ;
#6322 = EDGE_CURVE ( 'NONE', #20178, #10985, #19759, .T. ) ;
#6323 = VERTEX_POINT ( 'NONE', #29186 ) ;
#6324 = ADVANCED_FACE ( 'NONE', ( #3228 ), #6826, .T. ) ;
#6325 = ORIENTED_EDGE ( 'NONE', *, *, #27983, .F. ) ;
#6326 = CARTESIAN_POINT ( 'NONE',  ( 23.87821517812500005, -4.985214923628404016, -5.390624999385473792 ) ) ;
#6327 = FACE_OUTER_BOUND ( 'NONE', #15458, .T. ) ;
#6328 = CARTESIAN_POINT ( 'NONE',  ( 21.00000000000000000, 246.9343750006145228, -6.646953231504538984 ) ) ;
#6329 = CARTESIAN_POINT ( 'NONE',  ( 4.622313124798573369, 37.43518628210144783, 11.61527771782819940 ) ) ;
#6330 = CARTESIAN_POINT ( 'NONE',  ( -49.79836230271183695, 204.3130714775002446, -3.149950860017828091 ) ) ;
#6331 = CARTESIAN_POINT ( 'NONE',  ( 10.42677199038734592, 213.9649605036083528, -4.520320870630215815 ) ) ;
#6332 = CARTESIAN_POINT ( 'NONE',  ( -30.99627896937850480, 205.4690446883607535, -1.090244570138286351 ) ) ;
#6333 = CARTESIAN_POINT ( 'NONE',  ( 36.83448269341698733, -3.464101615137751278, 162.1466858989149387 ) ) ;
#6334 = CARTESIAN_POINT ( 'NONE',  ( -8.715434833792127023, 88.13981371789856212, 8.962234695871568846 ) ) ;
#6335 = CARTESIAN_POINT ( 'NONE',  ( -58.11830436395491262, 209.8844732041982297, 4.499999999999996447 ) ) ;
#6336 = CARTESIAN_POINT ( 'NONE',  ( -65.04538769728824832, 211.8571965466039444, -6.469044688360768625 ) ) ;
#6337 = EDGE_CURVE ( 'NONE', #22269, #17991, #7900, .T. ) ;
#6338 = CARTESIAN_POINT ( 'NONE',  ( 23.87821517812499650, 4.985214923628404904, -7.603124999385480365 ) ) ;
#6339 = DIRECTION ( 'NONE',  ( -0.000000000000000000, -0.000000000000000000, 1.000000000000000000 ) ) ;
#6340 = CARTESIAN_POINT ( 'NONE',  ( -10.83675517735179028, 69.73981371789855643, 11.08355503943118947 ) ) ;
#6341 = CARTESIAN_POINT ( 'NONE',  ( -64.24627896937850835, 201.4690446883607251, -2.162041339862721845 ) ) ;
#6342 = ORIENTED_EDGE ( 'NONE', *, *, #1022, .T. ) ;
#6343 = CARTESIAN_POINT ( 'NONE',  ( 15.52041717089296213, 5.908847349338256727, -9.999738233010948107 ) ) ;
#6344 = CARTESIAN_POINT ( 'NONE',  ( -8.715434833791929847, 87.46018628210144641, -8.962234695871762469 ) ) ;
#6345 = CARTESIAN_POINT ( 'NONE',  ( 14.25334919248782661, 45.48518628210144499, 6.092822981423971385 ) ) ;
#6346 = EDGE_CURVE ( 'NONE', #37113, #27676, #28190, .T. ) ;
#6347 = CARTESIAN_POINT ( 'NONE',  ( -81.00000000000002842, 210.0000000000000000, -2.499999999999998668 ) ) ;
#6348 = CARTESIAN_POINT ( 'NONE',  ( 24.47326942580252407, 3.604726614523240613, 161.3365789202697727 ) ) ;
#6349 = CARTESIAN_POINT ( 'NONE',  ( -5.770363421893818234, 51.23518628210143788, -14.38691631536207005 ) ) ;
#6350 = CARTESIAN_POINT ( 'NONE',  ( 27.24356964375000345, 199.5781250006145342, -3.336375036156643733E-15 ) ) ;
#6351 = CARTESIAN_POINT ( 'NONE',  ( 10.31873187879411091, 3.604726614523236616, -8.728124999385524774 ) ) ;
#6352 = AXIS2_PLACEMENT_3D ( 'NONE', #36755, #36564, #10981 ) ;
#6353 = CARTESIAN_POINT ( 'NONE',  ( 20.99999999999999645, 185.0294372515228645, -5.999999999999999112 ) ) ;
#6354 = CARTESIAN_POINT ( 'NONE',  ( -51.98288769728821990, 203.5309553116391612, -1.857196546604028775 ) ) ;
#6355 = CARTESIAN_POINT ( 'NONE',  ( 0.1745138560725515708, 33.41018628210144925, -12.50000000000000355 ) ) ;
#6356 = CARTESIAN_POINT ( 'NONE',  ( 26.99999999999999645, 7.347880794884117764E-16, -3.768749998770942966 ) ) ;
#6357 = CARTESIAN_POINT ( 'NONE',  ( -9.465287035748065847, 3.797686282101448096, -2.064181346179273735 ) ) ;
#6358 = CARTESIAN_POINT ( 'NONE',  ( 20.99999999999999645, 246.1468750006145285, -6.646953231504538984 ) ) ;
#6359 = EDGE_LOOP ( 'NONE', ( #16449, #32660, #37421, #24323 ) ) ;
#6360 = CARTESIAN_POINT ( 'NONE',  ( 26.99999999999999645, -3.464101615137751278, -6.112499999999988276 ) ) ;
#6361 = CARTESIAN_POINT ( 'NONE',  ( -14.50000000000000000, 210.0000000000000000, 0.000000000000000000 ) ) ;
#6362 = CARTESIAN_POINT ( 'NONE',  ( 26.99999999999999645, 7.347880794884117764E-16, -1.968749998770946696 ) ) ;
#6363 = CARTESIAN_POINT ( 'NONE',  ( 13.44051670066911797, -5.407089921784859143, -4.115624999385558702 ) ) ;
#6364 = CARTESIAN_POINT ( 'NONE',  ( 25.02725311564228505, 3.604726614523236616, 167.6686414700154444 ) ) ;
#6365 = CARTESIAN_POINT ( 'NONE',  ( 26.99999999999999645, 240.3625000000000114, -3.464101615137755275 ) ) ;
#6366 = LINE ( 'NONE', #32699, #16090 ) ;
#6367 = CARTESIAN_POINT ( 'NONE',  ( -11.48171059495397373, 50.08518628210144641, -4.944772684328680334 ) ) ;
#6368 = VERTEX_POINT ( 'NONE', #6456 ) ;
#6369 = VERTEX_POINT ( 'NONE', #21064 ) ;
#6370 = CARTESIAN_POINT ( 'NONE',  ( 33.95048549033182184, -5.196152422706635576, 163.6035867636436478 ) ) ;
#6371 = CARTESIAN_POINT ( 'NONE',  ( 22.60769515458672885, 246.5325961894323541, 5.999999999999997335 ) ) ;
#6372 = CARTESIAN_POINT ( 'NONE',  ( 18.12178482187500350, -4.985214923628407568, -6.815624999385455851 ) ) ;
#6373 = CARTESIAN_POINT ( 'NONE',  ( -8.715434833791929847, 96.66018628210146346, -8.962234695871762469 ) ) ;
#6374 = CARTESIAN_POINT ( 'NONE',  ( 15.50000000000000533, 20.28981371789855004, -0.1745138560722452326 ) ) ;
#6375 = CARTESIAN_POINT ( 'NONE',  ( 21.00000000000000000, 249.4375000000000568, -5.999999999999998224 ) ) ;
#6376 = CARTESIAN_POINT ( 'NONE',  ( 15.24356964374999990, 240.3718750006145228, -3.323476615752268604 ) ) ;
#6377 = CARTESIAN_POINT ( 'NONE',  ( -67.80877896937849414, 211.0902445701383101, -4.530955311639234040 ) ) ;
#6378 = CARTESIAN_POINT ( 'NONE',  ( -5.530181890562601232, 223.3271220116375275, 2.500000000000000000 ) ) ;
#6379 = CARTESIAN_POINT ( 'NONE',  ( 36.82137784845814821, 3.604726614523243278, 159.2022485878779889 ) ) ;
#6380 = CARTESIAN_POINT ( 'NONE',  ( 8.152565276336593669, 11.95231371789853902, 5.233372021372610483 ) ) ;
#6381 = CARTESIAN_POINT ( 'NONE',  ( -57.52455436395488420, 205.1570982666397356, 4.673758765035198159 ) ) ;
#6382 = CARTESIAN_POINT ( 'NONE',  ( -30.40252896937850124, 205.6499508600178103, -7.303452534266820173 ) ) ;
#6383 = AXIS2_PLACEMENT_3D ( 'NONE', #15313, #26866, #24035 ) ;
#6384 = CARTESIAN_POINT ( 'NONE',  ( 0.000000000000000000, 0.000000000000000000, 0.000000000000000000 ) ) ;
#6385 = DIRECTION ( 'NONE',  ( -0.000000000000000000, -0.000000000000000000, 1.000000000000000000 ) ) ;
#6386 = CARTESIAN_POINT ( 'NONE',  ( -27.24356964374999990, 196.2218750006145456, -15.72908226750537786 ) ) ;
#6387 = CARTESIAN_POINT ( 'NONE',  ( -13.23911966647199812, 136.1523137178985507, -8.632099005475788900 ) ) ;
#6388 = CARTESIAN_POINT ( 'NONE',  ( -57.71502896937850124, 215.5714017266979567, -3.350049139982168800 ) ) ;
#6389 = EDGE_CURVE ( 'NONE', #4918, #21578, #30150, .T. ) ;
#6390 = ORIENTED_EDGE ( 'NONE', *, *, #20591, .T. ) ;
#6391 =( BOUNDED_CURVE ( )  B_SPLINE_CURVE ( 2, ( #34672, #5863, #28606, #22945, #176, #9091, #11373, #8532, #11743 ),
 .UNSPECIFIED., .F., .F. ) 
 B_SPLINE_CURVE_WITH_KNOTS ( ( 3, 2, 2, 2, 3 ),
 ( 0.2717391304347825942, 0.2753623188405797118, 0.2826086956521738913, 0.2898550724637681264, 0.2934782608695652439 ),
 .UNSPECIFIED. ) 
 CURVE ( )  GEOMETRIC_REPRESENTATION_ITEM ( )  RATIONAL_B_SPLINE_CURVE ( ( 0.9330127018922191873, 0.9330127018922187432, 1.000000000000000000, 0.8660254037844387076, 1.000000000000000000, 0.8660254037844387076, 1.000000000000000000, 0.9330127018922188542, 0.9330127018922194093 ) ) 
 REPRESENTATION_ITEM ( '' )  );
#6392 = CARTESIAN_POINT ( 'NONE',  ( -8.715434833791929847, 41.46018628210144641, -8.962234695871762469 ) ) ;
#6393 = CARTESIAN_POINT ( 'NONE',  ( -4.526655657482483441, 226.9744801578922022, -2.499999999999999556 ) ) ;
#6394 = CARTESIAN_POINT ( 'NONE',  ( 1.069080835302379631E-14, 198.7624999999999886, 27.00000000000000000 ) ) ;
#6395 = CARTESIAN_POINT ( 'NONE',  ( 28.20742792136773858, 5.407089921784862696, 168.1997419705030552 ) ) ;
#6396 = CARTESIAN_POINT ( 'NONE',  ( 24.00000000000000000, -5.196152422706629359, -3.393749998770956289 ) ) ;
#6397 = CARTESIAN_POINT ( 'NONE',  ( -67.61830436395489130, 209.8844732041982581, 6.500000000000000888 ) ) ;
#6398 = CARTESIAN_POINT ( 'NONE',  ( 13.44051670066911264, 5.407089921784856479, -1.565624999385561988 ) ) ;
#6399 = CARTESIAN_POINT ( 'NONE',  ( 9.500000000000005329, 54.11018628210144499, 0.1745138560725188748 ) ) ;
#6400 = CARTESIAN_POINT ( 'NONE',  ( 50.97598229932587799, 123.5575933553551522, 0.5000000000000000000 ) ) ;
#6401 = CARTESIAN_POINT ( 'NONE',  ( 0.000000000000000000, 141.0000000000000000, 0.000000000000000000 ) ) ;
#6402 = CARTESIAN_POINT ( 'NONE',  ( 2.660918448318279950, 88.89768628210146062, -12.46528703574805697 ) ) ;
#6403 = CARTESIAN_POINT ( 'NONE',  ( 27.00000000000001421, 199.7375000000000114, 15.58845726811988897 ) ) ;
#6404 = DIRECTION ( 'NONE',  ( -1.000000000000000000, -6.123233995736766036E-17, 0.000000000000000000 ) ) ;
#6405 = EDGE_LOOP ( 'NONE', ( #22858, #25663, #2931, #16829, #11316 ) ) ;
#6406 = CARTESIAN_POINT ( 'NONE',  ( 36.82301201863464968, 7.646167579472015790E-16, 159.2209272384671976 ) ) ;
#6407 = CARTESIAN_POINT ( 'NONE',  ( 26.75643035624999655, 7.049594010296217766E-16, -9.365624999385479654 ) ) ;
#6408 = FACE_OUTER_BOUND ( 'NONE', #12127, .T. ) ;
#6409 = CARTESIAN_POINT ( 'NONE',  ( 27.93288733171263516, 5.407089921784862696, 165.0617286715140608 ) ) ;
#6410 = CARTESIAN_POINT ( 'NONE',  ( 27.92756053683882911, -5.196152422706638241, 163.6035190036313622 ) ) ;
#6411 = CARTESIAN_POINT ( 'NONE',  ( 37.10575494261148322, 3.464101615138019508, 165.2473418955011937 ) ) ;
#6412 = CARTESIAN_POINT ( 'NONE',  ( 21.00000000000000000, 249.4375000000000000, -6.928203230275506996 ) ) ;
#6413 = CARTESIAN_POINT ( 'NONE',  ( -13.62178482187500528, 197.0281250006145228, -23.59362340125807123 ) ) ;
#6414 = CIRCLE ( 'NONE', #27599, 7.500000000000000000 ) ;
#6415 =( BOUNDED_CURVE ( )  B_SPLINE_CURVE ( 2, ( #2877, #14450, #17118, #5531, #35, #11600, #25449 ),
 .UNSPECIFIED., .F., .F. ) 
 B_SPLINE_CURVE_WITH_KNOTS ( ( 3, 2, 2, 3 ),
 ( 0.000000000000000000, 0.007246376811594299264, 0.01449275362318859853, 0.02173913043478289606 ),
 .UNSPECIFIED. ) 
 CURVE ( )  GEOMETRIC_REPRESENTATION_ITEM ( )  RATIONAL_B_SPLINE_CURVE ( ( 1.000000000000000000, 0.8660254037844387076, 1.000000000000000000, 0.8660254037844387076, 1.000000000000000000, 0.8660254037844333785, 1.000000000000005329 ) ) 
 REPRESENTATION_ITEM ( '' )  );
#6416 = CARTESIAN_POINT ( 'NONE',  ( -6.932735513424201912, 97.05231371789857064, 10.69584247140429412 ) ) ;
#6417 = CARTESIAN_POINT ( 'NONE',  ( -8.715434833791929847, 96.66018628210146346, -8.962234695871762469 ) ) ;
#6418 = EDGE_LOOP ( 'NONE', ( #27583, #31801, #3275, #29103 ) ) ;
#6419 = CARTESIAN_POINT ( 'NONE',  ( -27.24356964374999990, 195.2656250006145342, -15.72908226750537786 ) ) ;
#6420 = CARTESIAN_POINT ( 'NONE',  ( 20.99999999999999289, 248.8187500012290911, 5.999999999999999112 ) ) ;
#6421 = ADVANCED_FACE ( 'NONE', ( #18028 ), #11949, .F. ) ;
#6422 = CARTESIAN_POINT ( 'NONE',  ( -14.38691631536193860, 71.46481371789856496, -5.770363421894132649 ) ) ;
#6423 = CARTESIAN_POINT ( 'NONE',  ( 15.24356964375000167, -3.323476615752272600, -4.265624999385501326 ) ) ;
#6424 = CARTESIAN_POINT ( 'NONE',  ( 26.75643035624999655, 248.7718750006145569, -3.323476615752271712 ) ) ;
#6425 = CARTESIAN_POINT ( 'NONE',  ( -9.465287035748065847, 95.79768628210145209, -2.064181346179273735 ) ) ;
#6426 = VECTOR ( 'NONE', #4288, 1000.000000000000000 ) ;
#6427 = CARTESIAN_POINT ( 'NONE',  ( -1.909035429704832693E-15, 197.7500000012290400, -31.17691453623979214 ) ) ;
#6428 = CARTESIAN_POINT ( 'NONE',  ( 9.500000000000005329, 84.68981371789855928, -0.1745138560723090149 ) ) ;
#6429 = CARTESIAN_POINT ( 'NONE',  ( 16.56230152254411436, -7.209453229046475009, -4.978124999385539873 ) ) ;
#6430 = CARTESIAN_POINT ( 'NONE',  ( 26.75643035624999655, 242.7343750006145058, 3.323476615752267271 ) ) ;
#6431 = CARTESIAN_POINT ( 'NONE',  ( -10.69584247140429412, 53.35231371789855359, -6.932735513424201024 ) ) ;
#6432 = CARTESIAN_POINT ( 'NONE',  ( 20.99999999999999645, 249.6625000000000512, 5.999999999999998224 ) ) ;
#6433 = CARTESIAN_POINT ( 'NONE',  ( -2.660918448318275509, 102.6976862821014720, 12.46528703574805874 ) ) ;
#6434 = CARTESIAN_POINT ( 'NONE',  ( 22.56230152254410370, 7.347880794884117764E-16, -6.862499998771004250 ) ) ;
#6435 = VECTOR ( 'NONE', #22137, 1000.000000000000000 ) ;
#6436 = CARTESIAN_POINT ( 'NONE',  ( -32.98288769728824121, 203.5309553116391612, -1.857196546604028775 ) ) ;
#6437 = CARTESIAN_POINT ( 'NONE',  ( 10.49813415415989581, 137.7726862821014606, 7.228626920339068285 ) ) ;
#6438 = CARTESIAN_POINT ( 'NONE',  ( 34.13799077639428958, -5.407089921784855591, 164.3494578665133474 ) ) ;
#6439 = CARTESIAN_POINT ( 'NONE',  ( 2.908627838312118019, 74.52268628210144641, 15.53471296425195369 ) ) ;
#6440 = CARTESIAN_POINT ( 'NONE',  ( 10.31873187879411091, 3.604726614523240613, -3.834374999385520066 ) ) ;
#6441 = CARTESIAN_POINT ( 'NONE',  ( -2.311890736173176641, 5.522686282101451738, -12.53471296425194659 ) ) ;
#6442 = PLANE ( 'NONE',  #20666 ) ;
#6443 = CARTESIAN_POINT ( 'NONE',  ( 10.49999999999999645, 244.5000000000000000, 2.500000000000000000 ) ) ;
#6444 = CARTESIAN_POINT ( 'NONE',  ( -1.715153634034234598, 115.9226862821014521, -9.534712964251941258 ) ) ;
#6445 = DIRECTION ( 'NONE',  ( 0.8660254037844224984, 0.000000000000000000, -0.5000000000000278666 ) ) ;
#6446 = CARTESIAN_POINT ( 'NONE',  ( 8.927990412390657937, 6.672686282101436106, -13.04141134922759804 ) ) ;
#6447 = CARTESIAN_POINT ( 'NONE',  ( -27.24356964375000345, 195.3593750006145342, 0.000000000000000000 ) ) ;
#6448 = CARTESIAN_POINT ( 'NONE',  ( 15.24356964374999990, 242.9968750006145228, 0.000000000000000000 ) ) ;
#6449 = ORIENTED_EDGE ( 'NONE', *, *, #8485, .F. ) ;
#6450 = CARTESIAN_POINT ( 'NONE',  ( 28.18618370907300275, -5.407089921784859143, 167.9569195128432000 ) ) ;
#6451 =( BOUNDED_CURVE ( )  B_SPLINE_CURVE ( 2, ( #2471, #10448, #18999, #2102, #30922, #30738, #30556 ),
 .UNSPECIFIED., .F., .F. ) 
 B_SPLINE_CURVE_WITH_KNOTS ( ( 3, 2, 2, 3 ),
 ( 0.8478260869565198421, 0.8550724637681141882, 0.8623188405797084233, 0.8695652173913026584 ),
 .UNSPECIFIED. ) 
 CURVE ( )  GEOMETRIC_REPRESENTATION_ITEM ( )  RATIONAL_B_SPLINE_CURVE ( ( 1.000000000000034861, 0.8660254037844038466, 1.000000000000000000, 0.8660254037844387076, 1.000000000000000000, 0.8660254037844694608, 0.9999999999999692468 ) ) 
 REPRESENTATION_ITEM ( '' )  );
#6452 = CARTESIAN_POINT ( 'NONE',  ( 18.12178482187500350, -4.985214923628407568, -2.315624999385479388 ) ) ;
#6453 = VECTOR ( 'NONE', #1858, 1000.000000000000000 ) ;
#6455 = ADVANCED_FACE ( 'NONE', ( #17843 ), #15175, .F. ) ;
#6454 = CARTESIAN_POINT ( 'NONE',  ( 5.778771075727756162E-15, 199.0718750006145399, 31.45816453501076637 ) ) ;
#6456 = CARTESIAN_POINT ( 'NONE',  ( 15.24356964374999990, 249.7468750006145228, 0.000000000000000000 ) ) ;
#6457 = DIRECTION ( 'NONE',  ( 0.000000000000000000, 1.000000000000000000, 0.000000000000000000 ) ) ;
#6458 = EDGE_CURVE ( 'NONE', #29003, #33644, #20970, .T. ) ;
#6459 = CARTESIAN_POINT ( 'NONE',  ( 31.07629330841286830, -6.928203230275514990, 165.1725595331320449 ) ) ;
#6460 = DIRECTION ( 'NONE',  ( 0.08715574274765150453, 0.000000000000000000, 0.9961946980917461003 ) ) ;
#6461 = CARTESIAN_POINT ( 'NONE',  ( 8.843639120294245259, 20.86481371789854578, 3.474262827703527901 ) ) ;
#6462 = CARTESIAN_POINT ( 'NONE',  ( 27.24356964375000700, 198.6968750006145115, 15.72908226750537075 ) ) ;
#6463 = ORIENTED_EDGE ( 'NONE', *, *, #26275, .F. ) ;
#6464 = CARTESIAN_POINT ( 'NONE',  ( 26.75643035624999655, 247.6843750006145513, 3.323476615752267715 ) ) ;
#6465 = CARTESIAN_POINT ( 'NONE',  ( -10.49813415416004858, 42.42731371789855643, 7.228626920338840023 ) ) ;
#6466 = EDGE_CURVE ( 'NONE', #25042, #8199, #29757, .T. ) ;
#6467 = CARTESIAN_POINT ( 'NONE',  ( 15.24356964374999990, 3.323476615752268604, -1.978124999385461935 ) ) ;
#6468 = CARTESIAN_POINT ( 'NONE',  ( -10.83675517735179028, 134.1398137178985621, 11.08355503943118947 ) ) ;
#6469 = ADVANCED_FACE ( 'NONE', ( #35440 ), #32035, .F. ) ;
#6470 = CARTESIAN_POINT ( 'NONE',  ( 21.00000000000000000, -6.928203230275506996, -7.031249998770932486 ) ) ;
#6471 = CARTESIAN_POINT ( 'NONE',  ( -104.7527771047627994, 12.87393045632884636, 3.000000000000000000 ) ) ;
#6472 = ORIENTED_EDGE ( 'NONE', *, *, #25994, .F. ) ;
#6473 = CARTESIAN_POINT ( 'NONE',  ( 10.31873187879410736, 3.604726614523240613, -3.834374999385520955 ) ) ;
#6474 = CARTESIAN_POINT ( 'NONE',  ( -13.62178482187498396, 198.9781250006145399, 23.59362340125808188 ) ) ;
#6475 = CARTESIAN_POINT ( 'NONE',  ( 24.71512661192725702, -3.604726614523244610, 164.1010192074743657 ) ) ;
#6476 = CARTESIAN_POINT ( 'NONE',  ( -66.42336230271182274, 217.4189793300686233, 4.149950860017807663 ) ) ;
#6477 = CARTESIAN_POINT ( 'NONE',  ( 15.24356964374999990, 248.3593750006145342, -3.323476615752268604 ) ) ;
#6478 =( NAMED_UNIT ( * ) SI_UNIT ( $, .STERADIAN. ) SOLID_ANGLE_UNIT ( ) );
#6479 = AXIS2_PLACEMENT_3D ( 'NONE', #12815, #35363, #29496 ) ;
#6480 = CARTESIAN_POINT ( 'NONE',  ( -51.18377896937850835, 208.9097554298617183, 4.530955311639234040 ) ) ;
#6481 = CARTESIAN_POINT ( 'NONE',  ( 13.49999999999999645, 197.1500000000000057, -23.38268590217984766 ) ) ;
#6482 = CARTESIAN_POINT ( 'NONE',  ( 28.13389026342440857, 5.407089921784856479, 167.3592026939881237 ) ) ;
#6483 = VERTEX_POINT ( 'NONE', #23518 ) ;
#6484 = CARTESIAN_POINT ( 'NONE',  ( -27.87471972953271049, 209.7345472881551984, 8.000000000000001776 ) ) ;
#6485 = CARTESIAN_POINT ( 'NONE',  ( 13.23911966647218996, 136.0476862821014379, -8.632099005475504683 ) ) ;
#6486 = CARTESIAN_POINT ( 'NONE',  ( -60.29538769728823411, 212.3930949314662371, -8.469044688360781947 ) ) ;
#6487 = CARTESIAN_POINT ( 'NONE',  ( 0.1745138560725194299, 134.6101862821014947, -9.500000000000005329 ) ) ;
#6488 = DIRECTION ( 'NONE',  ( -0.000000000000000000, 1.000000000000000000, 0.000000000000000000 ) ) ;
#6489 = CARTESIAN_POINT ( 'NONE',  ( -6.932735513423968321, 23.34768628210144570, -10.69584247140445221 ) ) ;
#6490 = CARTESIAN_POINT ( 'NONE',  ( 19.56230152254412502, -5.196152422706635576, -6.600000000000050271 ) ) ;
#6491 = ORIENTED_EDGE ( 'NONE', *, *, #17296, .T. ) ;
#6492 = CARTESIAN_POINT ( 'NONE',  ( 2.999999999999997335, 244.5000000000000000, 5.000000000000000000 ) ) ;
#6493 = CARTESIAN_POINT ( 'NONE',  ( 2.908627838312118019, 129.7226862821014208, 15.53471296425195369 ) ) ;
#6494 = PLANE ( 'NONE',  #20020 ) ;
#6495 = CARTESIAN_POINT ( 'NONE',  ( 6.594114490232313663, 9.260186282101427580, 6.840914352312096547 ) ) ;
#6496 = CARTESIAN_POINT ( 'NONE',  ( 27.24356964375000345, 198.6781250006145569, -3.336375036156643733E-15 ) ) ;
#6497 = CARTESIAN_POINT ( 'NONE',  ( 5.649999999999987921, 244.5000000000000000, 5.000000000000000000 ) ) ;
#6498 = CARTESIAN_POINT ( 'NONE',  ( 17.25050943477418031, -6.183923782582014361, -9.999999999999998224 ) ) ;
#6499 = CARTESIAN_POINT ( 'NONE',  ( 31.41211527974097706, -7.209453229046482114, 169.0110222298289671 ) ) ;
#6500 = CARTESIAN_POINT ( 'NONE',  ( 21.00000000000001066, 247.0187500012290513, 5.999999999999998224 ) ) ;
#6501 = CARTESIAN_POINT ( 'NONE',  ( -6.594114490232462877, 78.93981371789855928, 6.840914352311949109 ) ) ;
#6502 = DIRECTION ( 'NONE',  ( -4.130293990420971855E-17, 1.000000000000000000, 0.000000000000000000 ) ) ;
#6503 = ORIENTED_EDGE ( 'NONE', *, *, #13571, .T. ) ;
#6504 = CARTESIAN_POINT ( 'NONE',  ( 26.99999999999999645, 247.1312500012290343, -7.347880794884117764E-16 ) ) ;
#6505 = CARTESIAN_POINT ( 'NONE',  ( -12.53471296425189152, 107.9773137178985678, -2.311890736173453309 ) ) ;
#6506 = CARTESIAN_POINT ( 'NONE',  ( 13.44051670066911264, -5.407089921784865361, -3.271874999385554261 ) ) ;
#6507 = CARTESIAN_POINT ( 'NONE',  ( 20.99999999999999645, 185.0294372515228645, 5.999999999999999112 ) ) ;
#6508 = CARTESIAN_POINT ( 'NONE',  ( 18.12178482187499640, 4.985214923628404904, -4.828124999385480010 ) ) ;
#6509 = CARTESIAN_POINT ( 'NONE',  ( 2.660918448318002838, 59.10231371789854649, 12.46528703574811558 ) ) ;
#6510 = CARTESIAN_POINT ( 'NONE',  ( 5.778771075727756162E-15, 197.7218750006145456, 31.45816453501075927 ) ) ;
#6511 = ORIENTED_EDGE ( 'NONE', *, *, #34489, .F. ) ;
#6512 = ORIENTED_EDGE ( 'NONE', *, *, #22570, .F. ) ;
#6513 = CARTESIAN_POINT ( 'NONE',  ( 23.87821517812499650, 4.985214923628404904, -5.690624999385468286 ) ) ;
#6514 = B_SPLINE_CURVE_WITH_KNOTS ( 'NONE', 1,
 ( #15281, #1236 ),
 .UNSPECIFIED., .F., .F.,
 ( 2, 2 ),
 ( 0.000000000000000000, 1.000000000000000000 ),
 .UNSPECIFIED. ) ;
#6515 = CARTESIAN_POINT ( 'NONE',  ( 1.069080835302379631E-14, 195.6124999999999829, 27.00000000000000000 ) ) ;
#6516 = CARTESIAN_POINT ( 'NONE',  ( 15.24356964375000167, 246.1843750006145513, 3.323476615752272600 ) ) ;
#6517 = CARTESIAN_POINT ( 'NONE',  ( -2.311890736173176641, 33.12268628210144072, -12.53471296425194836 ) ) ;
#6518 = CARTESIAN_POINT ( 'NONE',  ( -33.96502896937850124, 215.5714017266979567, -3.350049139982168800 ) ) ;
#6519 = CARTESIAN_POINT ( 'NONE',  ( 22.80587116629410716, 7.646167579472015790E-16, -0.3656249993855553715 ) ) ;
#6520 = SHAPE_REPRESENTATION ( 'pusher spring', ( #17215 ), #2050 ) ;
#6521 = CARTESIAN_POINT ( 'NONE',  ( -64.04836230271183695, 204.3130714775002446, -3.149950860017828091 ) ) ;
#6522 =( LENGTH_UNIT ( ) NAMED_UNIT ( * ) SI_UNIT ( .MILLI., .METRE. ) );
#6523 = CARTESIAN_POINT ( 'NONE',  ( 24.86707295490388958, -3.464101615137757051, 163.0431256071730104 ) ) ;
#6524 = CARTESIAN_POINT ( 'NONE',  ( 2.660918448318002838, 86.70231371789854791, 12.46528703574811558 ) ) ;
#6525 = CARTESIAN_POINT ( 'NONE',  ( -55.14955436395491262, 213.3788001182225003, -3.209657149897400252 ) ) ;
#6526 = CARTESIAN_POINT ( 'NONE',  ( -36.74330436395489130, 210.1155267958016850, -8.500000000000003553 ) ) ;
#6527 = CARTESIAN_POINT ( 'NONE',  ( 26.75643035624999655, 7.049594010296217766E-16, -7.228124999385493687 ) ) ;
#6528 = CARTESIAN_POINT ( 'NONE',  ( -77.00000000000002842, 210.0000000000000000, 5.000000000000000000 ) ) ;
#6529 = CARTESIAN_POINT ( 'NONE',  ( 15.53471296425188797, 57.37731371789855928, 2.908627838312457747 ) ) ;
#6530 = CARTESIAN_POINT ( 'NONE',  ( -64.64211230271182274, 201.5309553116392181, 2.393094931466368980 ) ) ;
#6531 = CARTESIAN_POINT ( 'NONE',  ( 0.000000000000000000, 143.0000000000000000, 7.500000000000000000 ) ) ;
#6532 = CARTESIAN_POINT ( 'NONE',  ( 4.622313124798573369, 83.43518628210145494, 11.61527771782819940 ) ) ;
#6533 = CARTESIAN_POINT ( 'NONE',  ( -2.908627838312119351, 33.12268628210143362, -15.53471296425195369 ) ) ;
#6534 = DIRECTION ( 'NONE',  ( 6.123233995736766036E-17, -1.000000000000000000, 0.000000000000000000 ) ) ;
#6535 = CARTESIAN_POINT ( 'NONE',  ( 20.99999999999998579, 248.1437500012290229, -5.999999999999997335 ) ) ;
#6536 = VECTOR ( 'NONE', #3458, 1000.000000000000000 ) ;
#6537 = CARTESIAN_POINT ( 'NONE',  ( 8.632099005475504683, 46.34768628210144925, 13.23911966647218996 ) ) ;
#6538 = CARTESIAN_POINT ( 'NONE',  ( -27.24356964375000345, 199.8031250006145285, 0.000000000000000000 ) ) ;
#6539 = CARTESIAN_POINT ( 'NONE',  ( 16.56230152254411081, 7.209453229046475009, -7.903124999385497063 ) ) ;
#6540 = LINE ( 'NONE', #6353, #14037 ) ;
#6541 = CARTESIAN_POINT ( 'NONE',  ( -38.52455436395488420, 205.1570982666397356, 4.673758765035198159 ) ) ;
#6542 = CARTESIAN_POINT ( 'NONE',  ( 13.49999999999999645, 195.8000000000000114, -23.38268590217984766 ) ) ;
#6543 = CARTESIAN_POINT ( 'NONE',  ( 4.944772684328679446, 15.58518628210145351, -11.48171059495397373 ) ) ;
#6544 = FACE_OUTER_BOUND ( 'NONE', #26441, .T. ) ;
#6545 = CARTESIAN_POINT ( 'NONE',  ( 0.1745138560723095977, 123.7898137178985678, 9.500000000000005329 ) ) ;
#6546 = CARTESIAN_POINT ( 'NONE',  ( 26.75643035624999655, 246.8968750006145285, 3.323476615752267271 ) ) ;
#6547 = ORIENTED_EDGE ( 'NONE', *, *, #24892, .F. ) ;
#6548 = CARTESIAN_POINT ( 'NONE',  ( 26.99999999999999645, 7.347880794884117764E-16, -6.525000000000003020 ) ) ;
#6549 = CARTESIAN_POINT ( 'NONE',  ( 18.00000000000000000, 245.0312500012290400, -5.196152422706630247 ) ) ;
#6550 = CARTESIAN_POINT ( 'NONE',  ( 22.56230152254364185, -3.464101615138027057, -3.299999998771030008 ) ) ;
#6551 = CARTESIAN_POINT ( 'NONE',  ( 10.31873187879411091, -3.604726614523240613, -7.303124999385512517 ) ) ;
#6552 = CARTESIAN_POINT ( 'NONE',  ( 24.95534962787547073, -3.604726614523240613, 166.8467808440897500 ) ) ;
#6553 = CARTESIAN_POINT ( 'NONE',  ( 26.99999999999999645, 242.1250000000000000, -7.347880794884117764E-16 ) ) ;
#6554 = CARTESIAN_POINT ( 'NONE',  ( -27.00000000000000355, 199.5500000000000114, 0.000000000000000000 ) ) ;
#6555 = CARTESIAN_POINT ( 'NONE',  ( 8.962234695871762469, 52.96018628210144641, -8.715434833791931624 ) ) ;
#6556 = VERTEX_POINT ( 'NONE', #9675 ) ;
#6557 = ORIENTED_EDGE ( 'NONE', *, *, #34278, .F. ) ;
#6558 = CARTESIAN_POINT ( 'NONE',  ( 20.99999999999999645, 0.000000000000000000, -8.000000000000000000 ) ) ;
#6559 = CARTESIAN_POINT ( 'NONE',  ( 22.56230152254412502, 7.347880794884125653E-16, -2.925000000000066436 ) ) ;
#6560 = CARTESIAN_POINT ( 'NONE',  ( 20.99999999999998579, 248.3124999999999716, 5.999999999999998224 ) ) ;
#6561 = CARTESIAN_POINT ( 'NONE',  ( 23.87821517812499650, 4.985214923628404904, -7.040624999385459049 ) ) ;
#6562 = CARTESIAN_POINT ( 'NONE',  ( 8.962234695871762469, 89.76018628210144357, -8.715434833791931624 ) ) ;
#6563 = CARTESIAN_POINT ( 'NONE',  ( -14.38691631536193860, 25.46481371789855075, -5.770363421894132649 ) ) ;
#6564 = FACE_OUTER_BOUND ( 'NONE', #25971, .T. ) ;
#6565 = CARTESIAN_POINT ( 'NONE',  ( 21.00000000000000000, 240.9718750006145456, 6.646953231504538984 ) ) ;
#6566 = VECTOR ( 'NONE', #18369, 1000.000000000000000 ) ;
#6567 = CARTESIAN_POINT ( 'NONE',  ( -32.98288769728823411, 205.5309553116392465, -1.321298161741839117 ) ) ;
#6568 = CARTESIAN_POINT ( 'NONE',  ( 18.00000000000000355, 245.5749999999999886, 5.196152422706632912 ) ) ;
#6569 = CARTESIAN_POINT ( 'NONE',  ( 37.38683221308021842, 7.347880794884117764E-16, 168.4600697980714017 ) ) ;
#6570 = CARTESIAN_POINT ( 'NONE',  ( 7.228626920338837358, 141.3273137178985337, 10.49813415416005036 ) ) ;
#6571 = CARTESIAN_POINT ( 'NONE',  ( -55.34747103062156981, 213.3500491399821328, -5.571401726697985168 ) ) ;
#6572 = CARTESIAN_POINT ( 'NONE',  ( -36.14211230271182984, 201.5309553116392181, 2.393094931466368980 ) ) ;
#6573 = CARTESIAN_POINT ( 'NONE',  ( 19.39230484541326049, 240.9075961894323541, -5.999999999999997335 ) ) ;
#6574 = CARTESIAN_POINT ( 'NONE',  ( 5.778771075727756162E-15, 199.4656250006145797, 31.45816453501075927 ) ) ;
#6575 = CARTESIAN_POINT ( 'NONE',  ( 5.770363421894130873, 119.7648137178985905, -14.38691631536193860 ) ) ;
#6576 = CARTESIAN_POINT ( 'NONE',  ( -62.46502896937850124, 215.5714017266979567, -3.350049139982168800 ) ) ;
#6577 = EDGE_LOOP ( 'NONE', ( #17723, #29316 ) ) ;
#6578 = CARTESIAN_POINT ( 'NONE',  ( 4.622313124798573369, 28.23518628210144854, 11.61527771782819940 ) ) ;
#6579 = CARTESIAN_POINT ( 'NONE',  ( 20.99999999999999645, 210.0000000000000284, 0.000000000000000000 ) ) ;
#6580 = EDGE_CURVE ( 'NONE', #21580, #5242, #5774, .T. ) ;
#6581 = CIRCLE ( 'NONE', #21722, 2.499999999999996891 ) ;
#6582 = CARTESIAN_POINT ( 'NONE',  ( 37.52733936471412335, 3.604726614523243278, 167.2714256424211499 ) ) ;
#6583 = CARTESIAN_POINT ( 'NONE',  ( -6.092822981423970496, 112.1851862821014691, 14.25334919248782661 ) ) ;
#6584 = CARTESIAN_POINT ( 'NONE',  ( -62.27455436395490551, 205.1570982666397640, 4.673758765035199048 ) ) ;
#6585 = CARTESIAN_POINT ( 'NONE',  ( 22.80587116629410716, 3.604726614523238837, -1.678124999385518068 ) ) ;
#6586 = CARTESIAN_POINT ( 'NONE',  ( 2.064181346179272847, 61.29768628210142367, -9.465287035748065847 ) ) ;
#6587 = LINE ( 'NONE', #6400, #30381 ) ;
#6588 = DIRECTION ( 'NONE',  ( 0.000000000000000000, 0.000000000000000000, 1.000000000000000000 ) ) ;
#6589 = ADVANCED_FACE ( 'NONE', ( #6065 ), #14985, .F. ) ;
#6590 = CARTESIAN_POINT ( 'NONE',  ( -11.61527771782819940, 76.53518628210146346, 4.622313124798574258 ) ) ;
#6591 = CARTESIAN_POINT ( 'NONE',  ( 3.253724281355069334E-15, 199.8875000000000455, -27.00000000000000000 ) ) ;
#6592 = LINE ( 'NONE', #10372, #19016 ) ;
#6593 = VERTEX_POINT ( 'NONE', #26535 ) ;
#6594 = CARTESIAN_POINT ( 'NONE',  ( 36.89818384675449181, -3.604726614523235284, 160.0801451655713379 ) ) ;
#6595 = CARTESIAN_POINT ( 'NONE',  ( 19.00081571707362116, 5.492723647597327563, -10.12707781181606492 ) ) ;
#6596 = CARTESIAN_POINT ( 'NONE',  ( 20.99999999999999645, 185.0294372515228645, 0.000000000000000000 ) ) ;
#6597 = CARTESIAN_POINT ( 'NONE',  ( 37.29201885929546734, 3.604726614523243278, 164.5816999575734201 ) ) ;
#6598 = UNCERTAINTY_MEASURE_WITH_UNIT (LENGTH_MEASURE( 1.000000000000000082E-05 ), #26556, 'distance_accuracy_value', 'NONE');
#6599 = CARTESIAN_POINT ( 'NONE',  ( 24.89321967762106169, 0.000000000000000000, 163.3419840153761982 ) ) ;
#6600 = CARTESIAN_POINT ( 'NONE',  ( 15.00000000000000000, 0.000000000000000000, -6.750000000000006217 ) ) ;
#6601 = CARTESIAN_POINT ( 'NONE',  ( 21.00000000000000000, 248.5374999999999943, -6.928203230275506996 ) ) ;
#6602 = CARTESIAN_POINT ( 'NONE',  ( -1.926257025242585782E-15, 196.5406250006145399, -31.45816453501076637 ) ) ;
#6603 = CARTESIAN_POINT ( 'NONE',  ( 12.53471296425189330, 103.3773137178985735, 2.311890736173451977 ) ) ;
#6604 = CARTESIAN_POINT ( 'NONE',  ( 12.50000000000000355, 100.1101862821014521, 0.1745138560725507937 ) ) ;
#6605 = VERTEX_POINT ( 'NONE', #37076 ) ;
#6606 = CARTESIAN_POINT ( 'NONE',  ( 27.24356964374999635, 196.9156250006145399, -15.72908226750539029 ) ) ;
#6607 = CARTESIAN_POINT ( 'NONE',  ( 26.75643035624999655, 240.0343750006145740, 3.323476615752267715 ) ) ;
#6608 = ADVANCED_FACE ( 'NONE', ( #36005 ), #21437, .T. ) ;
#6609 = CARTESIAN_POINT ( 'NONE',  ( -13.23911966647199812, 80.95231371789854791, -8.632099005475788900 ) ) ;
#6610 = CARTESIAN_POINT ( 'NONE',  ( 18.12178482187499640, 4.985214923628404904, -3.928124999385496086 ) ) ;
#6611 = CARTESIAN_POINT ( 'NONE',  ( 26.75643035624999655, 247.3843750006145399, -7.049594010296217766E-16 ) ) ;
#6612 = CARTESIAN_POINT ( 'NONE',  ( -2.064181346179269738, 102.6976862821014294, 9.465287035748067623 ) ) ;
#6613 = CARTESIAN_POINT ( 'NONE',  ( -13.49999999999998401, 195.2375000012290229, 23.38268590217985476 ) ) ;
#6614 = CARTESIAN_POINT ( 'NONE',  ( 7.954856959092311719, 56.22731371789854649, -5.529263428287300108 ) ) ;
#6615 = CARTESIAN_POINT ( 'NONE',  ( 10.31873187879411091, 3.604726614523236616, -6.478124999385515004 ) ) ;
#6616 =( BOUNDED_CURVE ( )  B_SPLINE_CURVE ( 2, ( #1722, #33571, #30913, #19744, #22018, #7607, #16514 ),
 .UNSPECIFIED., .F., .F. ) 
 B_SPLINE_CURVE_WITH_KNOTS ( ( 3, 2, 2, 3 ),
 ( 0.2391304347826091192, 0.2463768115942034653, 0.2536231884057977837, 0.2608695652173921298 ),
 .UNSPECIFIED. ) 
 CURVE ( )  GEOMETRIC_REPRESENTATION_ITEM ( )  RATIONAL_B_SPLINE_CURVE ( ( 0.9999999999999923395, 0.8660254037844463681, 1.000000000000000000, 0.8660254037844387076, 1.000000000000000000, 0.8660254037844232755, 1.000000000000015321 ) ) 
 REPRESENTATION_ITEM ( '' )  );
#6617 = CARTESIAN_POINT ( 'NONE',  ( 2.064181346179061460, 105.1023137178985678, 9.465287035748106703 ) ) ;
#6618 = CARTESIAN_POINT ( 'NONE',  ( 27.24356964375000345, 199.6343750006145399, -3.336375036156643733E-15 ) ) ;
#6619 = CARTESIAN_POINT ( 'NONE',  ( -0.1745138560722763466, 45.58981371789855075, -12.50000000000000355 ) ) ;
#6620 = FACE_OUTER_BOUND ( 'NONE', #26973, .T. ) ;
#6621 = CARTESIAN_POINT ( 'NONE',  ( -2.311890736173176641, 97.52268628210144641, -12.53471296425194836 ) ) ;
#6622 = CARTESIAN_POINT ( 'NONE',  ( 22.56230152254410370, 3.464101615137755275, -6.374999998771000875 ) ) ;
#6623 = CARTESIAN_POINT ( 'NONE',  ( -67.22247103062156270, 207.6499508600178387, 3.839350919129076445 ) ) ;
#6624 = CARTESIAN_POINT ( 'NONE',  ( -12.46528703574805697, 132.5976862821014777, -2.660918448318280838 ) ) ;
#6625 = CARTESIAN_POINT ( 'NONE',  ( 24.75271252598717808, 3.604726614523236616, 164.5306281710264216 ) ) ;
#6626 = CARTESIAN_POINT ( 'NONE',  ( 13.04141134922759804, 91.77268628210144641, 8.927990412390657937 ) ) ;
#6627 = CARTESIAN_POINT ( 'NONE',  ( 10.31873187879411091, -3.604726614523244610, -2.859374999385534633 ) ) ;
#6628 = CARTESIAN_POINT ( 'NONE',  ( 20.99999999999999645, -6.928203230275506996, -4.837499999999994138 ) ) ;
#6629 = EDGE_CURVE ( 'NONE', #30804, #6033, #7015, .T. ) ;
#6630 = CARTESIAN_POINT ( 'NONE',  ( -7.234628195640302017, 199.1924038105676686, 27.00000000000000711 ) ) ;
#6631 = CARTESIAN_POINT ( 'NONE',  ( -5.529263428287477744, 112.4726862821014635, 7.954856959092191815 ) ) ;
#6632 = DIRECTION ( 'NONE',  ( 0.000000000000000000, 0.000000000000000000, 1.000000000000000000 ) ) ;
#6633 =( BOUNDED_CURVE ( )  B_SPLINE_CURVE ( 2, ( #27773, #1803, #13370, #13936, #25484, #8060, #37404, #20181, #28880 ),
 .UNSPECIFIED., .F., .F. ) 
 B_SPLINE_CURVE_WITH_KNOTS ( ( 3, 2, 2, 2, 3 ),
 ( 0.7282608695652174058, 0.7318840579710145233, 0.7391304347826086474, 0.7463768115942028825, 0.7500000000000000000 ),
 .UNSPECIFIED. ) 
 CURVE ( )  GEOMETRIC_REPRESENTATION_ITEM ( )  RATIONAL_B_SPLINE_CURVE ( ( 0.9330127018922194093, 0.9330127018922194093, 1.000000000000000000, 0.8660254037844387076, 1.000000000000000000, 0.8660254037844387076, 1.000000000000000000, 0.9330127018922194093, 0.9330127018922194093 ) ) 
 REPRESENTATION_ITEM ( '' )  );
#6634 = CARTESIAN_POINT ( 'NONE',  ( -13.04141134922759804, 4.372686282101438948, -8.927990412390657937 ) ) ;
#6635 = FACE_OUTER_BOUND ( 'NONE', #13357, .T. ) ;
#6636 = CARTESIAN_POINT ( 'NONE',  ( 26.75643035624999655, 241.9093750006145171, -3.323476615752271712 ) ) ;
#6637 = EDGE_LOOP ( 'NONE', ( #9950, #8508, #17913, #32330 ) ) ;
#6638 = CARTESIAN_POINT ( 'NONE',  ( 31.26013745332475224, -7.209453229046475009, 167.2739077250314779 ) ) ;
#6639 = CARTESIAN_POINT ( 'NONE',  ( 15.24356964374999990, 0.000000000000000000, -2.840624999385477079 ) ) ;
#6641 = EDGE_CURVE ( 'NONE', #34104, #16979, #1355, .T. ) ;
#6640 = CARTESIAN_POINT ( 'NONE',  ( 24.00000000000000000, 242.5000000000000000, 5.196152422706629359 ) ) ;
#6642 = CARTESIAN_POINT ( 'NONE',  ( 19.56230152254411792, 5.196152422706637353, -7.800000000000029132 ) ) ;
#6643 = LINE ( 'NONE', #9303, #32432 ) ;
#6644 = CARTESIAN_POINT ( 'NONE',  ( -20.80759054502876282, 194.7557263913445809, -17.45964060548497088 ) ) ;
#6645 = CARTESIAN_POINT ( 'NONE',  ( 3.474262827703532341, 27.76481371789854791, -8.843639120294245259 ) ) ;
#6646 = CARTESIAN_POINT ( 'NONE',  ( -27.24356964374999279, 197.6468750006145285, 15.72908226750539384 ) ) ;
#6648 = ORIENTED_EDGE ( 'NONE', *, *, #4990, .F. ) ;
#6647 = ORIENTED_EDGE ( 'NONE', *, *, #12890, .T. ) ;
#6649 = CARTESIAN_POINT ( 'NONE',  ( 21.00000000000000000, 246.0343750006144887, -6.646953231504538984 ) ) ;
#6650 = CARTESIAN_POINT ( 'NONE',  ( 4.622313124798831829, 18.56481371789855928, -11.61527771782809282 ) ) ;
#6651 = CARTESIAN_POINT ( 'NONE',  ( 15.24356964374999990, 0.000000000000000000, -2.390624999385471128 ) ) ;
#6652 = CARTESIAN_POINT ( 'NONE',  ( 11.08355503943118769, 131.8398137178985792, 10.83675517735179028 ) ) ;
#6653 = CARTESIAN_POINT ( 'NONE',  ( 18.00000000000000000, 5.196152422706630247, -8.118749998770963927 ) ) ;
#6654 = CARTESIAN_POINT ( 'NONE',  ( 10.56230152254410903, 0.000000000000000000, -7.987499998771019349 ) ) ;
#6655 = ORIENTED_EDGE ( 'NONE', *, *, #4345, .T. ) ;
#6656 = CARTESIAN_POINT ( 'NONE',  ( 22.80587116629411426, 7.646167579472024665E-16, -7.171874999385541294 ) ) ;
#6657 = VERTEX_POINT ( 'NONE', #19309 ) ;
#6658 = CARTESIAN_POINT ( 'NONE',  ( 27.24356964375000345, 196.8781250006145171, -3.336375036156643733E-15 ) ) ;
#6659 = AXIS2_PLACEMENT_3D ( 'NONE', #28128, #33129, #2712 ) ;
#6660 = CARTESIAN_POINT ( 'NONE',  ( 37.28548217858939040, -3.604726614523238837, 164.5069853552165284 ) ) ;
#6661 = CARTESIAN_POINT ( 'NONE',  ( -66.62127896937849414, 218.5309553116392465, 2.162041339862725842 ) ) ;
#6662 = CARTESIAN_POINT ( 'NONE',  ( 20.99999999999999645, 248.9593750006145285, 6.646953231504538984 ) ) ;
#6663 = LINE ( 'NONE', #30165, #51 ) ;
#6664 = CARTESIAN_POINT ( 'NONE',  ( -39.30877896937850124, 211.0902445701383101, -4.530955311639234040 ) ) ;
#6665 = CARTESIAN_POINT ( 'NONE',  ( -33.37872103062156981, 203.4690446883607535, 1.626142955000567936 ) ) ;
#6666 = CARTESIAN_POINT ( 'NONE',  ( 31.16208724273364084, 7.209453229046475009, 166.1531886896782737 ) ) ;
#6667 = ORIENTED_EDGE ( 'NONE', *, *, #9927, .F. ) ;
#6668 = CARTESIAN_POINT ( 'NONE',  ( -27.94841835328498902, 207.9074690653111475, 7.739347195566303128 ) ) ;
#6669 = VECTOR ( 'NONE', #1497, 1000.000000000000000 ) ;
#6670 = CARTESIAN_POINT ( 'NONE',  ( 5.770363421893814682, 138.6351862821014720, 14.38691631536207183 ) ) ;
#6671 = CARTESIAN_POINT ( 'NONE',  ( -45.45163769728823411, 217.4189793300686233, -4.149950860017907139 ) ) ;
#6672 =( BOUNDED_CURVE ( )  B_SPLINE_CURVE ( 2, ( #5420, #2951, #2584, #20217, #23059, #23425, #29095, #20590, #26443 ),
 .UNSPECIFIED., .F., .F. ) 
 B_SPLINE_CURVE_WITH_KNOTS ( ( 3, 2, 2, 2, 3 ),
 ( 0.6195652173913043237, 0.6231884057971014412, 0.6304347826086956763, 0.6376811594202898004, 0.6413043478260869179 ),
 .UNSPECIFIED. ) 
 CURVE ( )  GEOMETRIC_REPRESENTATION_ITEM ( )  RATIONAL_B_SPLINE_CURVE ( ( 0.9330127018922194093, 0.9330127018922194093, 1.000000000000000000, 0.8660254037844387076, 1.000000000000000000, 0.8660254037844387076, 1.000000000000000000, 0.9330127018922194093, 0.9330127018922194093 ) ) 
 REPRESENTATION_ITEM ( '' )  );
#6673 = CARTESIAN_POINT ( 'NONE',  ( 9.500000000000005329, 136.9101862821014777, 0.1745138560725188748 ) ) ;
#6674 = EDGE_CURVE ( 'NONE', #3075, #31515, #36643, .T. ) ;
#6675 = CARTESIAN_POINT ( 'NONE',  ( 19.39230484541326760, 249.2486538117967427, 5.999999999999999112 ) ) ;
#6676 = CARTESIAN_POINT ( 'NONE',  ( -10.49813415415989581, 22.77268628210143575, -7.228626920339068285 ) ) ;
#6677 = CARTESIAN_POINT ( 'NONE',  ( 22.56230152254412147, -3.464101615137755275, -6.112500000000051337 ) ) ;
#6679 = EDGE_CURVE ( 'NONE', #2746, #7301, #20797, .T. ) ;
#6678 = ORIENTED_EDGE ( 'NONE', *, *, #1060, .F. ) ;
#6680 = CARTESIAN_POINT ( 'NONE',  ( -32.19122103062156981, 208.3738570449994256, -6.530955311639227823 ) ) ;
#6681 = CARTESIAN_POINT ( 'NONE',  ( -2.908627838312119351, 125.1226862821014691, -15.53471296425195369 ) ) ;
#6682 = FACE_OUTER_BOUND ( 'NONE', #9451, .T. ) ;
#6683 = CARTESIAN_POINT ( 'NONE',  ( -6.840914352312096547, 11.56018628210145316, 6.594114490232313663 ) ) ;
#6684 = AXIS2_PLACEMENT_3D ( 'NONE', #4897, #13820, #8134 ) ;
#6685 = CARTESIAN_POINT ( 'NONE',  ( -1.926257025242585782E-15, 199.2406250006145285, -31.45816453501075927 ) ) ;
#6686 = DIRECTION ( 'NONE',  ( 1.000000000000000000, 0.000000000000000000, 0.000000000000000000 ) ) ;
#6687 = DIRECTION ( 'NONE',  ( 0.000000000000000000, 0.000000000000000000, 1.000000000000000000 ) ) ;
#6688 = CARTESIAN_POINT ( 'NONE',  ( 16.50512534395675601, 3.755008844408135094, -7.999999999999996447 ) ) ;
#6689 = FACE_OUTER_BOUND ( 'NONE', #35120, .T. ) ;
#6690 = CARTESIAN_POINT ( 'NONE',  ( 9.534712964251900402, 66.57731371789853370, 1.715153634034445540 ) ) ;
#6691 = CARTESIAN_POINT ( 'NONE',  ( 0.000000000000000000, 210.0000000000000284, 0.000000000000000000 ) ) ;
#6692 = EDGE_LOOP ( 'NONE', ( #6648, #17752, #23113, #17056 ) ) ;
#6693 = CARTESIAN_POINT ( 'NONE',  ( 15.00000000000000000, 245.1062500012290286, 0.000000000000000000 ) ) ;
#6694 = CARTESIAN_POINT ( 'NONE',  ( -12.46528703574811558, 89.00231371789855928, 2.660918448318004170 ) ) ;
#6695 = CARTESIAN_POINT ( 'NONE',  ( 16.56230152254411081, 7.209453229046482114, -3.909374999385482496 ) ) ;
#6696 = CARTESIAN_POINT ( 'NONE',  ( 18.00000000000000000, 242.7249999999999943, -5.196152422706630247 ) ) ;
#6697 = CARTESIAN_POINT ( 'NONE',  ( 21.00000000000000000, -6.646953231504538984, -3.740624999385479654 ) ) ;
#6698 = CARTESIAN_POINT ( 'NONE',  ( 8.715434833792128799, 46.73981371789854933, -8.962234695871567070 ) ) ;
#6699 = CARTESIAN_POINT ( 'NONE',  ( 27.24356964375000345, 198.7343750006145626, -3.336375036156643733E-15 ) ) ;
#6700 = ORIENTED_EDGE ( 'NONE', *, *, #35373, .F. ) ;
#6701 = ORIENTED_EDGE ( 'NONE', *, *, #32582, .T. ) ;
#6702 = CARTESIAN_POINT ( 'NONE',  ( 18.12178482187500350, -4.985214923628407568, -4.565624999385481608 ) ) ;
#6703 = CARTESIAN_POINT ( 'NONE',  ( 26.75643035624999655, 243.6718750006145058, -7.049594010296217766E-16 ) ) ;
#6704 = CARTESIAN_POINT ( 'NONE',  ( 4.622313124798573369, 28.23518628210144854, 11.61527771782819940 ) ) ;
#6705 = CARTESIAN_POINT ( 'NONE',  ( -32.18377896937850124, 208.3738570449995109, 6.530955311639247363 ) ) ;
#6706 = CARTESIAN_POINT ( 'NONE',  ( 13.44051670066911619, -5.407089921784859143, -1.415624999385550753 ) ) ;
#6707 = CARTESIAN_POINT ( 'NONE',  ( -62.26711230271183695, 216.4690446883607535, -1.857196546604089393 ) ) ;
#6708 =( NAMED_UNIT ( * ) PLANE_ANGLE_UNIT ( ) SI_UNIT ( $, .RADIAN. ) );
#6709 = CARTESIAN_POINT ( 'NONE',  ( 30.59584727662355164, 6.928203230275506996, 159.6810362611256267 ) ) ;
#6710 = CARTESIAN_POINT ( 'NONE',  ( -10.69584247140429412, 90.15231371789856496, -6.932735513424201024 ) ) ;
#6711 = CARTESIAN_POINT ( 'NONE',  ( -52.77455436395490551, 206.6211998817774997, 3.209657149897401585 ) ) ;
#6712 = EDGE_CURVE ( 'NONE', #4681, #15950, #10043, .T. ) ;
#6713 = CARTESIAN_POINT ( 'NONE',  ( -34.96205436395489841, 216.1378603801730094, 6.307003348497944195 ) ) ;
#6714 = CARTESIAN_POINT ( 'NONE',  ( 26.75643035624999655, 3.323476615752271268, -7.190624999385489602 ) ) ;
#6715 = CARTESIAN_POINT ( 'NONE',  ( 15.00000000000000000, 0.000000000000000000, -2.250000000000001776 ) ) ;
#6716 = CARTESIAN_POINT ( 'NONE',  ( -14.38691631536193860, 53.06481371789855928, -5.770363421894132649 ) ) ;
#6717 = CARTESIAN_POINT ( 'NONE',  ( -56.52752896937850124, 214.3500491399821897, 7.303452534266821949 ) ) ;
#6718 = CARTESIAN_POINT ( 'NONE',  ( -20.77649301497164913, 194.9291638889422700, -17.43354668227102167 ) ) ;
#6719 = CARTESIAN_POINT ( 'NONE',  ( -10.49813415415989581, 87.17268628210143788, -7.228626920339068285 ) ) ;
#6720 = EDGE_CURVE ( 'NONE', #20504, #34009, #12669, .T. ) ;
#6721 = CARTESIAN_POINT ( 'NONE',  ( 0.1745138560725837118, 33.41018628210144925, -15.50000000000000533 ) ) ;
#6722 = CARTESIAN_POINT ( 'NONE',  ( 19.56230152254412147, 5.196152422706637353, -0.6000000000000171863 ) ) ;
#6723 = CARTESIAN_POINT ( 'NONE',  ( 36.81484116775207127, -3.604726614523238837, 159.1275339855211257 ) ) ;
#6724 = VECTOR ( 'NONE', #35653, 1000.000000000000000 ) ;
#6725 = CARTESIAN_POINT ( 'NONE',  ( 13.23911966647218996, 53.24768628210144783, -8.632099005475504683 ) ) ;
#6726 = CARTESIAN_POINT ( 'NONE',  ( 5.778771075727756162E-15, 197.6656250006145399, 31.45816453501076637 ) ) ;
#6727 = LINE ( 'NONE', #12980, #1112 ) ;
#6728 = CARTESIAN_POINT ( 'NONE',  ( 20.99999999999999645, -6.928203230275506996, -1.181249998770955045 ) ) ;
#6729 = CARTESIAN_POINT ( 'NONE',  ( -32.78497103062156981, 204.4285982733020148, -3.350049139982115509 ) ) ;
#6730 = DIRECTION ( 'NONE',  ( 0.000000000000000000, 0.000000000000000000, 1.000000000000000000 ) ) ;
#6731 = CARTESIAN_POINT ( 'NONE',  ( -12.50000000000000355, 12.71018628210143753, -0.1745138560725492671 ) ) ;
#6732 = CARTESIAN_POINT ( 'NONE',  ( 22.56230152254410370, 0.000000000000000000, -10.00000000000000000 ) ) ;
#6733 = CARTESIAN_POINT ( 'NONE',  ( 9.465287035748106703, 130.4023137178985792, -2.064181346179063237 ) ) ;
#6734 = CARTESIAN_POINT ( 'NONE',  ( 20.99999999999999645, 247.0468750006145058, -6.646953231504538984 ) ) ;
#6735 = EDGE_LOOP ( 'NONE', ( #29915, #16615, #5200, #31531 ) ) ;
#6736 = CARTESIAN_POINT ( 'NONE',  ( 15.00000000000000000, 0.000000000000000000, -7.200000000000011724 ) ) ;
#6737 = FACE_OUTER_BOUND ( 'NONE', #11257, .T. ) ;
#6738 = CARTESIAN_POINT ( 'NONE',  ( 13.44051670066911086, 5.407089921784856479, -7.415624999385555860 ) ) ;
#6739 = CARTESIAN_POINT ( 'NONE',  ( 37.32960477335537774, -3.604726614523235284, 165.0113089211254760 ) ) ;
#6740 = DIRECTION ( 'NONE',  ( 0.000000000000000000, 0.000000000000000000, 1.000000000000000000 ) ) ;
#6741 = CARTESIAN_POINT ( 'NONE',  ( 13.49999999999999645, 199.4000000000000341, -23.38268590217984766 ) ) ;
#6742 = CARTESIAN_POINT ( 'NONE',  ( 12.46528703574805874, 45.19768628210144357, 2.660918448318279950 ) ) ;
#6743 = ORIENTED_EDGE ( 'NONE', *, *, #30770, .F. ) ;
#6744 = EDGE_LOOP ( 'NONE', ( #31559, #31724, #15749, #3286 ) ) ;
#6745 = CARTESIAN_POINT ( 'NONE',  ( 0.000000000000000000, 195.0000000000000000, 0.000000000000000000 ) ) ;
#6746 = CARTESIAN_POINT ( 'NONE',  ( -27.24356964375000345, 199.8312500006145171, 0.000000000000000000 ) ) ;
#6747 = CARTESIAN_POINT ( 'NONE',  ( 36.55994210376140785, -3.464101615138027057, 159.0086725999260011 ) ) ;
#6748 = CARTESIAN_POINT ( 'NONE',  ( 26.99999999999999645, 243.0249999999999773, -7.347880794884117764E-16 ) ) ;
#6749 = CARTESIAN_POINT ( 'NONE',  ( 23.87821517812499650, 4.985214923628404904, -9.290624999385460825 ) ) ;
#6750 = CARTESIAN_POINT ( 'NONE',  ( -4.622313124798576922, 88.03518628210144925, -11.61527771782819762 ) ) ;
#6751 = CARTESIAN_POINT ( 'NONE',  ( -0.1745138560722442889, 27.18981371789855572, -15.50000000000000533 ) ) ;
#6752 = CARTESIAN_POINT ( 'NONE',  ( 30.77233765568754720, -6.928203230275506996, 161.6983305247614453 ) ) ;
#6753 = CARTESIAN_POINT ( 'NONE',  ( 19.95279056986857569, 210.3927035363166169, 5.999999999999996447 ) ) ;
#6754 = CARTESIAN_POINT ( 'NONE',  ( -33.97247103062156270, 207.6499508600178387, 3.839350919129076445 ) ) ;
#6755 = FACE_OUTER_BOUND ( 'NONE', #29597, .T. ) ;
#6756 = CARTESIAN_POINT ( 'NONE',  ( 25.21678537267883868, 0.000000000000000000, 167.0403568332661450 ) ) ;
#6757 = CARTESIAN_POINT ( 'NONE',  ( 2.660918448318002838, 141.9023137178985792, 12.46528703574811558 ) ) ;
#6758 = CARTESIAN_POINT ( 'NONE',  ( -52.97247103062156981, 206.6499508600178672, 5.571401726697986057 ) ) ;
#6759 = CARTESIAN_POINT ( 'NONE',  ( -68.80580436395490551, 218.5000000000000000, 0.1155267958017064944 ) ) ;
#6760 = APPLICATION_PROTOCOL_DEFINITION ( 'draft international standard', 'automotive_design', 1998, #3496 ) ;
#6761 = CARTESIAN_POINT ( 'NONE',  ( -27.24356964374999990, 197.9656250006145228, -15.72908226750537786 ) ) ;
#6762 = CARTESIAN_POINT ( 'NONE',  ( -11.08355503943118592, 118.0398137178985536, -10.83675517735179383 ) ) ;
#6763 = CARTESIAN_POINT ( 'NONE',  ( -61.07961230271182274, 211.8571965466040297, 6.469044688360755302 ) ) ;
#6764 = ORIENTED_EDGE ( 'NONE', *, *, #35521, .T. ) ;
#6765 = CARTESIAN_POINT ( 'NONE',  ( -12.46528703574805697, 31.39768628210144641, -2.660918448318280838 ) ) ;
#6766 = DIRECTION ( 'NONE',  ( 0.000000000000000000, 1.000000000000000000, 0.000000000000000000 ) ) ;
#6767 = CARTESIAN_POINT ( 'NONE',  ( -26.99999999999999645, 197.7874999999999943, 15.58845726811991561 ) ) ;
#6768 = CARTESIAN_POINT ( 'NONE',  ( 37.48485094012463748, 7.646167579472024665E-16, 166.7857807271014394 ) ) ;
#6769 = CARTESIAN_POINT ( 'NONE',  ( -2.908627838312119351, 97.52268628210144641, -15.53471296425195369 ) ) ;
#6770 = CARTESIAN_POINT ( 'NONE',  ( -66.43080436395490551, 203.5000000000000000, -0.1155267958017335561 ) ) ;
#6771 = CARTESIAN_POINT ( 'NONE',  ( 19.68408634441911076, 5.407089921784857367, -5.240624999385545379 ) ) ;
#6772 = CARTESIAN_POINT ( 'NONE',  ( 5.233372021372432847, 55.54768628210144499, 8.152565276336710909 ) ) ;
#6773 = DIRECTION ( 'NONE',  ( 0.000000000000000000, 0.000000000000000000, 1.000000000000000000 ) ) ;
#6774 = CARTESIAN_POINT ( 'NONE',  ( -43.07663769728824121, 202.5810206699313767, 4.149950860017909804 ) ) ;
#6775 = DIRECTION ( 'NONE',  ( 0.000000000000000000, 1.000000000000000000, 0.000000000000000000 ) ) ;
#6776 = CARTESIAN_POINT ( 'NONE',  ( -11.48171059495397373, 77.68518628210145494, -4.944772684328680334 ) ) ;
#6777 = CARTESIAN_POINT ( 'NONE',  ( 24.69711925643884598, 0.000000000000000000, 161.1005459446697614 ) ) ;
#6778 = CYLINDRICAL_SURFACE ( 'NONE', #14750, 5.999999999999999112 ) ;
#6780 = CARTESIAN_POINT ( 'NONE',  ( 18.00000000000000000, 5.196152422706630247, -5.475000000000007638 ) ) ;
#6779 = CARTESIAN_POINT ( 'NONE',  ( 7.954856959092191815, 45.77268628210144641, 5.529263428287477744 ) ) ;
#6781 = CARTESIAN_POINT ( 'NONE',  ( 22.60769515458672174, 244.7888461906613600, 6.000000000000004441 ) ) ;
#6782 = AXIS2_PLACEMENT_3D ( 'NONE', #30033, #1030, #35711 ) ;
#6783 = CARTESIAN_POINT ( 'NONE',  ( 26.75643035624999655, -3.323476615752267715, -9.853124999385466154 ) ) ;
#6784 = CARTESIAN_POINT ( 'NONE',  ( -27.00000000000000355, 198.3125000012290400, 0.000000000000000000 ) ) ;
#6785 = CARTESIAN_POINT ( 'NONE',  ( 34.17230835010118994, -5.407089921784861808, 164.7417095288869859 ) ) ;
#6786 = CARTESIAN_POINT ( 'NONE',  ( 25.00761158997735478, 3.464101615137757051, 164.6494895566215746 ) ) ;
#6787 = CARTESIAN_POINT ( 'NONE',  ( 26.99999999999999645, 245.3124999999999716, -3.464101615137755275 ) ) ;
#6788 = CARTESIAN_POINT ( 'NONE',  ( 27.24356964375000345, 195.5281250006145228, -3.336375036156643733E-15 ) ) ;
#6789 = CARTESIAN_POINT ( 'NONE',  ( 11.48171059495408208, 111.7148137178985650, -4.944772684328420986 ) ) ;
#6790 = CARTESIAN_POINT ( 'NONE',  ( -0.1745138560725500443, 102.4101862821014493, 12.50000000000000355 ) ) ;
#6791 = EDGE_LOOP ( 'NONE', ( #14276, #11914, #34935, #8057 ) ) ;
#6792 = ORIENTED_EDGE ( 'NONE', *, *, #22356, .T. ) ;
#6793 = CARTESIAN_POINT ( 'NONE',  ( 13.62178482187501416, 196.8031250006145285, 23.59362340125806767 ) ) ;
#6794 = CARTESIAN_POINT ( 'NONE',  ( 15.24356964374999990, 240.7468750006144944, 0.000000000000000000 ) ) ;
#6795 = CARTESIAN_POINT ( 'NONE',  ( 6.092822981423662299, 77.21481371789855075, 14.25334919248795096 ) ) ;
#6796 = EDGE_CURVE ( 'NONE', #8155, #18512, #36709, .T. ) ;
#6797 = CARTESIAN_POINT ( 'NONE',  ( 26.75643035624999655, -3.323476615752267715, -6.815624999385487826 ) ) ;
#6798 = CARTESIAN_POINT ( 'NONE',  ( 23.87821517812499650, 246.1093750006145342, -4.985214923628404904 ) ) ;
#6799 = CARTESIAN_POINT ( 'NONE',  ( -9.534712964251941258, 104.4226862821014521, 1.715153634034234154 ) ) ;
#6800 = CARTESIAN_POINT ( 'NONE',  ( -27.00000000000000355, 195.1250000012290400, -15.58845726811989429 ) ) ;
#6801 = CARTESIAN_POINT ( 'NONE',  ( -6.840914352311947333, 53.63981371789855501, -6.594114490232462877 ) ) ;
#6802 = CARTESIAN_POINT ( 'NONE',  ( 22.80587116629411071, -3.604726614523235284, -5.353124999385542537 ) ) ;
#6803 = CARTESIAN_POINT ( 'NONE',  ( 5.233372021372610483, 120.0523137178985280, -8.152565276336593669 ) ) ;
#6804 = CARTESIAN_POINT ( 'NONE',  ( 15.24356964375000167, 239.8843750006145115, 3.323476615752272600 ) ) ;
#6805 = CARTESIAN_POINT ( 'NONE',  ( -11.61527771782809282, 25.46481371789855075, -4.622313124798832717 ) ) ;
#6806 = CARTESIAN_POINT ( 'NONE',  ( 6.000769315822030740E-16, 143.0000000000000000, -4.899999999999999467 ) ) ;
#6807 = CARTESIAN_POINT ( 'NONE',  ( 10.69584247140445221, 80.84768628210144925, -6.932735513423970097 ) ) ;
#6808 = CARTESIAN_POINT ( 'NONE',  ( 22.56230152254410370, -3.464101615137751278, -6.449999998771025922 ) ) ;
#6809 = EDGE_CURVE ( 'NONE', #1170, #35303, #134, .T. ) ;
#6810 = LINE ( 'NONE', #7201, #35876 ) ;
#6811 = CARTESIAN_POINT ( 'NONE',  ( 27.89856975800574546, 5.407089921784856479, 164.6694770091404223 ) ) ;
#6812 = CARTESIAN_POINT ( 'NONE',  ( -11.08355503943142573, 85.16018628210146346, 10.83675517735155402 ) ) ;
#6813 = CARTESIAN_POINT ( 'NONE',  ( 16.56230152254411436, -7.209453229046482114, -5.034374999385487826 ) ) ;
#6814 = CARTESIAN_POINT ( 'NONE',  ( -47.00000000000000711, 244.5000000000000000, 5.000000000000000888 ) ) ;
#6815 = DIRECTION ( 'NONE',  ( 0.9961946980917462113, 0.000000000000000000, -0.08715574274765118534 ) ) ;
#6816 = CARTESIAN_POINT ( 'NONE',  ( 6.840914352312096547, 117.3601862821014663, -6.594114490232313663 ) ) ;
#6817 = CARTESIAN_POINT ( 'NONE',  ( 22.56230152254410015, 7.347880794884117764E-16, -7.762499998770988618 ) ) ;
#6818 = EDGE_CURVE ( 'NONE', #10561, #6368, #14952, .T. ) ;
#6819 = CARTESIAN_POINT ( 'NONE',  ( -11.61527771782819940, 131.7351862821014663, 4.622313124798574258 ) ) ;
#6820 = CARTESIAN_POINT ( 'NONE',  ( -20.86978606573367045, 194.8588513912095550, -17.51182790300216752 ) ) ;
#6821 = CARTESIAN_POINT ( 'NONE',  ( 15.24356964374999990, 239.8093750006145228, -3.323476615752268604 ) ) ;
#6822 = VERTEX_POINT ( 'NONE', #17374 ) ;
#6823 = CARTESIAN_POINT ( 'NONE',  ( 34.29487111334006499, -5.407089921784855591, 166.1426083230784911 ) ) ;
#6824 = CARTESIAN_POINT ( 'NONE',  ( 26.75643035624999655, -3.323476615752267715, -2.653124999385471305 ) ) ;
#6825 = CARTESIAN_POINT ( 'NONE',  ( -13.62178482187500528, 199.7843750006145456, -23.59362340125807123 ) ) ;
#6826 = CYLINDRICAL_SURFACE ( 'NONE', #2745, 7.500000000000000000 ) ;
#6827 = DIRECTION ( 'NONE',  ( -0.000000000000000000, 1.000000000000000000, -0.000000000000000000 ) ) ;
#6828 = CARTESIAN_POINT ( 'NONE',  ( 10.56230152254410903, 7.347880794884117764E-16, -10.00000000000000000 ) ) ;
#6829 = VECTOR ( 'NONE', #4272, 1000.000000000000000 ) ;
#6830 = CARTESIAN_POINT ( 'NONE',  ( -100.7560012262353411, 61.79101779669657191, 5.000000000000000000 ) ) ;
#6831 = CARTESIAN_POINT ( 'NONE',  ( -2.064181346179062349, 17.70231371789854435, -9.465287035748106703 ) ) ;
#6832 = CARTESIAN_POINT ( 'NONE',  ( -27.24356964375000345, 197.6093750006145342, 0.000000000000000000 ) ) ;
#6834 = ORIENTED_EDGE ( 'NONE', *, *, #25880, .T. ) ;
#6833 = EDGE_LOOP ( 'NONE', ( #5107, #6869, #12376, #22734 ) ) ;
#6835 = CARTESIAN_POINT ( 'NONE',  ( 15.24356964374999990, 246.1093750006145342, -3.323476615752268604 ) ) ;
#6836 = CARTESIAN_POINT ( 'NONE',  ( -2.660918448318005058, 17.70231371789854435, -12.46528703574811558 ) ) ;
#6837 = CARTESIAN_POINT ( 'NONE',  ( 26.75643035624999655, 7.049594010296217766E-16, -2.615624999385474325 ) ) ;
#6838 = CARTESIAN_POINT ( 'NONE',  ( -8.632099005475794229, 124.6523137178985650, 13.23911966647199812 ) ) ;
#6839 =( BOUNDED_CURVE ( )  B_SPLINE_CURVE ( 2, ( #30124, #21421, #10217, #13067, #15917, #19142, #1492, #12685, #33155 ),
 .UNSPECIFIED., .F., .F. ) 
 B_SPLINE_CURVE_WITH_KNOTS ( ( 3, 2, 2, 2, 3 ),
 ( 0.6875000000000000000, 0.6944444444444444198, 0.7083333333333333703, 0.7222222222222222099, 0.7291666666666667407 ),
 .UNSPECIFIED. ) 
 CURVE ( )  GEOMETRIC_REPRESENTATION_ITEM ( )  RATIONAL_B_SPLINE_CURVE ( ( 0.9330127018922194093, 0.9330127018922194093, 1.000000000000000000, 0.8660254037844387076, 1.000000000000000000, 0.8660254037844387076, 1.000000000000000000, 0.9330127018922187432, 0.9330127018922192983 ) ) 
 REPRESENTATION_ITEM ( '' )  );
#6840 = CARTESIAN_POINT ( 'NONE',  ( 15.00000000000000000, 3.464101615137752166, -9.431249998770962151 ) ) ;
#6841 = AXIS2_PLACEMENT_3D ( 'NONE', #36089, #12604, #35901 ) ;
#6842 = CARTESIAN_POINT ( 'NONE',  ( 19.56230152254410370, 5.196152422706631135, -8.137499998771001941 ) ) ;
#6843 = ORIENTED_EDGE ( 'NONE', *, *, #19169, .F. ) ;
#6844 = CARTESIAN_POINT ( 'NONE',  ( 16.56230152254411436, -7.209453229046482114, -5.034374999385487826 ) ) ;
#6845 = PRESENTATION_LAYER_ASSIGNMENT (  '', '', ( #6872 ) ) ;
#6846 = CARTESIAN_POINT ( 'NONE',  ( -1.926257025242585782E-15, 197.4406250006145740, -31.45816453501075927 ) ) ;
#6847 = EDGE_CURVE ( 'NONE', #27888, #17896, #14521, .T. ) ;
#6848 = CARTESIAN_POINT ( 'NONE',  ( 10.49813415415989581, 128.5726862821014720, 7.228626920339068285 ) ) ;
#6849 = VECTOR ( 'NONE', #13997, 1000.000000000000000 ) ;
#6850 = CARTESIAN_POINT ( 'NONE',  ( 31.07874456373121319, 7.209453229046482114, 165.2005775096280615 ) ) ;
#6851 = CARTESIAN_POINT ( 'NONE',  ( -61.07961230271182984, 212.3930949314663792, 8.469044688360751749 ) ) ;
#6852 = CARTESIAN_POINT ( 'NONE',  ( 15.24356964374999990, 246.5593750006144944, -3.323476615752268604 ) ) ;
#6853 =( LENGTH_UNIT ( ) NAMED_UNIT ( * ) SI_UNIT ( .MILLI., .METRE. ) );
#6854 = CARTESIAN_POINT ( 'NONE',  ( 1.120210788295102201E-13, 197.1875000000000568, -27.00000000000000711 ) ) ;
#6855 = EDGE_CURVE ( 'NONE', #19498, #35111, #14874, .T. ) ;
#6856 = CARTESIAN_POINT ( 'NONE',  ( -47.62127896937850124, 214.5309553116392749, 1.090244570138288127 ) ) ;
#6857 = CARTESIAN_POINT ( 'NONE',  ( 15.00000000000000178, 245.9875000000000398, 3.464101615137757051 ) ) ;
#6858 = CARTESIAN_POINT ( 'NONE',  ( 24.95534962787547073, -3.604726614523240613, 166.8467808440897500 ) ) ;
#6859 = ORIENTED_EDGE ( 'NONE', *, *, #26272, .T. ) ;
#6860 =( BOUNDED_CURVE ( )  B_SPLINE_CURVE ( 2, ( #11139, #34071, #28199, #24797, #19692, #24975, #25173 ),
 .UNSPECIFIED., .F., .F. ) 
 B_SPLINE_CURVE_WITH_KNOTS ( ( 3, 2, 2, 3 ),
 ( 0.06521739130434746345, 0.07246376811594175404, 0.07971014492753603076, 0.08695652173913032135 ),
 .UNSPECIFIED. ) 
 CURVE ( )  GEOMETRIC_REPRESENTATION_ITEM ( )  RATIONAL_B_SPLINE_CURVE ( ( 1.000000000000006661, 0.8660254037844320463, 1.000000000000000000, 0.8660254037844387076, 1.000000000000000000, 0.8660254037844407060, 0.9999999999999980016 ) ) 
 REPRESENTATION_ITEM ( '' )  );
#6861 = CARTESIAN_POINT ( 'NONE',  ( 15.00000000000000178, 248.6875000000000000, 3.464101615137757051 ) ) ;
#6862 = CARTESIAN_POINT ( 'NONE',  ( -0.1745138560725817967, 130.0101862821014436, 15.50000000000000533 ) ) ;
#6863 = CARTESIAN_POINT ( 'NONE',  ( -53.36830436395490551, 209.8844732041983150, 8.500000000000003553 ) ) ;
#6864 = ADVANCED_FACE ( 'NONE', ( #17001 ), #28916, .T. ) ;
#6865 = CARTESIAN_POINT ( 'NONE',  ( 1.715153634034233487, 120.5226862821014322, 9.534712964251941258 ) ) ;
#6866 = CARTESIAN_POINT ( 'NONE',  ( 19.39230484541324984, 246.5486538117966973, 5.999999999999991118 ) ) ;
#6867 = CARTESIAN_POINT ( 'NONE',  ( -10.69584247140444866, 39.44768628210145067, 6.932735513423972762 ) ) ;
#6868 = CARTESIAN_POINT ( 'NONE',  ( 10.56230152254410726, -3.464101615137761048, -7.162500000000031619 ) ) ;
#6869 = ORIENTED_EDGE ( 'NONE', *, *, #4577, .T. ) ;
#6870 = CARTESIAN_POINT ( 'NONE',  ( -33.37872103062156981, 203.4690446883607535, 1.626142955000567936 ) ) ;
#6871 = CARTESIAN_POINT ( 'NONE',  ( 6.092822981423978490, 116.7851862821014635, -14.25334919248782306 ) ) ;
#6872 = STYLED_ITEM ( 'NONE', ( #5159 ), #5631 ) ;
#6873 = CARTESIAN_POINT ( 'NONE',  ( -73.23181873377778572, 221.0662276635146384, 0.4999999999999995559 ) ) ;
#6874 = CARTESIAN_POINT ( 'NONE',  ( -3.796722387233185003, 137.0148137178985621, -8.710071997420207879 ) ) ;
#6875 = CARTESIAN_POINT ( 'NONE',  ( 27.24356964374999635, 198.2656250006145058, -15.72908226750539029 ) ) ;
#6876 = DIRECTION ( 'NONE',  ( 1.000000000000000000, 0.000000000000000000, 0.000000000000000000 ) ) ;
#6877 = CARTESIAN_POINT ( 'NONE',  ( 26.99999999999999645, 196.6625000000000227, -15.58845726811990495 ) ) ;
#6878 = CARTESIAN_POINT ( 'NONE',  ( 25.22171936664797798, 0.000000000000000000, 169.8914008901326724 ) ) ;
#6879 = CARTESIAN_POINT ( 'NONE',  ( 27.75760683848089982, 5.196152422706636465, 161.6609393423525205 ) ) ;
#6880 = ADVANCED_FACE ( 'NONE', ( #23612 ), #25708, .T. ) ;
#6881 = CARTESIAN_POINT ( 'NONE',  ( -9.465287035748106703, 79.80231371789852801, 2.064181346179061460 ) ) ;
#6882 = CYLINDRICAL_SURFACE ( 'NONE', #7660, 28.99999999999999645 ) ;
#6883 = ORIENTED_EDGE ( 'NONE', *, *, #3843, .F. ) ;
#6884 = CARTESIAN_POINT ( 'NONE',  ( 18.00000000000000355, 242.9312500012290457, 5.196152422706632912 ) ) ;
#6885 = CARTESIAN_POINT ( 'NONE',  ( -10.49813415416004858, 88.42731371789858485, 7.228626920338840023 ) ) ;
#6886 = CARTESIAN_POINT ( 'NONE',  ( 22.80587116629412847, -3.604726614523238837, -3.159374999385510474 ) ) ;
#6887 = CARTESIAN_POINT ( 'NONE',  ( -7.856644100452656154, 143.0000000000000568, 10.55002382876331524 ) ) ;
#6888 = CARTESIAN_POINT ( 'NONE',  ( 26.75643035624999655, -3.323476615752267715, -5.015624999385472904 ) ) ;
#6889 = CARTESIAN_POINT ( 'NONE',  ( -11.61527771782809282, 43.86481371789854933, -4.622313124798832717 ) ) ;
#6890 = AXIS2_PLACEMENT_3D ( 'NONE', #32831, #9152, #6876 ) ;
#6891 = APPLICATION_CONTEXT ( 'automotive_design' ) ;
#6892 = ORIENTED_EDGE ( 'NONE', *, *, #36787, .F. ) ;
#6893 = CARTESIAN_POINT ( 'NONE',  ( 15.24356964375000167, -3.323476615752272600, -6.403124999385489069 ) ) ;
#6894 = CARTESIAN_POINT ( 'NONE',  ( 23.87821517812500005, 243.5968750006145171, 4.985214923628404016 ) ) ;
#6895 = CARTESIAN_POINT ( 'NONE',  ( 11.61527771782819940, 16.73518628210143788, -4.622313124798573369 ) ) ;
#6896 = EDGE_CURVE ( 'NONE', #212, #21530, #20034, .T. ) ;
#6897 = CARTESIAN_POINT ( 'NONE',  ( -36.93377896937850124, 208.3738570449995109, 6.530955311639247363 ) ) ;
#6898 = CARTESIAN_POINT ( 'NONE',  ( -51.97544563604516554, 214.8429017333602360, 4.673758765035156415 ) ) ;
#6899 = VECTOR ( 'NONE', #22643, 1000.000000000000000 ) ;
#6900 =( NAMED_UNIT ( * ) PLANE_ANGLE_UNIT ( ) SI_UNIT ( $, .RADIAN. ) );
#6901 =( BOUNDED_CURVE ( )  B_SPLINE_CURVE ( 2, ( #16334, #14044, #25228, #16150, #33577, #7802, #24855, #10822, #27882 ),
 .UNSPECIFIED., .F., .F. ) 
 B_SPLINE_CURVE_WITH_KNOTS ( ( 3, 2, 2, 2, 3 ),
 ( 0.5108695652173913526, 0.5144927536231883591, 0.5217391304347825942, 0.5289855072463768293, 0.5326086956521739468 ),
 .UNSPECIFIED. ) 
 CURVE ( )  GEOMETRIC_REPRESENTATION_ITEM ( )  RATIONAL_B_SPLINE_CURVE ( ( 0.9330127018922192983, 0.9330127018922202975, 1.000000000000000000, 0.8660254037844387076, 1.000000000000000000, 0.8660254037844387076, 1.000000000000000000, 0.9330127018922194093, 0.9330127018922194093 ) ) 
 REPRESENTATION_ITEM ( '' )  );
#6902 =( GEOMETRIC_REPRESENTATION_CONTEXT ( 3 ) GLOBAL_UNCERTAINTY_ASSIGNED_CONTEXT ( ( #18444 ) ) GLOBAL_UNIT_ASSIGNED_CONTEXT ( ( #20330, #31871, #2502 ) ) REPRESENTATION_CONTEXT ( 'NONE', 'WORKASPACE' ) );
#6903 = CARTESIAN_POINT ( 'NONE',  ( 24.66770419336863185, 0.000000000000000000, 160.7643302352881278 ) ) ;
#6904 = CARTESIAN_POINT ( 'NONE',  ( 2.311890736173452865, 82.67731371789855643, -12.53471296425189152 ) ) ;
#6905 = CARTESIAN_POINT ( 'NONE',  ( -53.36830436395490551, 209.8844732041982297, 4.499999999999996447 ) ) ;
#6906 = AXIS2_PLACEMENT_3D ( 'NONE', #3319, #14890, #285 ) ;
#6907 = CARTESIAN_POINT ( 'NONE',  ( -67.42038769728823411, 208.1428034533959703, 6.469044688360770401 ) ) ;
#6908 = CARTESIAN_POINT ( 'NONE',  ( 23.87821517812500005, -4.985214923628404016, -7.753124999385491378 ) ) ;
#6909 = DIRECTION ( 'NONE',  ( 0.000000000000000000, 0.000000000000000000, 1.000000000000000000 ) ) ;
#6910 = CARTESIAN_POINT ( 'NONE',  ( -15.46528703574811736, 52.20231371789854080, 3.257655550456946436 ) ) ;
#6911 = EDGE_CURVE ( 'NONE', #24301, #29694, #6672, .T. ) ;
#6912 = CARTESIAN_POINT ( 'NONE',  ( -41.88169563604517265, 210.1155267958018271, 8.500000000000003553 ) ) ;
#6913 = CARTESIAN_POINT ( 'NONE',  ( 1.069080835302379631E-14, 198.3124999999999716, 27.00000000000000000 ) ) ;
#6914 = CARTESIAN_POINT ( 'NONE',  ( -8.962234695871760692, 94.36018628210145209, 8.715434833791933400 ) ) ;
#6915 = CARTESIAN_POINT ( 'NONE',  ( -3.257655550457281723, 29.09768628210144925, 15.46528703574804986 ) ) ;
#6916 = CARTESIAN_POINT ( 'NONE',  ( 10.56230152254410903, 0.000000000000000000, -5.551115123125782702E-14 ) ) ;
#6917 = CARTESIAN_POINT ( 'NONE',  ( 36.89328133622495898, -3.604726614523238837, 160.0241092138036834 ) ) ;
#6918 = ORIENTED_EDGE ( 'NONE', *, *, #9691, .T. ) ;
#6919 = CARTESIAN_POINT ( 'NONE',  ( 0.1745138560725837118, 42.61018628210144499, -15.50000000000000533 ) ) ;
#6920 = CARTESIAN_POINT ( 'NONE',  ( 13.62178482187501416, 197.7031250006145342, 23.59362340125806767 ) ) ;
#6921 = CARTESIAN_POINT ( 'NONE',  ( 13.62178482187499640, 199.7093750006145285, -23.59362340125807123 ) ) ;
#6922 = CARTESIAN_POINT ( 'NONE',  ( 0.000000000000000000, 210.0000000000000284, -27.00000000000000000 ) ) ;
#6923 = CARTESIAN_POINT ( 'NONE',  ( -34.96205436395488420, 214.6737587650352168, 4.842901733360204908 ) ) ;
#6924 = DIRECTION ( 'NONE',  ( -0.8083506638593009885, -0.5887012860850802110, 0.000000000000000000 ) ) ;
#6925 = CARTESIAN_POINT ( 'NONE',  ( 12.46528703574805874, 26.79768628210144144, 2.660918448318279950 ) ) ;
#6926 = CARTESIAN_POINT ( 'NONE',  ( 18.00000000000000355, 247.4312500012290457, 5.196152422706632912 ) ) ;
#6927 = CARTESIAN_POINT ( 'NONE',  ( -0.1745138560723084320, 137.5898137178985792, -9.500000000000005329 ) ) ;
#6928 = CARTESIAN_POINT ( 'NONE',  ( 26.75643035624999655, 244.6843750006145228, -7.049594010296217766E-16 ) ) ;
#6929 = CIRCLE ( 'NONE', #11758, 3.999999999999996447 ) ;
#6930 = ORIENTED_EDGE ( 'NONE', *, *, #10076, .T. ) ;
#6931 = CARTESIAN_POINT ( 'NONE',  ( 24.00000000000000000, -5.196152422706629359, -6.149999999999988809 ) ) ;
#6932 = CARTESIAN_POINT ( 'NONE',  ( -11.08355503943142573, 94.36018628210146630, 10.83675517735155402 ) ) ;
#6933 = CARTESIAN_POINT ( 'NONE',  ( 23.99999999999999645, 5.196152422706631135, -3.299999999999997158 ) ) ;
#6934 = CARTESIAN_POINT ( 'NONE',  ( 12.53471296425189330, 130.9773137178985678, 2.311890736173451533 ) ) ;
#6935 = ADVANCED_FACE ( 'NONE', ( #3324 ), #9019, .T. ) ;
#6936 = CARTESIAN_POINT ( 'NONE',  ( 19.68408634441910365, -5.407089921784855591, -5.840624999385535254 ) ) ;
#6937 = VECTOR ( 'NONE', #24097, 1000.000000000000000 ) ;
#6938 = CARTESIAN_POINT ( 'NONE',  ( 37.21848120135211957, 3.604726614523238837, 163.7411606810585170 ) ) ;
#6939 = CARTESIAN_POINT ( 'NONE',  ( 26.99999999999995737, 3.464101615137778811, -1.987499999999999156 ) ) ;
#6940 = CARTESIAN_POINT ( 'NONE',  ( -8.147263093523481103, 219.8189111151660029, 2.997147438070004721 ) ) ;
#6941 = EDGE_LOOP ( 'NONE', ( #14617, #571, #29123, #37269 ) ) ;
#6942 = CARTESIAN_POINT ( 'NONE',  ( 10.69584247140445221, 53.24768628210144072, -6.932735513423970097 ) ) ;
#6943 = ORIENTED_EDGE ( 'NONE', *, *, #28922, .F. ) ;
#6944 = ORIENTED_EDGE ( 'NONE', *, *, #28448, .T. ) ;
#6945 = DIRECTION ( 'NONE',  ( 1.000000000000000000, 0.000000000000000000, 0.000000000000000000 ) ) ;
#6946 = CARTESIAN_POINT ( 'NONE',  ( 18.12178482187500350, -4.985214923628407568, -1.415624999385467486 ) ) ;
#6947 = CARTESIAN_POINT ( 'NONE',  ( -47.00000000000000711, 244.5000000000000000, -2.499999999999997780 ) ) ;
#6948 = CARTESIAN_POINT ( 'NONE',  ( -27.00000000000000355, 198.2750000012290172, -15.58845726811989429 ) ) ;
#6949 = CARTESIAN_POINT ( 'NONE',  ( 15.24356964375000167, -3.323476615752272600, -9.553124999385460114 ) ) ;
#6950 = CARTESIAN_POINT ( 'NONE',  ( 7.228626920339068285, 80.27268628210146062, -10.49813415415989581 ) ) ;
#6951 = CARTESIAN_POINT ( 'NONE',  ( -15.50000000000000533, 15.68981371789854329, 0.1745138560722471477 ) ) ;
#6952 = EDGE_CURVE ( 'NONE', #9049, #6180, #8223, .T. ) ;
#6953 = LINE ( 'NONE', #15666, #24840 ) ;
#6954 = CARTESIAN_POINT ( 'NONE',  ( 16.47967912936645263, 222.0541889883434976, 3.964960503605021280 ) ) ;
#6955 = CARTESIAN_POINT ( 'NONE',  ( -61.67336230271184405, 213.9548777149308023, 2.149950860017852960 ) ) ;
#6956 = PRODUCT_DEFINITION ( 'UNKNOWN', '', #6294, #26680 ) ;
#6957 = FACE_OUTER_BOUND ( 'NONE', #25657, .T. ) ;
#6958 = CARTESIAN_POINT ( 'NONE',  ( 28.15961270201155742, 5.196152422706630247, 166.2558873885250250 ) ) ;
#6959 = CARTESIAN_POINT ( 'NONE',  ( 10.69584247140429589, 140.7523137178985735, 6.932735513424201024 ) ) ;
#6960 = CARTESIAN_POINT ( 'NONE',  ( -43.27455436395490551, 205.1570982666397356, 4.673758765035198159 ) ) ;
#6961 = CARTESIAN_POINT ( 'NONE',  ( -67.81622103062157692, 212.1620413398628671, 8.530955311639223382 ) ) ;
#6962 = PRODUCT_CONTEXT ( 'NONE', #26974, 'mechanical' ) ;
#6963 = LINE ( 'NONE', #30069, #2196 ) ;
#6964 = CARTESIAN_POINT ( 'NONE',  ( 5.778771075727756162E-15, 198.5656250006145171, 31.45816453501075927 ) ) ;
#6965 = CARTESIAN_POINT ( 'NONE',  ( 14.25334919248795451, 111.7148137178985792, -6.092822981423661410 ) ) ;
#6966 = CARTESIAN_POINT ( 'NONE',  ( -44.25669563604516554, 209.8844732041982013, -6.500000000000000888 ) ) ;
#6967 = ORIENTED_EDGE ( 'NONE', *, *, #22705, .F. ) ;
#6968 = CARTESIAN_POINT ( 'NONE',  ( 11.48171059495397728, 36.28518628210144925, 4.944772684328674117 ) ) ;
#6969 = LINE ( 'NONE', #24759, #12914 ) ;
#6970 = PLANE ( 'NONE',  #36226 ) ;
#6971 = CARTESIAN_POINT ( 'NONE',  ( 28.12898775289485442, 5.407089921784862696, 167.3031667422204691 ) ) ;
#6972 = CARTESIAN_POINT ( 'NONE',  ( 13.23911966647218996, 108.4476862821014294, -8.632099005475504683 ) ) ;
#6973 = CARTESIAN_POINT ( 'NONE',  ( -56.53497103062156270, 204.4285982733020148, -3.350049139982115509 ) ) ;
#6974 = CARTESIAN_POINT ( 'NONE',  ( 22.80587116629411071, -3.604726614523235284, -5.353124999385542537 ) ) ;
#6975 = CARTESIAN_POINT ( 'NONE',  ( -3.796722387233375073, 47.78518628210144215, 8.710071997420127943 ) ) ;
#6976 = CARTESIAN_POINT ( 'NONE',  ( -89.83814373643217266, 60.44923248139874516, 5.000000000000000000 ) ) ;
#6977 = CARTESIAN_POINT ( 'NONE',  ( -34.17038769728823411, 207.6069050685337913, 8.469044688360781947 ) ) ;
#6978 = CARTESIAN_POINT ( 'NONE',  ( 22.80587116629411781, -3.604726614523238837, -9.909374999385510918 ) ) ;
#6979 =( BOUNDED_CURVE ( )  B_SPLINE_CURVE ( 2, ( #10572, #4693, #36157, #27638, #24791, #7736, #30857 ),
 .UNSPECIFIED., .F., .F. ) 
 B_SPLINE_CURVE_WITH_KNOTS ( ( 3, 2, 2, 3 ),
 ( 0.3695652173913039351, 0.3768115942028982257, 0.3840579710144925163, 0.3913043478260868069 ),
 .UNSPECIFIED. ) 
 CURVE ( )  GEOMETRIC_REPRESENTATION_ITEM ( )  RATIONAL_B_SPLINE_CURVE ( ( 1.000000000000007105, 0.8660254037844313801, 1.000000000000000000, 0.8660254037844387076, 1.000000000000000000, 0.8660254037844418162, 0.9999999999999968914 ) ) 
 REPRESENTATION_ITEM ( '' )  );
#6980 = CARTESIAN_POINT ( 'NONE',  ( -4.944772684328673229, 84.58518628210146062, 11.48171059495397728 ) ) ;
#6981 = CARTESIAN_POINT ( 'NONE',  ( -27.00000000000000355, 200.0000000000000000, 0.000000000000000000 ) ) ;
#6982 = FACE_BOUND ( 'NONE', #30724, .T. ) ;
#6984 = CARTESIAN_POINT ( 'NONE',  ( 13.56230152254410726, 5.196152422706636465, -1.875000000000043299 ) ) ;
#6983 = CARTESIAN_POINT ( 'NONE',  ( 9.500000000000005329, 44.91018628210144215, 0.1745138560725188748 ) ) ;
#6985 = CARTESIAN_POINT ( 'NONE',  ( 30.69144623189632526, 7.209453229046475009, 160.7737373199828426 ) ) ;
#6986 = ORIENTED_EDGE ( 'NONE', *, *, #32567, .T. ) ;
#6987 = CARTESIAN_POINT ( 'NONE',  ( 18.12178482187500350, -4.985214923628407568, -9.965624999385468641 ) ) ;
#6988 = DIRECTION ( 'NONE',  ( -0.000000000000000000, -0.000000000000000000, 1.000000000000000000 ) ) ;
#6989 = CARTESIAN_POINT ( 'NONE',  ( 27.78908035617901717, -5.407089921784865361, 163.4180074196626720 ) ) ;
#6990 = CARTESIAN_POINT ( 'NONE',  ( 24.73960768102833185, -3.464101615137761048, 161.5861908599894718 ) ) ;
#6991 = CARTESIAN_POINT ( 'NONE',  ( 15.00000000000000000, 245.4625000000000057, -3.464101615137752166 ) ) ;
#6992 = CARTESIAN_POINT ( 'NONE',  ( -27.24356964375000345, 197.1031250006145399, 0.000000000000000000 ) ) ;
#6993 = CARTESIAN_POINT ( 'NONE',  ( 10.69584247140429589, 94.75231371789854506, 6.932735513424201024 ) ) ;
#6994 = CARTESIAN_POINT ( 'NONE',  ( 11.61527771782819940, 99.53518628210144925, -4.622313124798573369 ) ) ;
#6995 = ORIENTED_EDGE ( 'NONE', *, *, #36066, .F. ) ;
#6996 = EDGE_LOOP ( 'NONE', ( #26128, #7212, #24838, #35940 ) ) ;
#6997 = CARTESIAN_POINT ( 'NONE',  ( 13.62178482187501416, 196.3531250006145115, 23.59362340125806767 ) ) ;
#6998 = CARTESIAN_POINT ( 'NONE',  ( 18.12178482187500350, 240.8218750006145399, 4.985214923628407568 ) ) ;
#6999 = CARTESIAN_POINT ( 'NONE',  ( 3.257655550456945548, 68.30231371789852801, 15.46528703574811736 ) ) ;
#7000 = CARTESIAN_POINT ( 'NONE',  ( 18.12178482187499640, 4.985214923628404904, -6.178124999385470772 ) ) ;
#7001 = CIRCLE ( 'NONE', #17894, 7.500000000000000000 ) ;
#7002 = CARTESIAN_POINT ( 'NONE',  ( 18.12178482187500350, 244.5343750006145456, 4.985214923628407568 ) ) ;
#7003 = CARTESIAN_POINT ( 'NONE',  ( 8.843639120294328748, 108.7351862821014663, -3.474262827703334722 ) ) ;
#7004 = CARTESIAN_POINT ( 'NONE',  ( 21.00000000000000000, 242.9687500012290684, 5.999999999999998224 ) ) ;
#7005 = CARTESIAN_POINT ( 'NONE',  ( 2.064181346179061460, 59.10231371789854649, 9.465287035748106703 ) ) ;
#7006 = CARTESIAN_POINT ( 'NONE',  ( 13.44051670066911619, -5.407089921784859143, -6.815624999385539340 ) ) ;
#7007 = EDGE_CURVE ( 'NONE', #17676, #3429, #4011, .T. ) ;
#7008 = CARTESIAN_POINT ( 'NONE',  ( 9.534712964251900402, 112.5773137178985479, 1.715153634034445540 ) ) ;
#7009 = DIRECTION ( 'NONE',  ( 0.9961946980917462113, 0.000000000000000000, -0.08715574274765118534 ) ) ;
#7010 = CARTESIAN_POINT ( 'NONE',  ( 10.69584247140429589, 21.15231371789855430, 6.932735513424201024 ) ) ;
#7011 = CARTESIAN_POINT ( 'NONE',  ( -4.622313124798576922, 88.03518628210144925, -11.61527771782819762 ) ) ;
#7012 = CARTESIAN_POINT ( 'NONE',  ( 19.56230152254411081, -5.196152422706629359, -6.037499998771039600 ) ) ;
#7013 = FACE_OUTER_BOUND ( 'NONE', #22463, .T. ) ;
#7014 = CARTESIAN_POINT ( 'NONE',  ( 34.03340388509710834, 5.407089921784857367, 163.1540242288032232 ) ) ;
#7015 = CIRCLE ( 'NONE', #12443, 8.000000000000007105 ) ;
#7016 = CARTESIAN_POINT ( 'NONE',  ( 13.44051670066911086, 5.407089921784862696, -2.971874999385532234 ) ) ;
#7017 = CARTESIAN_POINT ( 'NONE',  ( 22.56230152254458687, 3.464101615137479495, -3.224999998771004961 ) ) ;
#7018 = DIRECTION ( 'NONE',  ( -0.000000000000000000, 1.000000000000000000, -0.000000000000000000 ) ) ;
#7019 = CARTESIAN_POINT ( 'NONE',  ( 20.99999999999999645, -6.928203230275506996, -5.681249998770944387 ) ) ;
#7020 = CARTESIAN_POINT ( 'NONE',  ( -6.840914352312096547, 103.5601862821014407, 6.594114490232313663 ) ) ;
#7021 = CARTESIAN_POINT ( 'NONE',  ( 1.069080835302379631E-14, 198.4250000012290229, 27.00000000000000000 ) ) ;
#7022 = VECTOR ( 'NONE', #9594, 1000.000000000000000 ) ;
#7023 = CARTESIAN_POINT ( 'NONE',  ( -12.46528703574805697, 123.3976862821014606, -2.660918448318280838 ) ) ;
#7024 = CARTESIAN_POINT ( 'NONE',  ( 11.62741699796950989, 213.5147186257614180, 5.999999999999998224 ) ) ;
#7025 = CARTESIAN_POINT ( 'NONE',  ( 26.75643035624999655, 249.2218750006144887, -3.323476615752271712 ) ) ;
#7026 = B_SPLINE_CURVE_WITH_KNOTS ( 'NONE', 3,
 ( #31147, #24706, #36258, #16744, #33614, #30594, #10860, #10301, #7280, #36818, #1769, #21872, #28291, #22433, #8023, #13520 ),
 .UNSPECIFIED., .F., .F.,
 ( 4, 2, 2, 2, 2, 2, 2, 4 ),
 ( 0.000000000000000000, 0.002989157573830781168, 0.004483736360746172836, 0.005978315147661564938, 0.008967472721492300569, 0.01046205150840768747, 0.01120934090186539826, 0.01195663029532311079 ),
 .UNSPECIFIED. ) ;
#7027 = ORIENTED_EDGE ( 'NONE', *, *, #14956, .T. ) ;
#7028 = CARTESIAN_POINT ( 'NONE',  ( 28.06852345636367119, -5.407089921784859143, 166.6120566704193493 ) ) ;
#7029 = CARTESIAN_POINT ( 'NONE',  ( 15.24356964374999990, 0.000000000000000000, -3.290624999385455496 ) ) ;
#7030 = CARTESIAN_POINT ( 'NONE',  ( 26.99999999999999645, 242.5750000000000171, -7.347880794884117764E-16 ) ) ;
#7031 = CARTESIAN_POINT ( 'NONE',  ( 31.16453849805197507, -6.928203230275506996, 166.1812066661742904 ) ) ;
#7032 = CYLINDRICAL_SURFACE ( 'NONE', #29400, 5.999999999999999112 ) ;
#7033 = CARTESIAN_POINT ( 'NONE',  ( 14.99999999999999289, 204.0000000000000000, 0.000000000000000000 ) ) ;
#7034 = CARTESIAN_POINT ( 'NONE',  ( 18.12178482187500350, 243.6343750006145115, 4.985214923628407568 ) ) ;
#7035 = FACE_OUTER_BOUND ( 'NONE', #35435, .T. ) ;
#7036 = CARTESIAN_POINT ( 'NONE',  ( -3.474262827703527901, 13.96481371789853831, 8.843639120294245259 ) ) ;
#7037 = CARTESIAN_POINT ( 'NONE',  ( 13.62178482187499640, 196.1093750006145342, -23.59362340125807123 ) ) ;
#7039 = ORIENTED_EDGE ( 'NONE', *, *, #9923, .F. ) ;
#7038 = ORIENTED_EDGE ( 'NONE', *, *, #12828, .T. ) ;
#7040 = CARTESIAN_POINT ( 'NONE',  ( 26.75643035624999655, 246.3343750006145285, 3.323476615752267715 ) ) ;
#7041 = CARTESIAN_POINT ( 'NONE',  ( -7.228626920338836470, 17.12731371789855217, -10.49813415416005213 ) ) ;
#7042 = CARTESIAN_POINT ( 'NONE',  ( 18.12178482187499640, 4.985214923628404904, -2.015624999385456917 ) ) ;
#7043 = CARTESIAN_POINT ( 'NONE',  ( 13.04141134922778988, 129.8273137178985905, -8.927990412390371944 ) ) ;
#7044 = CARTESIAN_POINT ( 'NONE',  ( 15.24356964374999990, 3.323476615752268604, -0.2906249993854697622 ) ) ;
#7045 = CARTESIAN_POINT ( 'NONE',  ( 22.56230152254410015, 7.347880794884117764E-16, -8.212499998771022547 ) ) ;
#7046 = ORIENTED_EDGE ( 'NONE', *, *, #18000, .T. ) ;
#7047 = CARTESIAN_POINT ( 'NONE',  ( 13.44051670066910731, 5.407089921784862696, -5.221874999385534011 ) ) ;
#7048 = ORIENTED_EDGE ( 'NONE', *, *, #33116, .F. ) ;
#7049 = CARTESIAN_POINT ( 'NONE',  ( -1.926257025242585782E-15, 196.5406250006145399, -31.45816453501075927 ) ) ;
#7050 = CARTESIAN_POINT ( 'NONE',  ( -0.1745138560725500443, 139.2101862821014606, 12.50000000000000355 ) ) ;
#7051 = CARTESIAN_POINT ( 'NONE',  ( 31.01991443737654564, -7.209453229046482114, 164.5281460884161220 ) ) ;
#7052 = CARTESIAN_POINT ( 'NONE',  ( -49.20461230271185116, 207.6069050685336492, -8.469044688360751749 ) ) ;
#7053 = CARTESIAN_POINT ( 'NONE',  ( 15.24356964374999990, 247.0093750006145115, -3.323476615752268604 ) ) ;
#7054 = DIRECTION ( 'NONE',  ( 0.000000000000000000, -0.000000000000000000, 1.000000000000000000 ) ) ;
#7055 = CARTESIAN_POINT ( 'NONE',  ( -43.26711230271184405, 214.4690446883608104, -1.321298161741814914 ) ) ;
#7056 = CARTESIAN_POINT ( 'NONE',  ( 15.00000000000000000, 245.9499999999999886, 0.000000000000000000 ) ) ;
#7057 = CARTESIAN_POINT ( 'NONE',  ( 28.17311034766084887, 5.407089921784856479, 167.8074903081294167 ) ) ;
#7058 = VERTEX_POINT ( 'NONE', #20407 ) ;
#7059 = CARTESIAN_POINT ( 'NONE',  ( 15.06230152254410548, 0.000000000000000000, 10.00000000000000000 ) ) ;
#7060 = CARTESIAN_POINT ( 'NONE',  ( -0.1745138560725817967, 139.2101862821014890, 15.50000000000000533 ) ) ;
#7061 = CARTESIAN_POINT ( 'NONE',  ( -52.18080436395490551, 201.5000000000000000, -0.1155267958017054536 ) ) ;
#7062 = AXIS2_PLACEMENT_3D ( 'NONE', #31879, #19787, #8763 ) ;
#7063 = CARTESIAN_POINT ( 'NONE',  ( -9.465287035748065847, 114.1976862821014578, -2.064181346179273735 ) ) ;
#7064 = DIRECTION ( 'NONE',  ( 0.000000000000000000, 1.000000000000000000, 0.000000000000000000 ) ) ;
#7065 = CARTESIAN_POINT ( 'NONE',  ( 6.932735513423970097, 37.14768628210143930, 10.69584247140445044 ) ) ;
#7066 = ADVANCED_FACE ( 'NONE', ( #29285 ), #476, .T. ) ;
#7067 = CARTESIAN_POINT ( 'NONE',  ( 13.56230152254411614, -5.196152422706638241, -7.575000000000054357 ) ) ;
#7068 = UNCERTAINTY_MEASURE_WITH_UNIT (LENGTH_MEASURE( 1.000000000000000082E-05 ), #1195, 'distance_accuracy_value', 'NONE');
#7069 = EDGE_LOOP ( 'NONE', ( #11306, #3431, #23205, #19972 ) ) ;
#7070 = CARTESIAN_POINT ( 'NONE',  ( 27.00000000000000355, 197.6375000012290286, -3.306546357697854128E-15 ) ) ;
#7071 = CARTESIAN_POINT ( 'NONE',  ( -13.04141134922759804, 114.7726862821014322, -8.927990412390657937 ) ) ;
#7072 = CARTESIAN_POINT ( 'NONE',  ( 15.02283181144952628, 7.347880794884122694E-16, 50.52293445648592751 ) ) ;
#7073 = CARTESIAN_POINT ( 'NONE',  ( 9.465287035748067623, 8.397686282101439303, 2.064181346179272847 ) ) ;
#7074 = CARTESIAN_POINT ( 'NONE',  ( 13.62178482187501416, 199.5031250006145456, 23.59362340125806767 ) ) ;
#7076 = DIRECTION ( 'NONE',  ( 0.08715574274765150453, 0.000000000000000000, 0.9961946980917461003 ) ) ;
#7075 =( BOUNDED_CURVE ( )  B_SPLINE_CURVE ( 2, ( #11841, #3308, #23410, #460, #6152, #34590, #20200 ),
 .UNSPECIFIED., .F., .F. ) 
 B_SPLINE_CURVE_WITH_KNOTS ( ( 3, 2, 2, 3 ),
 ( 0.5217391304347814840, 0.5289855072463758301, 0.5362318840579701762, 0.5434782608695644113 ),
 .UNSPECIFIED. ) 
 CURVE ( )  GEOMETRIC_REPRESENTATION_ITEM ( )  RATIONAL_B_SPLINE_CURVE ( ( 1.000000000000020428, 0.8660254037844181685, 1.000000000000000000, 0.8660254037844387076, 1.000000000000000000, 0.8660254037844530295, 0.9999999999999856781 ) ) 
 REPRESENTATION_ITEM ( '' )  );
#7077 = CARTESIAN_POINT ( 'NONE',  ( -1.909035429704832693E-15, 195.8375000000000057, -31.17691453623979214 ) ) ;
#7078 = CARTESIAN_POINT ( 'NONE',  ( 0.000000000000000000, 143.0000000000000000, 0.000000000000000000 ) ) ;
#7079 = CARTESIAN_POINT ( 'NONE',  ( 24.77555942491173369, 0.000000000000000000, 161.9971211729523475 ) ) ;
#7080 = CARTESIAN_POINT ( 'NONE',  ( -3.796722387233185003, 72.61481371789855643, -8.710071997420207879 ) ) ;
#7081 = EDGE_LOOP ( 'NONE', ( #31814, #20303, #7169, #36106 ) ) ;
#7082 = CARTESIAN_POINT ( 'NONE',  ( 18.00000000000000355, 243.8312500012290513, 5.196152422706632912 ) ) ;
#7083 = CARTESIAN_POINT ( 'NONE',  ( 4.622313124798831829, 82.96481371789856496, -11.61527771782809282 ) ) ;
#7084 = CARTESIAN_POINT ( 'NONE',  ( 16.56230152254411436, 7.209453229046482114, -3.459374999385518290 ) ) ;
#7085 = CARTESIAN_POINT ( 'NONE',  ( -6.422845572874366304, 142.9999999999996305, 10.72508787064079172 ) ) ;
#7086 = CARTESIAN_POINT ( 'NONE',  ( 15.24356964375000167, -3.323476615752272600, -5.165624999385460825 ) ) ;
#7087 = CARTESIAN_POINT ( 'NONE',  ( 2.660918448318002838, 49.90231371789855075, 12.46528703574811558 ) ) ;
#7088 = ORIENTED_EDGE ( 'NONE', *, *, #18149, .T. ) ;
#7089 = CARTESIAN_POINT ( 'NONE',  ( 0.000000000000000000, 210.0000000000000284, 0.000000000000000000 ) ) ;
#7090 = CARTESIAN_POINT ( 'NONE',  ( 18.12178482187500350, 243.9718750006145171, 4.985214923628407568 ) ) ;
#7091 = EDGE_CURVE ( 'NONE', #33961, #5428, #5980, .T. ) ;
#7092 = CARTESIAN_POINT ( 'NONE',  ( -12.50000000000000355, 12.71018628210143753, -0.1745138560725492671 ) ) ;
#7093 = CARTESIAN_POINT ( 'NONE',  ( -44.05877896937849414, 211.6261429550004891, -6.530955311639245586 ) ) ;
#7094 =( BOUNDED_CURVE ( )  B_SPLINE_CURVE ( 2, ( #24018, #35369, #1441, #4103, #878, #15106, #29502, #6573, #9421 ),
 .UNSPECIFIED., .F., .F. ) 
 B_SPLINE_CURVE_WITH_KNOTS ( ( 3, 2, 2, 2, 3 ),
 ( 0.8586956521739130821, 0.8623188405797101996, 0.8695652173913043237, 0.8768115942028985588, 0.8804347826086956763 ),
 .UNSPECIFIED. ) 
 CURVE ( )  GEOMETRIC_REPRESENTATION_ITEM ( )  RATIONAL_B_SPLINE_CURVE ( ( 0.9330127018922194093, 0.9330127018922194093, 1.000000000000000000, 0.8660254037844387076, 1.000000000000000000, 0.8660254037844387076, 1.000000000000000000, 0.9330127018922194093, 0.9330127018922194093 ) ) 
 REPRESENTATION_ITEM ( '' )  );
#7095 = CARTESIAN_POINT ( 'NONE',  ( -52.37127896937850124, 216.5309553116391612, 1.626142955000506873 ) ) ;
#7096 = CARTESIAN_POINT ( 'NONE',  ( 36.64491895294083434, 3.464101615137755275, 159.9799624305654220 ) ) ;
#7097 = CARTESIAN_POINT ( 'NONE',  ( 2.311890736173452865, 91.87731371789855928, -12.53471296425189152 ) ) ;
#7098 = CARTESIAN_POINT ( 'NONE',  ( -41.88913769728823411, 207.8500491399821613, -3.954877714930864485 ) ) ;
#7099 = CARTESIAN_POINT ( 'NONE',  ( -52.97247103062156981, 206.6499508600178672, 5.571401726697986057 ) ) ;
#7100 = CARTESIAN_POINT ( 'NONE',  ( 18.12178482187500350, -4.985214923628407568, -6.028124999385486404 ) ) ;
#7101 = CARTESIAN_POINT ( 'NONE',  ( 24.94224478302373527, 0.000000000000000000, 163.9023435342771506 ) ) ;
#7102 = CARTESIAN_POINT ( 'NONE',  ( 8.927990412390371944, 49.32731371789854791, 13.04141134922778811 ) ) ;
#7103 = CARTESIAN_POINT ( 'NONE',  ( -44.85044563604516554, 203.6929966515019430, -6.137860380172892150 ) ) ;
#7104 = CARTESIAN_POINT ( 'NONE',  ( 3.253724281355069334E-15, 199.8875000000000455, -27.00000000000000000 ) ) ;
#7105 = CARTESIAN_POINT ( 'NONE',  ( 7.228626920339068285, 80.27268628210146062, -10.49813415415989581 ) ) ;
#7106 = CARTESIAN_POINT ( 'NONE',  ( -10.83675517735155047, 23.06018628210144783, -11.08355503943142750 ) ) ;
#7107 = CARTESIAN_POINT ( 'NONE',  ( 16.56230152254411436, -6.928203230275514990, -0.3375000000000368816 ) ) ;
#7108 = ORIENTED_EDGE ( 'NONE', *, *, #9183, .T. ) ;
#7109 = CARTESIAN_POINT ( 'NONE',  ( -15.46528703574804986, 40.59768628210144215, -3.257655550457287497 ) ) ;
#7110 = VECTOR ( 'NONE', #36576, 1000.000000000000000 ) ;
#7111 = CARTESIAN_POINT ( 'NONE',  ( -27.24356964374999279, 197.1406250006145342, 15.72908226750539384 ) ) ;
#7112 = CARTESIAN_POINT ( 'NONE',  ( 2.999999999999997335, 244.5000000000000000, -11.00000000000000000 ) ) ;
#7113 = LINE ( 'NONE', #15451, #35204 ) ;
#7114 = CARTESIAN_POINT ( 'NONE',  ( -37.93080436395489841, 203.5000000000000000, -0.1155267958017335561 ) ) ;
#7115 = CARTESIAN_POINT ( 'NONE',  ( 21.00000000000016342, 4.000000000000002665, 50.00000000000000000 ) ) ;
#7116 = CARTESIAN_POINT ( 'NONE',  ( -2.311890736173176641, 23.92268628210143788, -12.53471296425194836 ) ) ;
#7117 = CARTESIAN_POINT ( 'NONE',  ( 23.87821517812500005, 249.1093750006145342, 4.985214923628404016 ) ) ;
#7118 = CARTESIAN_POINT ( 'NONE',  ( 5.529263428287300108, 132.1273137178985735, 7.954856959092309943 ) ) ;
#7119 = CARTESIAN_POINT ( 'NONE',  ( 15.24356964375000167, 244.9468750006144830, 3.323476615752272600 ) ) ;
#7120 = EDGE_LOOP ( 'NONE', ( #21216, #20886, #8745, #8788 ) ) ;
#7121 = CARTESIAN_POINT ( 'NONE',  ( 20.00041297495057080, 239.8598985277379256, -5.668978411116884608 ) ) ;
#7122 = CARTESIAN_POINT ( 'NONE',  ( 2.311890736173452421, 128.6773137178985564, -12.53471296425189152 ) ) ;
#7123 = CARTESIAN_POINT ( 'NONE',  ( 19.68408634441910721, 5.407089921784857367, -6.590624999385563676 ) ) ;
#7124 = CARTESIAN_POINT ( 'NONE',  ( 27.89856975800574546, 5.407089921784856479, 164.6694770091404223 ) ) ;
#7125 = CARTESIAN_POINT ( 'NONE',  ( -77.00000000000002842, 210.0000000000000000, 0.000000000000000000 ) ) ;
#7126 = CARTESIAN_POINT ( 'NONE',  ( -26.99999999999998934, 197.3375000000000057, 15.58845726811991561 ) ) ;
#7127 = ORIENTED_EDGE ( 'NONE', *, *, #1948, .F. ) ;
#7128 = CARTESIAN_POINT ( 'NONE',  ( 8.715434833791931624, 55.26018628210144357, 8.962234695871760692 ) ) ;
#7129 = ORIENTED_EDGE ( 'NONE', *, *, #7177, .F. ) ;
#7130 = VERTEX_POINT ( 'NONE', #31401 ) ;
#7131 = CARTESIAN_POINT ( 'NONE',  ( -27.00000000000000355, 195.9125000000000796, -15.58845726811989429 ) ) ;
#7132 = CARTESIAN_POINT ( 'NONE',  ( 23.87821517812500005, -4.985214923628404016, -1.340624999385475746 ) ) ;
#7133 = CARTESIAN_POINT ( 'NONE',  ( 20.99999999999999289, 249.2125000000000057, 5.999999999999999112 ) ) ;
#7134 =( BOUNDED_CURVE ( )  B_SPLINE_CURVE ( 2, ( #2379, #13954, #34774, #14876, #32676, #26803, #20389, #14686, #3305 ),
 .UNSPECIFIED., .F., .F. ) 
 B_SPLINE_CURVE_WITH_KNOTS ( ( 3, 2, 2, 2, 3 ),
 ( 0.8804347826086956763, 0.8840579710144927938, 0.8913043478260869179, 0.8985507246376811530, 0.9021739130434782705 ),
 .UNSPECIFIED. ) 
 CURVE ( )  GEOMETRIC_REPRESENTATION_ITEM ( )  RATIONAL_B_SPLINE_CURVE ( ( 0.9330127018922194093, 0.9330127018922194093, 1.000000000000000000, 0.8660254037844387076, 1.000000000000000000, 0.8660254037844387076, 1.000000000000000000, 0.9330127018922194093, 0.9330127018922194093 ) ) 
 REPRESENTATION_ITEM ( '' )  );
#7135 = FACE_OUTER_BOUND ( 'NONE', #14437, .T. ) ;
#7136 = CARTESIAN_POINT ( 'NONE',  ( 15.24356964374999990, 0.000000000000000000, -8.240624999385465443 ) ) ;
#7137 = CARTESIAN_POINT ( 'NONE',  ( -8.715434833791929847, 69.06018628210145494, -8.962234695871762469 ) ) ;
#7138 = CARTESIAN_POINT ( 'NONE',  ( 15.46528703574804986, 137.1976862821014436, 3.257655550457285720 ) ) ;
#7139 = CARTESIAN_POINT ( 'NONE',  ( 10.56230152254410903, 0.000000000000000000, -3.937499998770993770 ) ) ;
#7140 = CARTESIAN_POINT ( 'NONE',  ( -60.88169563604516554, 210.1155267958017703, 4.499999999999996447 ) ) ;
#7141 = CARTESIAN_POINT ( 'NONE',  ( 19.39230484541326760, 245.5924038105676743, 5.999999999999999112 ) ) ;
#7142 = CARTESIAN_POINT ( 'NONE',  ( 31.20375858228842603, -6.928203230275506996, 166.6294942803155550 ) ) ;
#7143 = CARTESIAN_POINT ( 'NONE',  ( -6.932735513424201912, 133.8523137178985678, 10.69584247140429412 ) ) ;
#7144 = CARTESIAN_POINT ( 'NONE',  ( -46.04538769728823411, 211.8571965466039444, -6.469044688360768625 ) ) ;
#7145 = CARTESIAN_POINT ( 'NONE',  ( -57.12872103062156270, 201.4690446883607819, 2.162041339862843525 ) ) ;
#7146 = APPLICATION_PROTOCOL_DEFINITION ( 'draft international standard', 'automotive_design', 1998, #21182 ) ;
#7147 = CARTESIAN_POINT ( 'NONE',  ( 15.24356964374999990, 3.323476615752268604, -0.7406249993854976399 ) ) ;
#7148 = CARTESIAN_POINT ( 'NONE',  ( -13.62178482187500528, 197.4781250006145399, -23.59362340125807123 ) ) ;
#7149 = CIRCLE ( 'NONE', #12598, 4.899999999999999467 ) ;
#7150 = CARTESIAN_POINT ( 'NONE',  ( 13.23911966647199812, 113.1523137178985650, 8.632099005475788900 ) ) ;
#7151 = CARTESIAN_POINT ( 'NONE',  ( -47.81919563604517265, 216.5000000000000000, -0.1155267958017906493 ) ) ;
#7152 = ORIENTED_EDGE ( 'NONE', *, *, #35270, .F. ) ;
#7153 = CARTESIAN_POINT ( 'NONE',  ( 24.74941270219519751, -3.464101615138124757, 161.6982627647491597 ) ) ;
#7154 = CARTESIAN_POINT ( 'NONE',  ( -29.00000000000002487, 210.0000000000000284, 8.000000000000000000 ) ) ;
#7155 = CARTESIAN_POINT ( 'NONE',  ( 34.17230835010118994, -5.407089921784861808, 164.7417095288869859 ) ) ;
#7156 = CARTESIAN_POINT ( 'NONE',  ( 11.08355503943142750, 98.96018628210144641, -10.83675517735155225 ) ) ;
#7157 = CARTESIAN_POINT ( 'NONE',  ( -57.92038769728822700, 208.1428034533959703, 6.469044688360771289 ) ) ;
#7158 = EDGE_CURVE ( 'NONE', #33921, #456, #25893, .T. ) ;
#7159 = CARTESIAN_POINT ( 'NONE',  ( 10.31873187879411091, -3.604726614523240613, -4.153124999385542360 ) ) ;
#7160 = CARTESIAN_POINT ( 'NONE',  ( -0.1745138560725182642, 47.21018628210144641, 9.500000000000005329 ) ) ;
#7161 = CARTESIAN_POINT ( 'NONE',  ( 0.000000000000000000, 200.0000000000000000, 0.000000000000000000 ) ) ;
#7162 = CARTESIAN_POINT ( 'NONE',  ( -39.71205436395491262, 216.1378603801730094, 6.307003348497944195 ) ) ;
#7163 = EDGE_CURVE ( 'NONE', #31911, #22619, #5229, .T. ) ;
#7164 = CARTESIAN_POINT ( 'NONE',  ( 16.56230152254410726, 0.000000000000000000, -10.00000000000000000 ) ) ;
#7165 = CARTESIAN_POINT ( 'NONE',  ( -0.1745138560725500443, 84.01018628210145778, 12.50000000000000355 ) ) ;
#7166 = CARTESIAN_POINT ( 'NONE',  ( 10.56230152254410726, 0.000000000000000000, -8.550000000000029132 ) ) ;
#7167 = CARTESIAN_POINT ( 'NONE',  ( -20.68320042480033294, 194.9291638889422700, -17.35526491262919535 ) ) ;
#7169 = ORIENTED_EDGE ( 'NONE', *, *, #9103, .T. ) ;
#7168 = CARTESIAN_POINT ( 'NONE',  ( 3.796722387233379514, 43.18518628210144072, -8.710071997420127943 ) ) ;
#7170 = ORIENTED_EDGE ( 'NONE', *, *, #30917, .F. ) ;
#7171 = CARTESIAN_POINT ( 'NONE',  ( 15.00000000000000178, -3.464101615137757051, -1.312499999999990230 ) ) ;
#7172 = CARTESIAN_POINT ( 'NONE',  ( -62.07663769728823411, 204.3130714775002730, 3.149950860017883603 ) ) ;
#7173 = CARTESIAN_POINT ( 'NONE',  ( 24.66936984698473623, 3.604726614523240613, 163.5780169909762094 ) ) ;
#7174 = CARTESIAN_POINT ( 'NONE',  ( 30.86058284511243599, 6.928203230275514990, 162.7069776553549616 ) ) ;
#7175 = CARTESIAN_POINT ( 'NONE',  ( 18.00000000000000355, 245.5749999999999886, 5.196152422706632912 ) ) ;
#7176 = CARTESIAN_POINT ( 'NONE',  ( 2.999999999999997335, 252.0000000000000000, -2.499999999999999556 ) ) ;
#7177 = EDGE_CURVE ( 'NONE', #11864, #24223, #14420, .T. ) ;
#7178 = CARTESIAN_POINT ( 'NONE',  ( 8.715434833792128799, 92.73981371789855643, -8.962234695871567070 ) ) ;
#7179 =( REPRESENTATION_RELATIONSHIP ('NONE','NONE', #4304, #29986 ) REPRESENTATION_RELATIONSHIP_WITH_TRANSFORMATION ( #13202 )SHAPE_REPRESENTATION_RELATIONSHIP( ) );
#7180 = CARTESIAN_POINT ( 'NONE',  ( 10.69584247140445221, 99.24768628210145494, -6.932735513423970097 ) ) ;
#7181 = ORIENTED_EDGE ( 'NONE', *, *, #12144, .F. ) ;
#7182 = AXIS2_PLACEMENT_3D ( 'NONE', #15901, #27447, #1478 ) ;
#7183 = ORIENTED_EDGE ( 'NONE', *, *, #2992, .T. ) ;
#7184 = CARTESIAN_POINT ( 'NONE',  ( -13.50000000000000533, 198.6875000012290400, -23.38268590217984411 ) ) ;
#7185 = CARTESIAN_POINT ( 'NONE',  ( 24.97819652690671788, 3.464101615137507473, 164.3132738472399978 ) ) ;
#7186 = CARTESIAN_POINT ( 'NONE',  ( 15.50000000000000533, 75.48981371789854222, -0.1745138560722452326 ) ) ;
#7187 =( BOUNDED_CURVE ( )  B_SPLINE_CURVE ( 2, ( #37111, #11159, #8324, #22732, #10969 ),
 .UNSPECIFIED., .F., .F. ) 
 B_SPLINE_CURVE_WITH_KNOTS ( ( 3, 2, 3 ),
 ( 0.8541666666666667407, 0.8611111111111111605, 0.8636088982343050890 ),
 .UNSPECIFIED. ) 
 CURVE ( )  GEOMETRIC_REPRESENTATION_ITEM ( )  RATIONAL_B_SPLINE_CURVE ( ( 0.9330127018922192983, 0.9330127018922198534, 1.000000000000000000, 0.9759059184691117883, 0.9604780286076208817 ) ) 
 REPRESENTATION_ITEM ( '' )  );
#7188 = CARTESIAN_POINT ( 'NONE',  ( 21.00000000000000000, -6.646953231504538984, -5.990624999385490312 ) ) ;
#7189 = CARTESIAN_POINT ( 'NONE',  ( 15.24356964375000167, 244.4968750006145228, 3.323476615752272600 ) ) ;
#7190 = CARTESIAN_POINT ( 'NONE',  ( -51.38913769728824121, 207.8500491399821613, -3.954877714930864485 ) ) ;
#7191 = CARTESIAN_POINT ( 'NONE',  ( 15.00000000000000000, 0.000000000000000000, -6.693749998770953447 ) ) ;
#7192 = CARTESIAN_POINT ( 'NONE',  ( 8.152565276336593669, 48.75231371789854506, 5.233372021372610483 ) ) ;
#7193 = CARTESIAN_POINT ( 'NONE',  ( 22.80587116629410716, -3.604726614523235284, -6.703124999385561722 ) ) ;
#7194 = VECTOR ( 'NONE', #18538, 1000.000000000000000 ) ;
#7195 = CARTESIAN_POINT ( 'NONE',  ( -5.529263428287297444, 109.1273137178985451, -7.954856959092311719 ) ) ;
#7196 = CARTESIAN_POINT ( 'NONE',  ( 19.00081547855239350, 239.7604221912915534, -5.492723509887032840 ) ) ;
#7197 = CARTESIAN_POINT ( 'NONE',  ( -10.49813415416004858, 33.22731371789855359, 7.228626920338839135 ) ) ;
#7198 = CARTESIAN_POINT ( 'NONE',  ( -2.311890736173176641, 79.12268628210145494, -12.53471296425194836 ) ) ;
#7199 = CARTESIAN_POINT ( 'NONE',  ( 10.56230152254410903, 0.000000000000000000, -8.437499998771025744 ) ) ;
#7200 =( BOUNDED_CURVE ( )  B_SPLINE_CURVE ( 2, ( #27530, #19015, #22596, #22409, #19204 ),
 .UNSPECIFIED., .F., .F. ) 
 B_SPLINE_CURVE_WITH_KNOTS ( ( 3, 2, 3 ),
 ( 0.000000000000000000, 0.007246376811594202987, 0.01086956521739129711 ),
 .UNSPECIFIED. ) 
 CURVE ( )  GEOMETRIC_REPRESENTATION_ITEM ( )  RATIONAL_B_SPLINE_CURVE ( ( 1.000000000000000000, 0.8660254037844387076, 1.000000000000000000, 0.9330127018922194093, 0.9330127018922192983 ) ) 
 REPRESENTATION_ITEM ( '' )  );
#7201 = CARTESIAN_POINT ( 'NONE',  ( 15.24356964374999990, 249.8031250006145285, 0.000000000000000000 ) ) ;
#7202 = CARTESIAN_POINT ( 'NONE',  ( 24.83442103481310781, 0.000000000000000000, 165.4645607004874535 ) ) ;
#7203 = CARTESIAN_POINT ( 'NONE',  ( 16.56230152254411436, 7.209453229046482114, -4.359374999385510208 ) ) ;
#7204 = CARTESIAN_POINT ( 'NONE',  ( 22.56230152254411792, 7.347880794884125653E-16, -1.575000000000048583 ) ) ;
#7205 = CARTESIAN_POINT ( 'NONE',  ( 15.00000000000000000, 0.000000000000000000, -4.950000000000009948 ) ) ;
#7206 = CARTESIAN_POINT ( 'NONE',  ( 3.253724281355069334E-15, 199.5500000012290513, -27.00000000000000000 ) ) ;
#7207 = CARTESIAN_POINT ( 'NONE',  ( -5.529263428287477744, 103.2726862821014322, 7.954856959092191815 ) ) ;
#7208 = CARTESIAN_POINT ( 'NONE',  ( 14.99999999999982414, 3.464101615137652246, -2.231249998770932219 ) ) ;
#7209 = CARTESIAN_POINT ( 'NONE',  ( -8.962234695871760692, 131.1601862821014777, 8.715434833791933400 ) ) ;
#7210 = DIRECTION ( 'NONE',  ( 0.000000000000000000, 0.000000000000000000, -1.000000000000000000 ) ) ;
#7211 = CARTESIAN_POINT ( 'NONE',  ( 15.24356964374999990, 249.4093750006145171, 0.000000000000000000 ) ) ;
#7212 = ORIENTED_EDGE ( 'NONE', *, *, #27619, .T. ) ;
#7213 = CARTESIAN_POINT ( 'NONE',  ( 24.72002912245681472, -3.604726614523240613, 164.1570551592420202 ) ) ;
#7214 = CARTESIAN_POINT ( 'NONE',  ( 21.00000000000000000, 6.646953231504538984, -3.403124999385474858 ) ) ;
#7215 = CARTESIAN_POINT ( 'NONE',  ( 22.56230152254410370, 7.347880794884115792E-16, 10.00000000000000000 ) ) ;
#7216 = CARTESIAN_POINT ( 'NONE',  ( 37.37375885156096444, -3.464101615137755275, 168.3106405921333248 ) ) ;
#7217 = CARTESIAN_POINT ( 'NONE',  ( 18.91622474583366653, 239.6197971919061160, -5.725135026351895640 ) ) ;
#7218 = CARTESIAN_POINT ( 'NONE',  ( 26.75643035624999655, 243.8218750006145399, -3.323476615752271712 ) ) ;
#7219 = CARTESIAN_POINT ( 'NONE',  ( 19.68408634441910721, -5.407089921784855591, -1.790624999385564964 ) ) ;
#7220 = CARTESIAN_POINT ( 'NONE',  ( -3.796722387233185003, 8.214813717898532985, -8.710071997420207879 ) ) ;
#7221 = CARTESIAN_POINT ( 'NONE',  ( 27.24356964374999279, 197.8718750006145513, -15.72908226750539207 ) ) ;
#7223 = EDGE_LOOP ( 'NONE', ( #18130, #12430, #29578, #27605 ) ) ;
#7222 = ORIENTED_EDGE ( 'NONE', *, *, #13634, .F. ) ;
#7224 = CARTESIAN_POINT ( 'NONE',  ( 26.75643035624999655, 246.8593750006145342, -3.323476615752271712 ) ) ;
#7225 = CARTESIAN_POINT ( 'NONE',  ( 8.962234695871567070, 30.63981371789854791, 8.715434833792127023 ) ) ;
#7226 = CARTESIAN_POINT ( 'NONE',  ( 23.87821517812499650, 4.985214923628404904, -0.7406249993854585600 ) ) ;
#7227 = CARTESIAN_POINT ( 'NONE',  ( 15.53471296425188797, 140.1773137178985564, 2.908627838312457747 ) ) ;
#7228 = CARTESIAN_POINT ( 'NONE',  ( 23.99999999999999645, 5.196152422706631135, -9.093749998770938703 ) ) ;
#7229 = ORIENTED_EDGE ( 'NONE', *, *, #25210, .T. ) ;
#7230 = CARTESIAN_POINT ( 'NONE',  ( 22.80587116629412492, -3.604726614523238837, -5.409374999385521576 ) ) ;
#7231 = ORIENTED_EDGE ( 'NONE', *, *, #12828, .F. ) ;
#7232 = CARTESIAN_POINT ( 'NONE',  ( -27.24356964374999635, 196.6906250006145456, 15.72908226750539384 ) ) ;
#7233 = CARTESIAN_POINT ( 'NONE',  ( 12.46528703574805874, 127.9976862821014407, 2.660918448318279950 ) ) ;
#7234 = CARTESIAN_POINT ( 'NONE',  ( 27.77600699476686330, 5.407089921784862696, 163.2685782149489171 ) ) ;
#7235 = CARTESIAN_POINT ( 'NONE',  ( -57.31919563604516554, 218.5000000000000000, -0.1155267958018185298 ) ) ;
#7236 = CARTESIAN_POINT ( 'NONE',  ( 18.12178482187500350, 245.7718750006145001, 4.985214923628407568 ) ) ;
#7237 = CARTESIAN_POINT ( 'NONE',  ( 27.00000000000001421, 196.5875000000000341, 15.58845726811988897 ) ) ;
#7238 = CARTESIAN_POINT ( 'NONE',  ( -50.39211230271182984, 205.5309553116392465, 1.321298161741817356 ) ) ;
#7239 = LINE ( 'NONE', #13107, #26015 ) ;
#7240 = CARTESIAN_POINT ( 'NONE',  ( 16.56230152254411436, -6.928203230275506996, -2.024999998770999454 ) ) ;
#7241 = ORIENTED_EDGE ( 'NONE', *, *, #10058, .T. ) ;
#7242 = CARTESIAN_POINT ( 'NONE',  ( 24.00000000000000000, -5.196152422706629359, -5.250000000000004441 ) ) ;
#7243 = CARTESIAN_POINT ( 'NONE',  ( -11.08355503943142573, 121.9601862821014606, 10.83675517735155402 ) ) ;
#7244 = CARTESIAN_POINT ( 'NONE',  ( -48.02455436395490551, 203.6929966515020283, 6.137860380172978303 ) ) ;
#7245 = CARTESIAN_POINT ( 'NONE',  ( 9.534712964251941258, 118.2226862821014493, -1.715153634034235708 ) ) ;
#7246 = CARTESIAN_POINT ( 'NONE',  ( 0.000000000000000000, 202.0000000000000000, -27.00000000000000000 ) ) ;
#7247 = CARTESIAN_POINT ( 'NONE',  ( 8.962234695871762469, 6.960186282101432198, -8.715434833791931624 ) ) ;
#7248 = CARTESIAN_POINT ( 'NONE',  ( 13.44051670066910908, -5.407089921784859143, -0.5156249993855110958 ) ) ;
#7249 = ORIENTED_EDGE ( 'NONE', *, *, #24892, .T. ) ;
#7250 = CARTESIAN_POINT ( 'NONE',  ( -32.78497103062156981, 204.4285982733020148, -3.350049139982115509 ) ) ;
#7251 = CARTESIAN_POINT ( 'NONE',  ( 9.534712964251941258, 72.22268628210143504, -1.715153634034235708 ) ) ;
#7252 = LINE ( 'NONE', #32828, #16365 ) ;
#7253 = CARTESIAN_POINT ( 'NONE',  ( 8.843639120294245259, 131.2648137178985621, 3.474262827703527901 ) ) ;
#7254 = CARTESIAN_POINT ( 'NONE',  ( -27.24356964374999990, 197.9656250006145228, -15.72908226750537786 ) ) ;
#7255 = DIRECTION ( 'NONE',  ( 1.000000000000000000, 0.000000000000000000, 0.000000000000000000 ) ) ;
#7256 = CARTESIAN_POINT ( 'NONE',  ( 5.778771075727756162E-15, 198.1718750006145342, 31.45816453501075927 ) ) ;
#7257 = CARTESIAN_POINT ( 'NONE',  ( 22.60184008074515916, 0.09462734519745615025, -10.00000000000000178 ) ) ;
#7258 = CYLINDRICAL_SURFACE ( 'NONE', #12111, 5.999999999999994671 ) ;
#7259 = CARTESIAN_POINT ( 'NONE',  ( -9.500000000000005329, 80.08981371789856496, 0.1745138560723101806 ) ) ;
#7260 = ORIENTED_EDGE ( 'NONE', *, *, #13066, .T. ) ;
#7261 = CARTESIAN_POINT ( 'NONE',  ( 24.00000000000000000, 244.3562500012290286, 5.196152422706629359 ) ) ;
#7262 = CARTESIAN_POINT ( 'NONE',  ( -11.48171059495408208, 79.51481371789856212, 4.944772684328421875 ) ) ;
#7263 = CARTESIAN_POINT ( 'NONE',  ( 16.56230152254411436, -7.209453229046482114, -5.034374999385487826 ) ) ;
#7264 = CARTESIAN_POINT ( 'NONE',  ( -31.00000000000003553, 209.9999999999999716, -6.500000000000000888 ) ) ;
#7265 = CARTESIAN_POINT ( 'NONE',  ( 26.75643035624999655, 3.323476615752271712, -4.940624999385510918 ) ) ;
#7266 = CARTESIAN_POINT ( 'NONE',  ( -2.660918448318004614, 45.30231371789855643, -12.46528703574811558 ) ) ;
#7267 = EDGE_LOOP ( 'NONE', ( #10105, #34010 ) ) ;
#7268 = CARTESIAN_POINT ( 'NONE',  ( 15.24356964374999990, 3.323476615752268604, -6.928124999385478766 ) ) ;
#7269 = CARTESIAN_POINT ( 'NONE',  ( 26.75643035624999655, 245.0218750006145001, -7.049594010296217766E-16 ) ) ;
#7270 = CARTESIAN_POINT ( 'NONE',  ( -11.48171059495397373, 22.48518628210144499, -4.944772684328680334 ) ) ;
#7271 = EDGE_CURVE ( 'NONE', #24534, #25338, #34015, .T. ) ;
#7272 = CARTESIAN_POINT ( 'NONE',  ( -34.95461230271183695, 208.1428034533958851, -6.469044688360754414 ) ) ;
#7273 = VECTOR ( 'NONE', #30741, 1000.000000000000000 ) ;
#7274 = CARTESIAN_POINT ( 'NONE',  ( -57.31919563604516554, 216.5000000000000000, -0.1155267958017906493 ) ) ;
#7275 = CARTESIAN_POINT ( 'NONE',  ( 27.58438479987706415, -5.196152422706632912, 159.6810023811194981 ) ) ;
#7276 = CARTESIAN_POINT ( 'NONE',  ( -8.962234695871565293, 62.83981371789855785, -8.715434833792128799 ) ) ;
#7277 = CARTESIAN_POINT ( 'NONE',  ( -51.19122103062157692, 208.9097554298617752, -4.530955311639240257 ) ) ;
#7278 = CARTESIAN_POINT ( 'NONE',  ( -58.90997103062156270, 215.5714017266979852, 3.350049139982118618 ) ) ;
#7279 = DIRECTION ( 'NONE',  ( 1.000000000000000000, 0.000000000000000000, 0.000000000000000000 ) ) ;
#7280 = CARTESIAN_POINT ( 'NONE',  ( -11.18923628784230573, 217.4947066899765389, -4.100298858792801759 ) ) ;
#7281 = CARTESIAN_POINT ( 'NONE',  ( -10.83675517735179028, 60.53981371789856070, 11.08355503943118947 ) ) ;
#7282 = CARTESIAN_POINT ( 'NONE',  ( -51.38169563604516554, 210.1155267958018271, 8.500000000000003553 ) ) ;
#7283 = CYLINDRICAL_SURFACE ( 'NONE', #25014, 5.999999999999999112 ) ;
#7284 = CARTESIAN_POINT ( 'NONE',  ( -6.932735513423968321, 69.34768628210143504, -10.69584247140445221 ) ) ;
#7285 = CARTESIAN_POINT ( 'NONE',  ( -15.53471296425195369, 30.82268628210143291, 2.908627838312118019 ) ) ;
#7286 = EDGE_CURVE ( 'NONE', #33968, #5728, #34834, .T. ) ;
#7287 = CARTESIAN_POINT ( 'NONE',  ( 16.56230152254412147, 6.928203230275514990, -0.5625000000000506262 ) ) ;
#7288 = CARTESIAN_POINT ( 'NONE',  ( -13.50000000000000533, 197.3375000012290457, -23.38268590217984411 ) ) ;
#7289 = ORIENTED_EDGE ( 'NONE', *, *, #4005, .F. ) ;
#7290 = CARTESIAN_POINT ( 'NONE',  ( -13.04141134922759804, 31.97268628210143149, -8.927990412390657937 ) ) ;
#7291 = CARTESIAN_POINT ( 'NONE',  ( -13.62178482187500528, 198.3781250006145171, -23.59362340125807123 ) ) ;
#7292 = DIRECTION ( 'NONE',  ( -1.659705900203722642E-32, 2.710505431213758127E-16, 1.000000000000000000 ) ) ;
#7293 = CARTESIAN_POINT ( 'NONE',  ( 26.99999999999999645, 247.5250000000000057, -7.347880794884117764E-16 ) ) ;
#7294 = CARTESIAN_POINT ( 'NONE',  ( -36.34747103062156981, 213.3500491399821328, -5.571401726697985168 ) ) ;
#7295 = ADVANCED_FACE ( 'NONE', ( #33077, #24176 ), #35341, .T. ) ;
#7296 = CARTESIAN_POINT ( 'NONE',  ( -2.660918448318275509, 29.09768628210144925, 12.46528703574805874 ) ) ;
#7297 = DIRECTION ( 'NONE',  ( 0.000000000000000000, 1.000000000000000000, 0.000000000000000000 ) ) ;
#7298 = CARTESIAN_POINT ( 'NONE',  ( 6.594114490232462877, 138.7398137178985564, -6.840914352311949109 ) ) ;
#7299 = CARTESIAN_POINT ( 'NONE',  ( 26.75643035624999655, 243.8218750006145399, -3.323476615752271268 ) ) ;
#7300 = AXIS2_PLACEMENT_3D ( 'NONE', #14421, #31662, #32033 ) ;
#7301 = VERTEX_POINT ( 'NONE', #7121 ) ;
#7302 = FILL_AREA_STYLE_COLOUR ( '', #15397 ) ;
#7303 = CARTESIAN_POINT ( 'NONE',  ( -54.50000000000000711, 244.5000000000000000, -2.499999999999996003 ) ) ;
#7304 = CARTESIAN_POINT ( 'NONE',  ( -4.622313124798826500, 142.7648137178985621, 11.61527771782809637 ) ) ;
#7305 = CARTESIAN_POINT ( 'NONE',  ( 22.80587116629410716, 3.604726614523238837, -7.978124999385491023 ) ) ;
#7306 = CARTESIAN_POINT ( 'NONE',  ( 37.13677269252619340, 7.646167579472015790E-16, 162.8072281515975135 ) ) ;
#7307 = CARTESIAN_POINT ( 'NONE',  ( 18.00000000000000000, 5.196152422706630247, -1.874999999999987788 ) ) ;
#7308 = CARTESIAN_POINT ( 'NONE',  ( -26.99999999999998934, 196.8875000000000171, 15.58845726811991561 ) ) ;
#7309 = ORIENTED_EDGE ( 'NONE', *, *, #21463, .F. ) ;
#7310 = CARTESIAN_POINT ( 'NONE',  ( 4.622313124798573369, 37.43518628210144783, 11.61527771782819940 ) ) ;
#7311 = ORIENTED_EDGE ( 'NONE', *, *, #36224, .T. ) ;
#7312 = ORIENTED_EDGE ( 'NONE', *, *, #30081, .T. ) ;
#7313 = CARTESIAN_POINT ( 'NONE',  ( 36.64165061258780298, 7.347880794884117764E-16, 159.9426051293869477 ) ) ;
#7314 = DIRECTION ( 'NONE',  ( 1.000000000000000000, 0.000000000000000000, -0.000000000000000000 ) ) ;
#7315 = DIRECTION ( 'NONE',  ( 1.000000000000000000, 0.000000000000000000, 1.636531581110199847E-16 ) ) ;
#7316 = CARTESIAN_POINT ( 'NONE',  ( -7.234628195640354420, 196.4924038105676800, 26.99999999999996803 ) ) ;
#7317 = CARTESIAN_POINT ( 'NONE',  ( 26.75643035624999655, 7.049594010296217766E-16, -8.465624999385468641 ) ) ;
#7318 = CARTESIAN_POINT ( 'NONE',  ( 4.622313124798573369, 83.43518628210145494, 11.61527771782819940 ) ) ;
#7319 = CARTESIAN_POINT ( 'NONE',  ( -8.632099005475501130, 133.7476862821013981, -13.23911966647218996 ) ) ;
#7320 = DIRECTION ( 'NONE',  ( -2.057406622567553763E-16, 0.000000000000000000, 1.000000000000000000 ) ) ;
#7321 = CARTESIAN_POINT ( 'NONE',  ( 13.90958069845249767, 212.6589072380734251, 5.392997762652351312 ) ) ;
#7322 = CARTESIAN_POINT ( 'NONE',  ( -48.61086230271182984, 212.1499508600178387, -3.954877714930852495 ) ) ;
#7323 = CARTESIAN_POINT ( 'NONE',  ( 10.56230152254411081, 0.000000000000000000, -2.137499998771025034 ) ) ;
#7324 = CARTESIAN_POINT ( 'NONE',  ( 25.22005371303187715, -3.464101615137757051, 167.0777141344445624 ) ) ;
#7325 = CARTESIAN_POINT ( 'NONE',  ( 7.954856959092311719, 10.22731371789853405, -5.529263428287300108 ) ) ;
#7326 = ADVANCED_FACE ( 'NONE', ( #18692 ), #12422, .F. ) ;
#7327 = CARTESIAN_POINT ( 'NONE',  ( -40.70163769728823411, 215.6869285224996986, -3.149950860017881382 ) ) ;
#7328 = CARTESIAN_POINT ( 'NONE',  ( -52.57663769728824832, 202.5810206699313767, 4.149950860017909804 ) ) ;
#7329 = ITEM_DEFINED_TRANSFORMATION ( 'NONE', 'NONE', #2663,  #17215 ) ;
#7330 = VECTOR ( 'NONE', #3813, 1000.000000000000000 ) ;
#7331 = CARTESIAN_POINT ( 'NONE',  ( 15.24356964374999990, 3.323476615752268604, -2.540624999385480809 ) ) ;
#7332 = CARTESIAN_POINT ( 'NONE',  ( 13.62178482187499640, 199.6531250006145228, -23.59362340125807123 ) ) ;
#7333 = CARTESIAN_POINT ( 'NONE',  ( -5.770363421894122880, 115.1648137178985678, 14.38691631536194393 ) ) ;
#7334 = CARTESIAN_POINT ( 'NONE',  ( -48.80877896937850835, 211.6261429550004607, -6.530955311639245586 ) ) ;
#7335 = ADVANCED_FACE ( 'NONE', ( #35537, #20971 ), #852, .T. ) ;
#7336 = ORIENTED_EDGE ( 'NONE', *, *, #1487, .F. ) ;
#7337 = CARTESIAN_POINT ( 'NONE',  ( -49.64999999999999858, 244.5000000000000000, 5.000000000000000000 ) ) ;
#7338 = CARTESIAN_POINT ( 'NONE',  ( 4.944772684328679446, 135.1851862821014549, -11.48171059495397373 ) ) ;
#7339 = DIRECTION ( 'NONE',  ( 1.000000000000000000, 0.000000000000000000, 0.000000000000000000 ) ) ;
#7340 = CARTESIAN_POINT ( 'NONE',  ( 37.33123894353190764, 3.604726614523243278, 165.0299875717147415 ) ) ;
#7341 = CARTESIAN_POINT ( 'NONE',  ( -15.50000000000000533, 95.51018628210147199, -0.1745138560725808530 ) ) ;
#7342 = CARTESIAN_POINT ( 'NONE',  ( -55.74330436395489841, 210.1155267958017134, -6.500000000000000888 ) ) ;
#7343 = EDGE_CURVE ( 'NONE', #23173, #8675, #12991, .T. ) ;
#7344 = CARTESIAN_POINT ( 'NONE',  ( 22.80587116629410716, 7.646167579472015790E-16, -3.065624999385535787 ) ) ;
#7345 = CARTESIAN_POINT ( 'NONE',  ( 5.233372021372432847, 37.14768628210143220, 8.152565276336710909 ) ) ;
#7346 = CARTESIAN_POINT ( 'NONE',  ( 21.00000000000000355, 0.000000000000000000, 50.00000000000001421 ) ) ;
#7347 = CARTESIAN_POINT ( 'NONE',  ( -40.30580436395490551, 218.5000000000000000, 0.1155267958017064944 ) ) ;
#7348 = CARTESIAN_POINT ( 'NONE',  ( 22.80587116629411071, 3.604726614523243278, -9.384374999385521221 ) ) ;
#7349 = CARTESIAN_POINT ( 'NONE',  ( -10.49813415415989581, 68.77268628210146062, -7.228626920339068285 ) ) ;
#7350 = PLANE ( 'NONE',  #2724 ) ;
#7351 = FACE_OUTER_BOUND ( 'NONE', #26023, .T. ) ;
#7353 = CARTESIAN_POINT ( 'NONE',  ( 10.31873187879410736, 0.000000000000000000, -0.6468749993855105185 ) ) ;
#7352 = CARTESIAN_POINT ( 'NONE',  ( -2.064181346179269738, 38.29768628210144499, 9.465287035748067623 ) ) ;
#7354 = CYLINDRICAL_SURFACE ( 'NONE', #21587, 2.649999999999991029 ) ;
#7355 = VERTEX_POINT ( 'NONE', #29850 ) ;
#7356 = CARTESIAN_POINT ( 'NONE',  ( 26.99999999999999645, -3.464101615137751278, -2.062499999999993339 ) ) ;
#7357 = CARTESIAN_POINT ( 'NONE',  ( 30.78459393195788607, -7.209453229046482114, 161.8384204035683922 ) ) ;
#7358 = CARTESIAN_POINT ( 'NONE',  ( 33.71516498491316582, -5.196152422706635576, 160.9138610787959465 ) ) ;
#7359 = CARTESIAN_POINT ( 'NONE',  ( 21.00000000000000000, 246.2874999999999659, -6.928203230275506996 ) ) ;
#7360 = CARTESIAN_POINT ( 'NONE',  ( 10.56230152254410903, 0.000000000000000000, -3.937499998770993770 ) ) ;
#7361 = CARTESIAN_POINT ( 'NONE',  ( 8.962234695871567070, 76.63981371789856212, 8.715434833792127023 ) ) ;
#7362 = CARTESIAN_POINT ( 'NONE',  ( 10.69584247140445221, 90.04768628210145209, -6.932735513423970097 ) ) ;
#7363 = VERTEX_POINT ( 'NONE', #32503 ) ;
#7364 = VECTOR ( 'NONE', #35617, 1000.000000000000000 ) ;
#7365 = ORIENTED_EDGE ( 'NONE', *, *, #4969, .F. ) ;
#7366 = CARTESIAN_POINT ( 'NONE',  ( -26.99999999999998934, 198.8000000012290513, 15.58845726811991561 ) ) ;
#7367 = CARTESIAN_POINT ( 'NONE',  ( 20.99999999999999289, 248.5937500012290400, -5.999999999999997335 ) ) ;
#7368 = CARTESIAN_POINT ( 'NONE',  ( -3.257655550456946880, 54.50231371789855928, -15.46528703574811736 ) ) ;
#7369 = CARTESIAN_POINT ( 'NONE',  ( 18.12178482187500350, -4.985214923628407568, -7.378124999385477167 ) ) ;
#7370 = CARTESIAN_POINT ( 'NONE',  ( 18.12178482187499640, 244.8343750006145285, -4.985214923628404904 ) ) ;
#7371 = CARTESIAN_POINT ( 'NONE',  ( -59.50372103062157692, 214.5309553116392749, -1.090244570138262148 ) ) ;
#7372 = DIRECTION ( 'NONE',  ( 0.000000000000000000, 0.000000000000000000, -1.000000000000000000 ) ) ;
#7373 = EDGE_CURVE ( 'NONE', #32537, #212, #6292, .T. ) ;
#7374 = CARTESIAN_POINT ( 'NONE',  ( -9.500000000000005329, 61.68981371789855928, 0.1745138560723101806 ) ) ;
#7375 = CARTESIAN_POINT ( 'NONE',  ( 19.68408634441910721, 5.407089921784857367, -7.940624999385553551 ) ) ;
#7376 = CARTESIAN_POINT ( 'NONE',  ( 1.715153634034445762, 110.2773137178985650, -9.534712964251895073 ) ) ;
#7377 = CARTESIAN_POINT ( 'NONE',  ( 26.75643035624999655, 240.5218750006145001, -7.049594010296217766E-16 ) ) ;
#7378 = CARTESIAN_POINT ( 'NONE',  ( -2.660918448318004614, 26.90231371789854364, -12.46528703574811558 ) ) ;
#7379 = AXIS2_PLACEMENT_3D ( 'NONE', #24131, #4910, #801 ) ;
#7380 = CARTESIAN_POINT ( 'NONE',  ( -4.944772684328673229, 84.58518628210146062, 11.48171059495397728 ) ) ;
#7381 = CARTESIAN_POINT ( 'NONE',  ( 10.56230152254411081, 0.000000000000000000, -7.537499998771012955 ) ) ;
#7382 = CARTESIAN_POINT ( 'NONE',  ( 33.94189035521207387, -5.407089921784855591, 162.1080197958069107 ) ) ;
#7383 = CARTESIAN_POINT ( 'NONE',  ( 19.68408634441911431, 5.407089921784862696, -5.296874999385526195 ) ) ;
#7384 = CARTESIAN_POINT ( 'NONE',  ( 13.56230152254411614, -5.196152422706638241, -1.725000000000059819 ) ) ;
#7385 = DIRECTION ( 'NONE',  ( -0.000000000000000000, -0.000000000000000000, -1.000000000000000000 ) ) ;
#7386 = CARTESIAN_POINT ( 'NONE',  ( 7.954856959092191815, 91.77268628210144641, 5.529263428287477744 ) ) ;
#7387 = FACE_OUTER_BOUND ( 'NONE', #17940, .T. ) ;
#7388 = CARTESIAN_POINT ( 'NONE',  ( 8.962234695871762469, 126.5601862821014691, -8.715434833791931624 ) ) ;
#7389 = CARTESIAN_POINT ( 'NONE',  ( 10.56230152254410726, 0.000000000000000000, -3.150000000000041656 ) ) ;
#7390 = CARTESIAN_POINT ( 'NONE',  ( 15.24356964375000167, 240.3343750006145001, 3.323476615752272600 ) ) ;
#7391 = EDGE_LOOP ( 'NONE', ( #33138, #6647, #18909, #8193 ) ) ;
#7392 = CARTESIAN_POINT ( 'NONE',  ( 24.79846929092969887, -3.604726614523240613, 165.0536303875245778 ) ) ;
#7393 = CARTESIAN_POINT ( 'NONE',  ( 26.75643035624999655, -3.323476615752267715, -5.353124999385477700 ) ) ;
#7394 = CARTESIAN_POINT ( 'NONE',  ( -13.62178482187500528, 197.5343750006145456, -23.59362340125807123 ) ) ;
#7395 =( BOUNDED_CURVE ( )  B_SPLINE_CURVE ( 2, ( #8153, #33547, #19727, #2261, #16310, #4916, #11171, #22555, #18972, #30527, #19535, #27856, #1889, #16497, #13652, #31265, #4549, #5291, #2447, #10798, #33919, #7962, #16686, #28232, #13840, #28408, #25387, #36937, #10983, #14022, #25571, #37124, #12095, #31448, #35031, #23669, #14765, #19907, #28592, #32192, #28966, #5849, #6226, #3006, #34655, #11359, #8337, #11540, #23112, #5659, #9076, #14389, #8518, #528, #5471, #17427, #8700, #14206, #2818, #14575, #29148, #26127, #32002, #20274, #37489, #17054, #2629, #20085, #31813, #25757, #159, #37309, #31629, #11726, #22930, #23298, #34845, #25946, #34475, #17800, #8883, #17239, #28780, #20461, #6032, #17618, #3189, #26310, #347, #20645, #11912, #23478, #29342, #3381, #14949, #26497, #29533, #27073, #3574, #18564, #18365, #35592, #9637, #29719, #21400, #15134, #13048, #30293, #29913, #26686, #4136, #3943, #35779, #23861, #35970, #24422, #35400, #24047, #716, #30105, #21214, #12666, #3753, #15708, #35214, #9822, #27259, #15897, #10007, #1282, #21027, #910, #32753, #21589, #32562, #9263, #6790, #4318, #24234, #33136, #32940, #15519, #1098, #12479, #6604, #1474, #6994, #7180, #9450, #12854, #18751, #18179, #20835, #27443, #32378, #12289, #6417, #17990, #15327, #26879, #28369, #19682, #19496, #22515, #13613, #24787, #16827, #2405, #21959, #34062, #27820, #24966, #1849, #10383, #18934, #8110, #4878, #4689, #30673, #7362, #13237, #10756, #19315, #16271, #33504, #33880, #10568, #19122, #36525, #2217, #7549, #31221, #22145, #33693, #7732, #30487, #36716, #5251, #13418, #31043, #24604, #30853, #16458, #2034, #36153, #25161, #22328, #10197, #5064, #7922, #16645, #28187, #28002, #13799, #21773, #25348, #36894, #10942, #33323, #4508, #16084, #27634, #1663, #36337, #34249, #2958, #29102, #6178, #3145, #5427, #14714, #34797, #17008, #17195, #17750, #17567, #29292, #13978, #14527, #14161, #37268, #37447, #8654, #28734, #22882, #25529, #26083, #23431, #25715, #17382, #2773, #11314, #37082, #26263, #23252, #19864, #34612, #112, #31407, #20413, #11129, #9026, #8841, #11862, #11678, #34433, #22707, #20224, #25899, #11496, #8292, #31956, #28548, #34983, #5988, #8470, #297, #20598, #32138, #2590, #20042, #31586, #5610, #23065, #14346, #5800, #31768, #28923, #3520, #32701, #24182, #9958, #29859, #12801, #35727, #27020, #32890, #9773, #859, #12429, #7128, #15086, #29671, #20784, #21350, #15275, #32510, #6942, #6555, #9213, #23620, #3895, #18511, #33085, #30050, #32328, #4084, #15656, #6367, #18129, #18700, #3705, #35915, #15466, #27206, #1045, #26828, #23998, #35544, #9588, #12237, #3330, #12617, #24371, #26636, #6742, #21162, #666, #14901, #1230, #21539, #17938, #18317, #35165, #26450, #482, #29482, #12049, #23808, #35350, #9402, #20977, #30993, #4639, #21904, #7494, #12998, #7682, #15842, #22279, #24920, #1611, #7310, #19443, #5012, #19070, #36286, #24554, #27582, #30622, #19262, #1798, #36104, #36473, #18883, #27768, #30801, #7869, #30241, #4453, #33832, #27390, #30434, #10514, #10147, #33453, #16218, #13181, #1420, #10702, #10333, #16033, #33643, #13365, #22093, #24735, #4824, #16405, #27951, #1982, #13553, #4268, #25107, #36664, #21720, #33271, #5494, #36965, #25596, #34679, #32022, #2653, #14229, #34316, #25967, #19752, #14412, #28615, #25780, #34498, #17076, #14600, #23318, #8540, #16894, #37151, #22582, #6053, #14046, #184, #37330, #22953, #28433, #11380, #34127, #5690, #20106, #5318, #34867, #8724, #11750, #2473, #17640, #31654, #5681, #17263, #8177, #23137, #11009, #8909, #28803, #11192, #26151, #20484, #2288, #22767, #13864, #2840, #31470, #31290, #19932, #11564, #8361, #20296, #31838, #5871, #17449, #25412, #28987, #3028, #1122, #32401, #29558, #6441, #14974, #23505, #27098, #9475, #9288, #35238, #11934 ),
 .UNSPECIFIED., .F., .F. ) 
 B_SPLINE_CURVE_WITH_KNOTS ( ( 3, 2, 2, 2, 2, 2, 2, 2, 2, 2, 2, 2, 2, 2, 2, 2, 2, 2, 2, 2, 2, 2, 2, 2, 2, 2, 2, 2, 2, 2, 2, 2, 2, 2, 2, 2, 2, 2, 2, 2, 2, 2, 2, 2, 2, 2, 2, 2, 2, 2, 2, 2, 2, 2, 2, 2, 2, 2, 2, 2, 2, 2, 2, 2, 2, 2, 2, 2, 2, 2, 2, 2, 2, 2, 2, 2, 2, 2, 2, 2, 2, 2, 2, 2, 2, 2, 2, 2, 2, 2, 2, 2, 2, 2, 2, 2, 2, 2, 2, 2, 2, 2, 2, 2, 2, 2, 2, 2, 2, 2, 2, 2, 2, 2, 2, 2, 2, 2, 2, 2, 2, 2, 2, 2, 2, 2, 2, 2, 2, 2, 2, 2, 2, 2, 2, 2, 2, 2, 2, 2, 2, 2, 2, 2, 2, 2, 2, 2, 2, 2, 2, 2, 2, 2, 2, 2, 2, 2, 2, 2, 2, 2, 2, 2, 2, 2, 2, 2, 2, 2, 2, 2, 2, 2, 2, 2, 2, 2, 2, 2, 2, 2, 2, 2, 2, 2, 2, 2, 2, 2, 2, 2, 2, 2, 2, 2, 2, 2, 2, 2, 2, 2, 2, 2, 2, 2, 2, 2, 2, 2, 2, 2, 2, 2, 2, 2, 2, 2, 2, 2, 2, 2, 2, 2, 2, 2, 2, 2, 2, 2, 2, 2, 2, 2, 2, 2, 2, 2, 2, 2, 3 ),
 ( 0.000000000000000000, 0.004166666666666666609, 0.008333333333333333218, 0.01250000000000000069, 0.01666666666666666644, 0.02083333333333333218, 0.02500000000000000139, 0.02916666666666666713, 0.03333333333333333287, 0.03749999999999999861, 0.04166666666666666435, 0.04583333333333333010, 0.05000000000000000278, 0.05416666666666666852, 0.05833333333333333426, 0.06250000000000000000, 0.06666666666666666574, 0.07083333333333333148, 0.07499999999999999722, 0.07916666666666666297, 0.08333333333333332871, 0.08749999999999999445, 0.09166666666666666019, 0.09583333333333333981, 0.1000000000000000056, 0.1041666666666666713, 0.1083333333333333370, 0.1125000000000000028, 0.1166666666666666685, 0.1208333333333333343, 0.1250000000000000000, 0.1291666666666666796, 0.1333333333333333315, 0.1375000000000000111, 0.1416666666666666630, 0.1458333333333333426, 0.1499999999999999944, 0.1541666666666666741, 0.1583333333333333259, 0.1625000000000000056, 0.1666666666666666574, 0.1708333333333333370, 0.1749999999999999889, 0.1791666666666666685, 0.1833333333333333204, 0.1875000000000000000, 0.1916666666666666796, 0.1958333333333333315, 0.2000000000000000111, 0.2041666666666666630, 0.2083333333333333426, 0.2124999999999999944, 0.2166666666666666741, 0.2208333333333333259, 0.2250000000000000056, 0.2291666666666666574, 0.2333333333333333370, 0.2374999999999999889, 0.2416666666666666685, 0.2458333333333333204, 0.2500000000000000000, 0.2541666666666666519, 0.2583333333333333592, 0.2625000000000000111, 0.2666666666666666630, 0.2708333333333333148, 0.2750000000000000222, 0.2791666666666666741, 0.2833333333333333259, 0.2874999999999999778, 0.2916666666666666852, 0.2958333333333333370, 0.2999999999999999889, 0.3041666666666666408, 0.3083333333333333481, 0.3125000000000000000, 0.3166666666666666519, 0.3208333333333333592, 0.3250000000000000111, 0.3291666666666666630, 0.3333333333333333148, 0.3375000000000000222, 0.3416666666666666741, 0.3458333333333333259, 0.3499999999999999778, 0.3541666666666666852, 0.3583333333333333370, 0.3624999999999999889, 0.3666666666666666408, 0.3708333333333333481, 0.3750000000000000000, 0.3791666666666666519, 0.3833333333333333592, 0.3875000000000000111, 0.3916666666666666630, 0.3958333333333333148, 0.4000000000000000222, 0.4041666666666666741, 0.4083333333333333259, 0.4124999999999999778, 0.4166666666666666852, 0.4208333333333333370, 0.4249999999999999889, 0.4291666666666666408, 0.4333333333333333481, 0.4375000000000000000, 0.4416666666666666519, 0.4458333333333333592, 0.4500000000000000111, 0.4541666666666666630, 0.4583333333333333148, 0.4625000000000000222, 0.4666666666666666741, 0.4708333333333333259, 0.4749999999999999778, 0.4791666666666666852, 0.4833333333333333370, 0.4874999999999999889, 0.4916666666666666408, 0.4958333333333333481, 0.5000000000000000000, 0.5041666666666666519, 0.5083333333333333037, 0.5124999999999999556, 0.5166666666666667185, 0.5208333333333333703, 0.5250000000000000222, 0.5291666666666666741, 0.5333333333333333259, 0.5374999999999999778, 0.5416666666666666297, 0.5458333333333332815, 0.5500000000000000444, 0.5541666666666666963, 0.5583333333333333481, 0.5625000000000000000, 0.5666666666666666519, 0.5708333333333333037, 0.5749999999999999556, 0.5791666666666667185, 0.5833333333333333703, 0.5875000000000000222, 0.5916666666666666741, 0.5958333333333333259, 0.5999999999999999778, 0.6041666666666666297, 0.6083333333333332815, 0.6125000000000000444, 0.6166666666666666963, 0.6208333333333333481, 0.6250000000000000000, 0.6291666666666666519, 0.6333333333333333037, 0.6374999999999999556, 0.6416666666666667185, 0.6458333333333333703, 0.6500000000000000222, 0.6541666666666666741, 0.6583333333333333259, 0.6624999999999999778, 0.6666666666666666297, 0.6708333333333332815, 0.6750000000000000444, 0.6791666666666666963, 0.6833333333333333481, 0.6875000000000000000, 0.6916666666666666519, 0.6958333333333333037, 0.6999999999999999556, 0.7041666666666667185, 0.7083333333333333703, 0.7125000000000000222, 0.7166666666666666741, 0.7208333333333333259, 0.7249999999999999778, 0.7291666666666666297, 0.7333333333333332815, 0.7375000000000000444, 0.7416666666666666963, 0.7458333333333333481, 0.7500000000000000000, 0.7541666666666666519, 0.7583333333333333037, 0.7624999999999999556, 0.7666666666666667185, 0.7708333333333333703, 0.7750000000000000222, 0.7791666666666666741, 0.7833333333333333259, 0.7874999999999999778, 0.7916666666666666297, 0.7958333333333332815, 0.8000000000000000444, 0.8041666666666666963, 0.8083333333333333481, 0.8125000000000000000, 0.8166666666666666519, 0.8208333333333333037, 0.8249999999999999556, 0.8291666666666667185, 0.8333333333333333703, 0.8375000000000000222, 0.8416666666666666741, 0.8458333333333333259, 0.8499999999999999778, 0.8541666666666666297, 0.8583333333333332815, 0.8625000000000000444, 0.8666666666666666963, 0.8708333333333333481, 0.8750000000000000000, 0.8791666666666666519, 0.8833333333333333037, 0.8874999999999999556, 0.8916666666666667185, 0.8958333333333333703, 0.9000000000000000222, 0.9041666666666666741, 0.9083333333333333259, 0.9124999999999999778, 0.9166666666666666297, 0.9208333333333332815, 0.9250000000000000444, 0.9291666666666666963, 0.9333333333333333481, 0.9375000000000000000, 0.9416666666666666519, 0.9458333333333333037, 0.9499999999999999556, 0.9541666666666667185, 0.9583333333333333703, 0.9625000000000000222, 0.9666666666666666741, 0.9708333333333333259, 0.9749999999999999778, 0.9791666666666666297, 0.9833333333333332815, 0.9875000000000000444, 0.9916666666666666963, 0.9958333333333333481, 1.000000000000000000 ),
 .UNSPECIFIED. ) 
 CURVE ( )  GEOMETRIC_REPRESENTATION_ITEM ( )  RATIONAL_B_SPLINE_CURVE ( ( 1.000000000000000000, 0.9807852804032304306, 1.000000000000000000, 0.9807852804032304306, 1.000000000000000000, 0.9807852804032304306, 1.000000000000000000, 0.9807852804032304306, 1.000000000000000000, 0.9807852804032304306, 1.000000000000000000, 0.9807852804032304306, 1.000000000000000000, 0.9807852804032304306, 1.000000000000000000, 0.9807852804032304306, 1.000000000000000000, 0.9807852804032304306, 1.000000000000000000, 0.9807852804032304306, 1.000000000000000000, 0.9807852804032304306, 1.000000000000000000, 0.9807852804032304306, 1.000000000000000000, 0.9807852804032304306, 1.000000000000000000, 0.9807852804032304306, 1.000000000000000000, 0.9807852804032304306, 1.000000000000000000, 0.9807852804032304306, 1.000000000000000000, 0.9807852804032304306, 1.000000000000000000, 0.9807852804032304306, 1.000000000000000000, 0.9807852804032304306, 1.000000000000000000, 0.9807852804032304306, 1.000000000000000000, 0.9807852804032304306, 1.000000000000000000, 0.9807852804032304306, 1.000000000000000000, 0.9807852804032304306, 1.000000000000000000, 0.9807852804032304306, 1.000000000000000000, 0.9807852804032304306, 1.000000000000000000, 0.9807852804032304306, 1.000000000000000000, 0.9807852804032304306, 1.000000000000000000, 0.9807852804032304306, 1.000000000000000000, 0.9807852804032304306, 1.000000000000000000, 0.9807852804032304306, 1.000000000000000000, 0.9807852804032304306, 1.000000000000000000, 0.9807852804032304306, 1.000000000000000000, 0.9807852804032304306, 1.000000000000000000, 0.9807852804032304306, 1.000000000000000000, 0.9807852804032304306, 1.000000000000000000, 0.9807852804032304306, 1.000000000000000000, 0.9807852804032304306, 1.000000000000000000, 0.9807852804032304306, 1.000000000000000000, 0.9807852804032304306, 1.000000000000000000, 0.9807852804032304306, 1.000000000000000000, 0.9807852804032304306, 1.000000000000000000, 0.9807852804032304306, 1.000000000000000000, 0.9807852804032304306, 1.000000000000000000, 0.9807852804032304306, 1.000000000000000000, 0.9807852804032304306, 1.000000000000000000, 0.9807852804032304306, 1.000000000000000000, 0.9807852804032304306, 1.000000000000000000, 0.9807852804032304306, 1.000000000000000000, 0.9807852804032304306, 1.000000000000000000, 0.9807852804032304306, 1.000000000000000000, 0.9807852804032304306, 1.000000000000000000, 0.9807852804032304306, 1.000000000000000000, 0.9807852804032304306, 1.000000000000000000, 0.9807852804032304306, 1.000000000000000000, 0.9807852804032304306, 1.000000000000000000, 0.9807852804032304306, 1.000000000000000000, 0.9807852804032304306, 1.000000000000000000, 0.9807852804032304306, 1.000000000000000000, 0.9807852804032304306, 1.000000000000000000, 0.9807852804032304306, 1.000000000000000000, 0.9807852804032304306, 1.000000000000000000, 0.9807852804032304306, 1.000000000000000000, 0.9807852804032304306, 1.000000000000000000, 0.9807852804032304306, 1.000000000000000000, 0.9807852804032304306, 1.000000000000000000, 0.9807852804032304306, 1.000000000000000000, 0.9807852804032304306, 1.000000000000000000, 0.9807852804032304306, 1.000000000000000000, 0.9807852804032304306, 1.000000000000000000, 0.9807852804032304306, 1.000000000000000000, 0.9807852804032304306, 1.000000000000000000, 0.9807852804032304306, 1.000000000000000000, 0.9807852804032304306, 1.000000000000000000, 0.9807852804032304306, 1.000000000000000000, 0.9807852804032304306, 1.000000000000000000, 0.9807852804032304306, 1.000000000000000000, 0.9807852804032304306, 1.000000000000000000, 0.9807852804032304306, 1.000000000000000000, 0.9807852804032304306, 1.000000000000000000, 0.9807852804032304306, 1.000000000000000000, 0.9807852804032304306, 1.000000000000000000, 0.9807852804032304306, 1.000000000000000000, 0.9807852804032304306, 1.000000000000000000, 0.9807852804032304306, 1.000000000000000000, 0.9807852804032304306, 1.000000000000000000, 0.9807852804032304306, 1.000000000000000000, 0.9807852804032304306, 1.000000000000000000, 0.9807852804032304306, 1.000000000000000000, 0.9807852804032304306, 1.000000000000000000, 0.9807852804032304306, 1.000000000000000000, 0.9807852804032304306, 1.000000000000000000, 0.9807852804032304306, 1.000000000000000000, 0.9807852804032304306, 1.000000000000000000, 0.9807852804032304306, 1.000000000000000000, 0.9807852804032304306, 1.000000000000000000, 0.9807852804032304306, 1.000000000000000000, 0.9807852804032304306, 1.000000000000000000, 0.9807852804032304306, 1.000000000000000000, 0.9807852804032304306, 1.000000000000000000, 0.9807852804032304306, 1.000000000000000000, 0.9807852804032304306, 1.000000000000000000, 0.9807852804032304306, 1.000000000000000000, 0.9807852804032304306, 1.000000000000000000, 0.9807852804032304306, 1.000000000000000000, 0.9807852804032304306, 1.000000000000000000, 0.9807852804032304306, 1.000000000000000000, 0.9807852804032304306, 1.000000000000000000, 0.9807852804032304306, 1.000000000000000000, 0.9807852804032304306, 1.000000000000000000, 0.9807852804032304306, 1.000000000000000000, 0.9807852804032304306, 1.000000000000000000, 0.9807852804032304306, 1.000000000000000000, 0.9807852804032304306, 1.000000000000000000, 0.9807852804032304306, 1.000000000000000000, 0.9807852804032304306, 1.000000000000000000, 0.9807852804032304306, 1.000000000000000000, 0.9807852804032304306, 1.000000000000000000, 0.9807852804032304306, 1.000000000000000000, 0.9807852804032304306, 1.000000000000000000, 0.9807852804032304306, 1.000000000000000000, 0.9807852804032304306, 1.000000000000000000, 0.9807852804032304306, 1.000000000000000000, 0.9807852804032304306, 1.000000000000000000, 0.9807852804032304306, 1.000000000000000000, 0.9807852804032304306, 1.000000000000000000, 0.9807852804032304306, 1.000000000000000000, 0.9807852804032304306, 1.000000000000000000, 0.9807852804032304306, 1.000000000000000000, 0.9807852804032304306, 1.000000000000000000, 0.9807852804032304306, 1.000000000000000000, 0.9807852804032304306, 1.000000000000000000, 0.9807852804032304306, 1.000000000000000000, 0.9807852804032304306, 1.000000000000000000, 0.9807852804032304306, 1.000000000000000000, 0.9807852804032304306, 1.000000000000000000, 0.9807852804032304306, 1.000000000000000000, 0.9807852804032304306, 1.000000000000000000, 0.9807852804032304306, 1.000000000000000000, 0.9807852804032304306, 1.000000000000000000, 0.9807852804032304306, 1.000000000000000000, 0.9807852804032304306, 1.000000000000000000, 0.9807852804032304306, 1.000000000000000000, 0.9807852804032304306, 1.000000000000000000, 0.9807852804032304306, 1.000000000000000000, 0.9807852804032304306, 1.000000000000000000, 0.9807852804032304306, 1.000000000000000000, 0.9807852804032304306, 1.000000000000000000, 0.9807852804032304306, 1.000000000000000000, 0.9807852804032304306, 1.000000000000000000, 0.9807852804032304306, 1.000000000000000000, 0.9807852804032304306, 1.000000000000000000, 0.9807852804032304306, 1.000000000000000000, 0.9807852804032304306, 1.000000000000000000, 0.9807852804032304306, 1.000000000000000000, 0.9807852804032304306, 1.000000000000000000, 0.9807852804032304306, 1.000000000000000000, 0.9807852804032304306, 1.000000000000000000, 0.9807852804032304306, 1.000000000000000000, 0.9807852804032304306, 1.000000000000000000, 0.9807852804032304306, 1.000000000000000000, 0.9807852804032304306, 1.000000000000000000, 0.9807852804032304306, 1.000000000000000000, 0.9807852804032304306, 1.000000000000000000, 0.9807852804032304306, 1.000000000000000000, 0.9807852804032304306, 1.000000000000000000, 0.9807852804032304306, 1.000000000000000000, 0.9807852804032304306, 1.000000000000000000, 0.9807852804032304306, 1.000000000000000000, 0.9807852804032304306, 1.000000000000000000, 0.9807852804032304306, 1.000000000000000000, 0.9807852804032304306, 1.000000000000000000, 0.9807852804032304306, 1.000000000000000000, 0.9807852804032304306, 1.000000000000000000, 0.9807852804032304306, 1.000000000000000000, 0.9807852804032304306, 1.000000000000000000, 0.9807852804032304306, 1.000000000000000000, 0.9807852804032304306, 1.000000000000000000, 0.9807852804032304306, 1.000000000000000000, 0.9807852804032304306, 1.000000000000000000, 0.9807852804032304306, 1.000000000000000000, 0.9807852804032304306, 1.000000000000000000, 0.9807852804032304306, 1.000000000000000000, 0.9807852804032304306, 1.000000000000000000, 0.9807852804032304306, 1.000000000000000000, 0.9807852804032304306, 1.000000000000000000, 0.9807852804032304306, 1.000000000000000000, 0.9807852804032304306, 1.000000000000000000, 0.9807852804032304306, 1.000000000000000000, 0.9807852804032304306, 1.000000000000000000, 0.9807852804032304306, 1.000000000000000000, 0.9807852804032304306, 1.000000000000000000, 0.9807852804032304306, 1.000000000000000000, 0.9807852804032304306, 1.000000000000000000, 0.9807852804032304306, 1.000000000000000000, 0.9807852804032304306, 1.000000000000000000, 0.9807852804032304306, 1.000000000000000000, 0.9807852804032304306, 1.000000000000000000, 0.9807852804032304306, 1.000000000000000000, 0.9807852804032304306, 1.000000000000000000, 0.9807852804032304306, 1.000000000000000000, 0.9807852804032304306, 1.000000000000000000, 0.9807852804032304306, 1.000000000000000000, 0.9807852804032304306, 1.000000000000000000, 0.9807852804032304306, 1.000000000000000000, 0.9807852804032304306, 1.000000000000000000, 0.9807852804032304306, 1.000000000000000000, 0.9807852804032304306, 1.000000000000000000, 0.9807852804032304306, 1.000000000000000000, 0.9807852804032304306, 1.000000000000000000, 0.9807852804032304306, 1.000000000000000000, 0.9807852804032304306, 1.000000000000000000, 0.9807852804032304306, 1.000000000000000000, 0.9807852804032304306, 1.000000000000000000, 0.9807852804032304306, 1.000000000000000000, 0.9807852804032304306, 1.000000000000000000, 0.9807852804032304306, 1.000000000000000000, 0.9807852804032304306, 1.000000000000000000, 0.9807852804032304306, 1.000000000000000000, 0.9807852804032304306, 1.000000000000000000, 0.9807852804032304306, 1.000000000000000000, 0.9807852804032304306, 1.000000000000000000, 0.9807852804032304306, 1.000000000000000000, 0.9807852804032304306, 1.000000000000000000, 0.9807852804032304306, 1.000000000000000000, 0.9807852804032304306, 1.000000000000000000, 0.9807852804032304306, 1.000000000000000000, 0.9807852804032304306, 1.000000000000000000, 0.9807852804032304306, 1.000000000000000000, 0.9807852804032304306, 1.000000000000000000, 0.9807852804032304306, 1.000000000000000000, 0.9807852804032304306, 1.000000000000000000, 0.9807852804032304306, 1.000000000000000000, 0.9807852804032304306, 1.000000000000000000, 0.9807852804032304306, 1.000000000000000000, 0.9807852804032304306, 1.000000000000000000, 0.9807852804032304306, 1.000000000000000000, 0.9807852804032304306, 1.000000000000000000, 0.9807852804032304306, 1.000000000000000000, 0.9807852804032304306, 1.000000000000000000, 0.9807852804032304306, 1.000000000000000000 ) ) 
 REPRESENTATION_ITEM ( '' )  );
#7396 = DIRECTION ( 'NONE',  ( 0.000000000000000000, 0.000000000000000000, 1.000000000000000000 ) ) ;
#7397 = CARTESIAN_POINT ( 'NONE',  ( 27.69224003142016954, -5.196152422706638241, 160.9137933187836609 ) ) ;
#7398 = CARTESIAN_POINT ( 'NONE',  ( 15.24356964375000167, 242.6968750006145399, 3.323476615752272600 ) ) ;
#7399 = CARTESIAN_POINT ( 'NONE',  ( 11.48171059495408208, 139.3148137178985451, -4.944772684328420986 ) ) ;
#7400 = CARTESIAN_POINT ( 'NONE',  ( 27.24356964375000345, 196.9343750006145228, -3.336375036156643733E-15 ) ) ;
#7402 = ORIENTED_EDGE ( 'NONE', *, *, #33282, .T. ) ;
#7401 = ORIENTED_EDGE ( 'NONE', *, *, #23703, .F. ) ;
#7403 = CIRCLE ( 'NONE', #29156, 27.00000000000000000 ) ;
#7404 = CARTESIAN_POINT ( 'NONE',  ( 26.75643035624999655, 245.5093750006145115, -3.323476615752271712 ) ) ;
#7405 = CARTESIAN_POINT ( 'NONE',  ( 7.228626920338837358, 21.72731371789854293, 10.49813415416005036 ) ) ;
#7406 = CARTESIAN_POINT ( 'NONE',  ( 15.24356964374999990, 3.323476615752268604, -4.228124999385472371 ) ) ;
#7407 = CARTESIAN_POINT ( 'NONE',  ( 6.092822981423662299, 104.8148137178985593, 14.25334919248795096 ) ) ;
#7408 = EDGE_CURVE ( 'NONE', #35545, #16460, #15649, .T. ) ;
#7409 = CARTESIAN_POINT ( 'NONE',  ( 13.56230152254410903, 5.196152422706636465, -2.325000000000049027 ) ) ;
#7410 = CARTESIAN_POINT ( 'NONE',  ( 26.99999999999999645, 3.464101615137755275, -8.681249998770958598 ) ) ;
#7411 = ORIENTED_EDGE ( 'NONE', *, *, #16798, .T. ) ;
#7412 = CARTESIAN_POINT ( 'NONE',  ( 16.56230152254411792, 7.209453229046482114, -7.059374999385484628 ) ) ;
#7413 = ADVANCED_FACE ( 'NONE', ( #6737 ), #18311, .T. ) ;
#7414 = ORIENTED_EDGE ( 'NONE', *, *, #35342, .F. ) ;
#7415 = CARTESIAN_POINT ( 'NONE',  ( 13.62178482187499640, 196.9531250006145342, -23.59362340125807123 ) ) ;
#7416 = CARTESIAN_POINT ( 'NONE',  ( 0.1745138560725515708, 125.4101862821014635, -12.50000000000000355 ) ) ;
#7417 = CARTESIAN_POINT ( 'NONE',  ( 13.44051670066911441, 5.407089921784856479, -0.6656249993855500868 ) ) ;
#7418 = CARTESIAN_POINT ( 'NONE',  ( 30.76498388983966237, 7.209453229046482114, 161.6142765964977741 ) ) ;
#7419 = EDGE_CURVE ( 'NONE', #456, #31856, #32884, .T. ) ;
#7420 =( BOUNDED_CURVE ( )  B_SPLINE_CURVE ( 2, ( #26297, #2807, #6215, #32549, #29331, #23100, #148, #8688, #23850 ),
 .UNSPECIFIED., .F., .F. ) 
 B_SPLINE_CURVE_WITH_KNOTS ( ( 3, 2, 2, 2, 3 ),
 ( 0.8125000000000000000, 0.8194444444444444198, 0.8333333333333333703, 0.8472222222222222099, 0.8541666666666667407 ),
 .UNSPECIFIED. ) 
 CURVE ( )  GEOMETRIC_REPRESENTATION_ITEM ( )  RATIONAL_B_SPLINE_CURVE ( ( 0.9330127018922194093, 0.9330127018922194093, 1.000000000000000000, 0.8660254037844387076, 1.000000000000000000, 0.8660254037844387076, 1.000000000000000000, 0.9330127018922187432, 0.9330127018922192983 ) ) 
 REPRESENTATION_ITEM ( '' )  );
#7421 = CARTESIAN_POINT ( 'NONE',  ( -49.40252896937850124, 205.6499508600178103, -7.303452534266820173 ) ) ;
#7422 = CARTESIAN_POINT ( 'NONE',  ( 15.24356964375000167, 246.1843750006145513, 3.323476615752272600 ) ) ;
#7423 = PRODUCT_DEFINITION ( 'UNKNOWN', '', #32950, #9257 ) ;
#7424 = CARTESIAN_POINT ( 'NONE',  ( -1.045839947578415010E-13, 196.5125000000000455, 27.00000000000000355 ) ) ;
#7425 = CARTESIAN_POINT ( 'NONE',  ( -38.12127896937850835, 214.5309553116392749, 1.090244570138288127 ) ) ;
#7426 = CARTESIAN_POINT ( 'NONE',  ( 4.944772684328679446, 135.1851862821014549, -11.48171059495397373 ) ) ;
#7427 = CARTESIAN_POINT ( 'NONE',  ( 10.31873187879410736, 0.000000000000000000, -10.09687499938552513 ) ) ;
#7428 = ORIENTED_EDGE ( 'NONE', *, *, #16906, .F. ) ;
#7429 = CARTESIAN_POINT ( 'NONE',  ( 27.00000000000001421, 195.3500000012290343, 15.58845726811988897 ) ) ;
#7430 = CARTESIAN_POINT ( 'NONE',  ( -8.927990412390661490, 112.4726862821014635, 13.04141134922759804 ) ) ;
#7431 = CARTESIAN_POINT ( 'NONE',  ( 6.594114490232313663, 119.6601862821014635, 6.840914352312096547 ) ) ;
#7432 = CARTESIAN_POINT ( 'NONE',  ( 1.069080835302379631E-14, 199.2125000000000057, 27.00000000000000000 ) ) ;
#7433 = CARTESIAN_POINT ( 'NONE',  ( 2.660918448318279950, 6.097686282101443922, -12.46528703574805697 ) ) ;
#7434 = AXIS2_PLACEMENT_3D ( 'NONE', #27806, #30088, #15882 ) ;
#7435 = CARTESIAN_POINT ( 'NONE',  ( 22.56230152254412857, -3.464101615137755275, -8.812500000000058620 ) ) ;
#7436 = ORIENTED_EDGE ( 'NONE', *, *, #7888, .F. ) ;
#7437 = CARTESIAN_POINT ( 'NONE',  ( -6.840914352312096547, 85.16018628210146346, 6.594114490232313663 ) ) ;
#7438 = CARTESIAN_POINT ( 'NONE',  ( 6.840914352311949109, 131.8398137178985792, 6.594114490232462877 ) ) ;
#7439 = CARTESIAN_POINT ( 'NONE',  ( -27.24356964374999635, 195.7906250006145115, 15.72908226750539384 ) ) ;
#7440 = LINE ( 'NONE', #16532, #28065 ) ;
#7441 = CARTESIAN_POINT ( 'NONE',  ( 13.62178482187499640, 198.8093750006145513, -23.59362340125807123 ) ) ;
#7442 = DIRECTION ( 'NONE',  ( -1.000000000000000000, 0.000000000000000000, 0.000000000000000000 ) ) ;
#7443 = FACE_OUTER_BOUND ( 'NONE', #5198, .T. ) ;
#7444 = CARTESIAN_POINT ( 'NONE',  ( -9.465287035748106703, 61.40231371789855785, 2.064181346179061460 ) ) ;
#7445 = ORIENTED_EDGE ( 'NONE', *, *, #12185, .T. ) ;
#7446 = CARTESIAN_POINT ( 'NONE',  ( 15.00000000000000178, 241.9937500012290457, 3.464101615137757051 ) ) ;
#7447 = CARTESIAN_POINT ( 'NONE',  ( -6.932735513424201912, 78.65231371789856496, 10.69584247140429412 ) ) ;
#7448 = CARTESIAN_POINT ( 'NONE',  ( 16.56230152254411436, -7.209453229046482114, -5.934374999385510385 ) ) ;
#7449 = CARTESIAN_POINT ( 'NONE',  ( -14.00000000000001599, 143.0000000000000000, 1.203016833088524695 ) ) ;
#7450 = CARTESIAN_POINT ( 'NONE',  ( 18.12178482187500350, -4.985214923628407568, -7.828124999385482674 ) ) ;
#7451 = CARTESIAN_POINT ( 'NONE',  ( 4.944772684328420986, 40.41481371789855359, 11.48171059495408208 ) ) ;
#7452 = MANIFOLD_SOLID_BREP ( 'Thread1', #29547 ) ;
#7453 = ORIENTED_EDGE ( 'NONE', *, *, #23541, .T. ) ;
#7454 = CARTESIAN_POINT ( 'NONE',  ( 15.24356964375000167, -3.323476615752272600, -6.853124999385484806 ) ) ;
#7455 = CARTESIAN_POINT ( 'NONE',  ( 6.932735513423970097, 27.94768628210143646, 10.69584247140445044 ) ) ;
#7456 = CARTESIAN_POINT ( 'NONE',  ( 19.56230152254410370, 5.196152422706631135, -9.487499998770992704 ) ) ;
#7457 = CARTESIAN_POINT ( 'NONE',  ( -50.98586230271183695, 206.8500491399821328, 5.686928522499748340 ) ) ;
#7458 = CARTESIAN_POINT ( 'NONE',  ( 27.70204505258639216, -5.196152422706632912, 161.0258652235433487 ) ) ;
#7459 = CARTESIAN_POINT ( 'NONE',  ( -11.48171059495408208, 61.11481371789854933, 4.944772684328421875 ) ) ;
#7460 = CARTESIAN_POINT ( 'NONE',  ( -49.60788769728823411, 214.4690446883608104, 1.321298161741840893 ) ) ;
#7461 = CARTESIAN_POINT ( 'NONE',  ( -59.10788769728823411, 216.4690446883607535, 1.857196546604031662 ) ) ;
#7462 = EDGE_CURVE ( 'NONE', #11777, #8243, #28691, .T. ) ;
#7463 = LINE ( 'NONE', #4608, #20972 ) ;
#7464 = CARTESIAN_POINT ( 'NONE',  ( 13.56230152254411792, -5.196152422706638241, -6.225000000000063594 ) ) ;
#7465 = CARTESIAN_POINT ( 'NONE',  ( 14.25334919248795451, 38.11481371789853512, -6.092822981423661410 ) ) ;
#7466 = CARTESIAN_POINT ( 'NONE',  ( -45.24627896937850835, 201.4690446883607251, -2.162041339862721845 ) ) ;
#7467 = STYLED_ITEM ( 'NONE', ( #17344 ), #35907 ) ;
#7468 = CARTESIAN_POINT ( 'NONE',  ( 26.99999999999999645, 199.8125000000000000, -15.58845726811990495 ) ) ;
#7469 = CARTESIAN_POINT ( 'NONE',  ( -8.962234695871760692, 66.76018628210145778, 8.715434833791933400 ) ) ;
#7470 = CARTESIAN_POINT ( 'NONE',  ( -15.53471296425195369, 12.42268628210144144, 2.908627838312118019 ) ) ;
#7471 = CARTESIAN_POINT ( 'NONE',  ( 22.56230152254411792, 3.464101615137759271, -1.537500000000068257 ) ) ;
#7472 = CARTESIAN_POINT ( 'NONE',  ( 20.99999999999999645, 192.3000000000000398, -8.000000000000000000 ) ) ;
#7473 = ORIENTED_EDGE ( 'NONE', *, *, #16912, .T. ) ;
#7474 = CARTESIAN_POINT ( 'NONE',  ( -14.25334919248782306, 22.48518628210144499, -6.092822981423979378 ) ) ;
#7475 = CARTESIAN_POINT ( 'NONE',  ( 13.62178482187501416, 198.1531250006145228, 23.59362340125806767 ) ) ;
#7476 = CARTESIAN_POINT ( 'NONE',  ( 22.56230152254410370, 7.347880794884117764E-16, -8.662499998771028942 ) ) ;
#7477 = CARTESIAN_POINT ( 'NONE',  ( 21.00000000000001066, 247.4124999999999943, 5.999999999999998224 ) ) ;
#7478 = EDGE_CURVE ( 'NONE', #24079, #22329, #19622, .T. ) ;
#7479 = CARTESIAN_POINT ( 'NONE',  ( -7.234628195640302017, 195.5924038105676743, 27.00000000000000711 ) ) ;
#7480 = AXIS2_PLACEMENT_3D ( 'NONE', #13535, #10684, #1595 ) ;
#7481 = CARTESIAN_POINT ( 'NONE',  ( 21.00000000000000000, 246.8218750006145399, 6.646953231504538984 ) ) ;
#7482 = CARTESIAN_POINT ( 'NONE',  ( 0.1745138560723095977, 114.5898137178985650, 9.500000000000005329 ) ) ;
#7483 = CARTESIAN_POINT ( 'NONE',  ( 15.24356964374999990, 244.0093750006145399, 0.000000000000000000 ) ) ;
#7484 = EDGE_CURVE ( 'NONE', #29149, #21861, #21895, .T. ) ;
#7485 = ORIENTED_EDGE ( 'NONE', *, *, #24532, .T. ) ;
#7486 =( LENGTH_UNIT ( ) NAMED_UNIT ( * ) SI_UNIT ( .MILLI., .METRE. ) );
#7487 = CARTESIAN_POINT ( 'NONE',  ( 25.16449192692294545, 3.464101615137650025, 166.4426400131867751 ) ) ;
#7488 = CARTESIAN_POINT ( 'NONE',  ( 2.660918448318003282, 141.9023137178985792, 12.46528703574811558 ) ) ;
#7489 = CARTESIAN_POINT ( 'NONE',  ( 10.31873187879410914, 0.000000000000000000, -8.690624999385526905 ) ) ;
#7490 = CARTESIAN_POINT ( 'NONE',  ( 31.00520690578787253, 7.209453229046475009, 164.3600382331131300 ) ) ;
#7491 = CARTESIAN_POINT ( 'NONE',  ( 5.999999999999999112, -30.00000000000000000, -19.99999999999999289 ) ) ;
#7492 = CARTESIAN_POINT ( 'NONE',  ( 27.00000000000001066, 197.4875000000000114, 15.58845726811988897 ) ) ;
#7493 = ORIENTED_EDGE ( 'NONE', *, *, #24996, .F. ) ;
#7494 = CARTESIAN_POINT ( 'NONE',  ( -10.69584247140444866, 39.44768628210145067, 6.932735513423972762 ) ) ;
#7495 = ORIENTED_EDGE ( 'NONE', *, *, #19453, .F. ) ;
#7496 = VERTEX_POINT ( 'NONE', #25098 ) ;
#7497 = CARTESIAN_POINT ( 'NONE',  ( 18.00000000000000000, 5.196152422706630247, -5.868749998770961263 ) ) ;
#7498 = CARTESIAN_POINT ( 'NONE',  ( -9.000000000000024869, 210.0000000000000000, 0.000000000000000000 ) ) ;
#7499 = CARTESIAN_POINT ( 'NONE',  ( 20.99999999999997513, 247.1875000000000284, -5.999999999999999112 ) ) ;
#7501 = CARTESIAN_POINT ( 'NONE',  ( 3.306546357697854128E-15, 200.0000000000000000, 27.00000000000000355 ) ) ;
#7500 =( GEOMETRIC_REPRESENTATION_CONTEXT ( 3 ) GLOBAL_UNCERTAINTY_ASSIGNED_CONTEXT ( ( #903 ) ) GLOBAL_UNIT_ASSIGNED_CONTEXT ( ( #4566, #10070, #33195 ) ) REPRESENTATION_CONTEXT ( 'NONE', 'WORKASPACE' ) );
#7502 = CARTESIAN_POINT ( 'NONE',  ( 18.12178482187499640, 4.985214923628404904, -8.765624999385462246 ) ) ;
#7503 = CARTESIAN_POINT ( 'NONE',  ( 2.311890736173175753, 83.72268628210143504, 12.53471296425194836 ) ) ;
#7504 = CARTESIAN_POINT ( 'NONE',  ( -13.23911966647199812, 7.352313717898546486, -8.632099005475788900 ) ) ;
#7505 = CIRCLE ( 'NONE', #6906, 8.000000000000000000 ) ;
#7506 = CARTESIAN_POINT ( 'NONE',  ( -66.62127896937847993, 216.5309553116392181, 1.626142955000506429 ) ) ;
#7507 = CARTESIAN_POINT ( 'NONE',  ( 20.99999999999999645, 210.0000000000000000, 5.999999999999996447 ) ) ;
#7508 = CARTESIAN_POINT ( 'NONE',  ( -56.13169563604517265, 210.1155267958017703, 4.499999999999996447 ) ) ;
#7509 = CARTESIAN_POINT ( 'NONE',  ( 13.49999999999999645, 197.1500000000000057, -23.38268590217984766 ) ) ;
#7510 = CARTESIAN_POINT ( 'NONE',  ( 25.33771396574120516, -3.464101615137757051, 168.4225769768684131 ) ) ;
#7511 = CARTESIAN_POINT ( 'NONE',  ( -10.69584247140429412, 117.7523137178986019, -6.932735513424201024 ) ) ;
#7512 = CARTESIAN_POINT ( 'NONE',  ( -45.64955436395490551, 214.8429017333601792, -4.673758765035196383 ) ) ;
#7513 = MANIFOLD_SOLID_BREP ( 'Extrude-Thin1', #1999 ) ;
#7514 = CARTESIAN_POINT ( 'NONE',  ( -55.34747103062157692, 214.3500491399821044, -7.303452534266878793 ) ) ;
#7515 = EDGE_CURVE ( 'NONE', #25852, #19565, #24912, .T. ) ;
#7516 = CARTESIAN_POINT ( 'NONE',  ( 26.75643035624999655, 3.323476615752271268, -2.240624999385472549 ) ) ;
#7517 = CARTESIAN_POINT ( 'NONE',  ( -13.62178482187498396, 195.3781250006145171, 23.59362340125808188 ) ) ;
#7518 = CARTESIAN_POINT ( 'NONE',  ( 13.23911966647199812, 94.75231371789854506, 8.632099005475788900 ) ) ;
#7519 = CARTESIAN_POINT ( 'NONE',  ( -41.68377896937849414, 208.3738570449995109, 6.530955311639247363 ) ) ;
#7520 = ORIENTED_EDGE ( 'NONE', *, *, #26777, .F. ) ;
#7521 = CARTESIAN_POINT ( 'NONE',  ( -77.00000000000002842, 214.0000000000000000, -2.499999999999998668 ) ) ;
#7522 = CARTESIAN_POINT ( 'NONE',  ( -8.962234695871760692, 121.9601862821014464, 8.715434833791933400 ) ) ;
#7523 = CARTESIAN_POINT ( 'NONE',  ( -13.23911966647218463, 76.24768628210145494, 8.632099005475506459 ) ) ;
#7524 = DIRECTION ( 'NONE',  ( -0.1219804832088933616, -0.9925324990730152175, 0.000000000000000000 ) ) ;
#7525 = CARTESIAN_POINT ( 'NONE',  ( 24.87200694887302532, -3.604726614523244610, 165.8941696640395378 ) ) ;
#7526 = AXIS2_PLACEMENT_3D ( 'NONE', #13681, #16709, #22024 ) ;
#7527 = CARTESIAN_POINT ( 'NONE',  ( 15.50000000000000533, 81.71018628210144641, 0.1745138560725827404 ) ) ;
#7528 = CARTESIAN_POINT ( 'NONE',  ( -57.12872103062157692, 203.4690446883607535, 1.626142955000567936 ) ) ;
#7529 = AXIS2_PLACEMENT_3D ( 'NONE', #20789, #9780, #12624 ) ;
#7530 = CARTESIAN_POINT ( 'NONE',  ( 19.68408634441910365, 5.407089921784857367, -4.340624999385561900 ) ) ;
#7531 = CARTESIAN_POINT ( 'NONE',  ( -8.152565276336710909, 39.44768628210144357, 5.233372021372435512 ) ) ;
#7532 = DIRECTION ( 'NONE',  ( -0.000000000000000000, -1.000000000000000000, -0.000000000000000000 ) ) ;
#7533 = CARTESIAN_POINT ( 'NONE',  ( -35.15997103062156270, 217.3034525342668815, 4.350049139982096413 ) ) ;
#7534 = EDGE_CURVE ( 'NONE', #10561, #23659, #9331, .T. ) ;
#7535 = FACE_OUTER_BOUND ( 'NONE', #23386, .T. ) ;
#7536 = CARTESIAN_POINT ( 'NONE',  ( 4.622313124798573369, 65.03518628210144925, 11.61527771782819940 ) ) ;
#7537 = CARTESIAN_POINT ( 'NONE',  ( -13.50000000000000533, 199.9250000000000114, -23.38268590217984411 ) ) ;
#7538 = CARTESIAN_POINT ( 'NONE',  ( 26.97716818855048260, 0.000000000000000000, 49.47706554351410801 ) ) ;
#7540 = CARTESIAN_POINT ( 'NONE',  ( 16.56230152254411436, 7.209453229046482114, -1.209374999385475657 ) ) ;
#7539 = CARTESIAN_POINT ( 'NONE',  ( -9.534712964251941258, 49.22268628210144215, 1.715153634034234154 ) ) ;
#7541 = DIRECTION ( 'NONE',  ( -1.000000000000000000, 0.000000000000000000, 0.000000000000000000 ) ) ;
#7542 = ORIENTED_EDGE ( 'NONE', *, *, #17513, .F. ) ;
#7543 = CARTESIAN_POINT ( 'NONE',  ( 15.00000000000000178, -3.464101615137757051, -1.762499999999985967 ) ) ;
#7544 = CARTESIAN_POINT ( 'NONE',  ( 37.05669835387679711, 3.604726614523243278, 161.8919742727257187 ) ) ;
#7545 = CARTESIAN_POINT ( 'NONE',  ( 30.76253263452132458, -6.928203230275514990, 161.5862586200017574 ) ) ;
#7546 = CARTESIAN_POINT ( 'NONE',  ( 15.00000000000000178, 245.9874999999999829, 3.464101615137757051 ) ) ;
#7547 = LINE ( 'NONE', #10194, #28748 ) ;
#7548 = CARTESIAN_POINT ( 'NONE',  ( 12.46528703574811558, 93.60231371789855359, -2.660918448318005503 ) ) ;
#7549 = CARTESIAN_POINT ( 'NONE',  ( -11.48171059495397373, 86.88518628210145778, -4.944772684328680334 ) ) ;
#7550 = ORIENTED_EDGE ( 'NONE', *, *, #17453, .T. ) ;
#7551 = VERTEX_POINT ( 'NONE', #30425 ) ;
#7552 = CARTESIAN_POINT ( 'NONE',  ( -27.00000000000000355, 197.4125000012290343, 0.000000000000000000 ) ) ;
#7553 = CARTESIAN_POINT ( 'NONE',  ( 15.00000000000000178, 248.7437500012290457, 3.464101615137757051 ) ) ;
#7554 = CARTESIAN_POINT ( 'NONE',  ( -0.1745138560722442889, 63.98981371789855643, -15.50000000000000533 ) ) ;
#7555 = CARTESIAN_POINT ( 'NONE',  ( 15.24356964375000167, -3.323476615752272600, -6.515624999385480010 ) ) ;
#7556 = CARTESIAN_POINT ( 'NONE',  ( 26.75643035624999655, 244.6843750006145228, -7.049594010296217766E-16 ) ) ;
#7557 = CARTESIAN_POINT ( 'NONE',  ( -55.74330436395489841, 210.1155267958017703, -4.499999999999996447 ) ) ;
#7558 = ADVANCED_FACE ( 'NONE', ( #16025 ), #27574, .T. ) ;
#7559 = CARTESIAN_POINT ( 'NONE',  ( 26.99999999999999645, 7.347880794884117764E-16, -7.424999999999987388 ) ) ;
#7560 = CARTESIAN_POINT ( 'NONE',  ( 8.152565276336593669, 39.55231371789854933, 5.233372021372610483 ) ) ;
#7561 = CARTESIAN_POINT ( 'NONE',  ( 10.31873187879410736, 0.000000000000000000, -6.890624999385530636 ) ) ;
#7562 = CARTESIAN_POINT ( 'NONE',  ( 9.465287035748106703, 93.60231371789855359, -2.064181346179063237 ) ) ;
#7563 = CARTESIAN_POINT ( 'NONE',  ( 13.62178482187501416, 198.2093750006145285, 23.59362340125806767 ) ) ;
#7564 = CARTESIAN_POINT ( 'NONE',  ( -6.932735513424201912, 23.45231371789854791, 10.69584247140429412 ) ) ;
#7565 = CARTESIAN_POINT ( 'NONE',  ( 10.49813415415989581, 91.77268628210144641, 7.228626920339068285 ) ) ;
#7566 = CARTESIAN_POINT ( 'NONE',  ( 22.56230152254410370, 3.464101615137755275, -8.624999998771011533 ) ) ;
#7567 = DIRECTION ( 'NONE',  ( 0.000000000000000000, 0.000000000000000000, -1.000000000000000000 ) ) ;
#7568 = CARTESIAN_POINT ( 'NONE',  ( 36.94394061169700905, 3.604726614523238837, 160.6031473820695226 ) ) ;
#7569 = CARTESIAN_POINT ( 'NONE',  ( 28.19883278624800127, 5.196152422706630247, 166.7041750026663181 ) ) ;
#7570 = CARTESIAN_POINT ( 'NONE',  ( 16.56230152254411436, -7.209453229046482114, -6.384374999385507010 ) ) ;
#7571 = CARTESIAN_POINT ( 'NONE',  ( 36.86716609684025059, 7.347880794884125653E-16, 162.5202589094750181 ) ) ;
#7572 = CARTESIAN_POINT ( 'NONE',  ( 29.53112584896062032, 5.988803496771940793, 159.6272768299058669 ) ) ;
#7573 = CARTESIAN_POINT ( 'NONE',  ( -6.594114490232312775, 87.46018628210146062, -6.840914352312096547 ) ) ;
#7574 = CARTESIAN_POINT ( 'NONE',  ( 10.56230152254394916, 3.464101615137665124, -5.887500000000066791 ) ) ;
#7575 = CARTESIAN_POINT ( 'NONE',  ( -12.53471296425194836, 122.8226862821014720, 2.311890736173176641 ) ) ;
#7576 = CARTESIAN_POINT ( 'NONE',  ( 4.999999999999998224, 216.0000000000000000, 3.514718625761427795 ) ) ;
#7577 = CARTESIAN_POINT ( 'NONE',  ( 15.24356964375000167, 249.4468750006145399, 3.323476615752272600 ) ) ;
#7578 = ORIENTED_EDGE ( 'NONE', *, *, #20721, .T. ) ;
#7579 = CARTESIAN_POINT ( 'NONE',  ( 37.29365302947196881, 7.646167579472015790E-16, 164.6003786081626572 ) ) ;
#7580 = CARTESIAN_POINT ( 'NONE',  ( 23.87821517812500005, -4.985214923628404016, -5.840624999385479299 ) ) ;
#7581 = CARTESIAN_POINT ( 'NONE',  ( 27.24356964375000345, 196.9343750006145228, -3.336375036156643733E-15 ) ) ;
#7582 = CARTESIAN_POINT ( 'NONE',  ( 18.85832510013969454, 5.387298466171131395, -8.000000000000000000 ) ) ;
#7583 = AXIS2_PLACEMENT_3D ( 'NONE', #6691, #32084, #14654 ) ;
#7584 = CARTESIAN_POINT ( 'NONE',  ( 37.38029553226704138, 3.464101615137759271, 168.3853551944901596 ) ) ;
#7585 = CARTESIAN_POINT ( 'NONE',  ( 16.56230152254410726, 0.000000000000000000, -10.00000000000000000 ) ) ;
#7586 = CARTESIAN_POINT ( 'NONE',  ( 23.87821517812499650, 243.4093750006145171, -4.985214923628404904 ) ) ;
#7587 = CARTESIAN_POINT ( 'NONE',  ( 29.48995970988985604, 6.148715791637016537, 159.4803054849043917 ) ) ;
#7588 = CIRCLE ( 'NONE', #34813, 2.649999999999992806 ) ;
#7589 = CARTESIAN_POINT ( 'NONE',  ( 3.474262827703532341, 9.364813717898543999, -8.843639120294245259 ) ) ;
#7590 = CARTESIAN_POINT ( 'NONE',  ( 27.24356964375000700, 195.0968750006145456, 15.72908226750537075 ) ) ;
#7592 = EDGE_LOOP ( 'NONE', ( #1256, #9796, #27771, #14858 ) ) ;
#7591 = ORIENTED_EDGE ( 'NONE', *, *, #12440, .T. ) ;
#7593 = CARTESIAN_POINT ( 'NONE',  ( 26.75643035624999655, 245.0593750006144944, -3.323476615752271712 ) ) ;
#7594 = LINE ( 'NONE', #22193, #32849 ) ;
#7595 = CARTESIAN_POINT ( 'NONE',  ( 18.12178482187499640, 4.985214923628404904, -3.815624999385480720 ) ) ;
#7596 = CARTESIAN_POINT ( 'NONE',  ( 0.1745138560722461762, 105.3898137178985479, 15.50000000000000533 ) ) ;
#7597 = DIRECTION ( 'NONE',  ( -0.8083506638593009885, -0.5887012860850802110, 1.927470528863119295E-16 ) ) ;
#7598 = CARTESIAN_POINT ( 'NONE',  ( 21.00000000000000000, 6.928203230275506996, -8.606249998770964638 ) ) ;
#7599 = CARTESIAN_POINT ( 'NONE',  ( 10.31873187879410736, 0.000000000000000000, -7.396874999385516958 ) ) ;
#7600 = EDGE_LOOP ( 'NONE', ( #16594, #26037, #26562, #27503 ) ) ;
#7601 = CARTESIAN_POINT ( 'NONE',  ( -1.909035429704832693E-15, 199.1000000012290627, -31.17691453623979214 ) ) ;
#7602 = CARTESIAN_POINT ( 'NONE',  ( 11.61527771782819940, 136.3351862821014606, -4.622313124798573369 ) ) ;
#7603 = CARTESIAN_POINT ( 'NONE',  ( 13.44051670066911264, 5.407089921784856479, -1.565624999385561988 ) ) ;
#7604 = CARTESIAN_POINT ( 'NONE',  ( -54.74627896937850835, 201.4690446883607251, -2.162041339862721845 ) ) ;
#7605 = CARTESIAN_POINT ( 'NONE',  ( 15.24356964374999990, 247.4593750006145285, -3.323476615752268604 ) ) ;
#7606 = AXIS2_PLACEMENT_3D ( 'NONE', #37260, #34791, #11308 ) ;
#7607 = CARTESIAN_POINT ( 'NONE',  ( 10.56230152254371824, -3.464101615137527457, -2.999999998771021748 ) ) ;
#7608 = CARTESIAN_POINT ( 'NONE',  ( -66.02752896937849414, 213.3500491399821613, 5.571401726697954970 ) ) ;
#7609 = CARTESIAN_POINT ( 'NONE',  ( -2.660918448318275509, 130.2976862821014379, 12.46528703574805874 ) ) ;
#7610 = CARTESIAN_POINT ( 'NONE',  ( 22.56230152254410370, 3.464101615137755275, -2.324999998771006826 ) ) ;
#7611 = ORIENTED_EDGE ( 'NONE', *, *, #34267, .F. ) ;
#7612 = AXIS2_PLACEMENT_3D ( 'NONE', #15047, #31914, #17523 ) ;
#7613 = CARTESIAN_POINT ( 'NONE',  ( 1.120210788295102201E-13, 195.0500000012290798, -27.00000000000000711 ) ) ;
#7614 = CARTESIAN_POINT ( 'NONE',  ( -50.22894823740646331, 235.3444610600932094, 5.000000000000000000 ) ) ;
#7615 = CARTESIAN_POINT ( 'NONE',  ( -0.1745138560725817967, 120.8101862821014691, 15.50000000000000533 ) ) ;
#7616 =( BOUNDED_CURVE ( )  B_SPLINE_CURVE ( 2, ( #1048, #12240, #9776, #35353, #862, #4087, #32513, #12621, #24185 ),
 .UNSPECIFIED., .F., .F. ) 
 B_SPLINE_CURVE_WITH_KNOTS ( ( 3, 2, 2, 2, 3 ),
 ( 0.5208333333333333703, 0.5277777777777777901, 0.5416666666666666297, 0.5555555555555555802, 0.5625000000000000000 ),
 .UNSPECIFIED. ) 
 CURVE ( )  GEOMETRIC_REPRESENTATION_ITEM ( )  RATIONAL_B_SPLINE_CURVE ( ( 0.9330127018922192983, 0.9330127018922198534, 1.000000000000000000, 0.8660254037844387076, 1.000000000000000000, 0.8660254037844387076, 1.000000000000000000, 0.9330127018922194093, 0.9330127018922194093 ) ) 
 REPRESENTATION_ITEM ( '' )  );
#7617 = CARTESIAN_POINT ( 'NONE',  ( 24.00000000000000000, -5.196152422706629359, -2.493749998770944387 ) ) ;
#7618 = CARTESIAN_POINT ( 'NONE',  ( 7.228626920339068285, 15.87268628210144961, -10.49813415415989581 ) ) ;
#7619 = CARTESIAN_POINT ( 'NONE',  ( 22.56230152254412857, -3.464101615137755275, -8.362500000000061107 ) ) ;
#7620 = ORIENTED_EDGE ( 'NONE', *, *, #29790, .T. ) ;
#7621 = DIRECTION ( 'NONE',  ( 0.000000000000000000, 0.000000000000000000, 1.000000000000000000 ) ) ;
#7622 = CARTESIAN_POINT ( 'NONE',  ( 8.843639120294328748, 90.33518628210144641, -3.474262827703334722 ) ) ;
#7623 =( LENGTH_UNIT ( ) NAMED_UNIT ( * ) SI_UNIT ( .MILLI., .METRE. ) );
#7624 = CARTESIAN_POINT ( 'NONE',  ( -3.796722387233185003, 127.8148137178985735, -8.710071997420207879 ) ) ;
#7625 = EDGE_CURVE ( 'NONE', #32085, #33186, #15648, .T. ) ;
#7626 = CARTESIAN_POINT ( 'NONE',  ( -1.926257025242585782E-15, 195.6406250006145058, -31.45816453501075927 ) ) ;
#7627 = CARTESIAN_POINT ( 'NONE',  ( 15.00000000000000000, 245.0499999999999829, 0.000000000000000000 ) ) ;
#7628 = CARTESIAN_POINT ( 'NONE',  ( 27.24356964375000345, 197.8343750006145569, -3.336375036156643733E-15 ) ) ;
#7629 = CARTESIAN_POINT ( 'NONE',  ( 11.70272374968897289, 194.9999999999999432, 24.61780419312783863 ) ) ;
#7630 = EDGE_CURVE ( 'NONE', #16688, #23609, #14103, .T. ) ;
#7631 = CARTESIAN_POINT ( 'NONE',  ( -8.843639120294245259, 53.06481371789855928, -3.474262827703533230 ) ) ;
#7632 = CARTESIAN_POINT ( 'NONE',  ( 0.000000000000000000, 210.0000000000000284, 0.000000000000000000 ) ) ;
#7633 = ORIENTED_EDGE ( 'NONE', *, *, #17453, .F. ) ;
#7634 = CARTESIAN_POINT ( 'NONE',  ( 26.99999999999999645, 241.6937500012290343, 3.464101615137751278 ) ) ;
#7635 = CARTESIAN_POINT ( 'NONE',  ( -2.660918448318005058, 63.70231371789855501, -12.46528703574811558 ) ) ;
#7636 = CARTESIAN_POINT ( 'NONE',  ( 10.31873187879410558, 0.000000000000000000, -6.496874999385504168 ) ) ;
#7637 = CARTESIAN_POINT ( 'NONE',  ( 13.62178482187499640, 197.4031250006145228, -23.59362340125807123 ) ) ;
#7638 = CARTESIAN_POINT ( 'NONE',  ( 15.24356964375000167, -3.323476615752272600, -6.515624999385480010 ) ) ;
#7639 = CARTESIAN_POINT ( 'NONE',  ( 0.1745138560722779009, 31.78981371789854649, 12.50000000000000355 ) ) ;
#7640 = EDGE_CURVE ( 'NONE', #22958, #37113, #5688, .T. ) ;
#7641 =( BOUNDED_CURVE ( )  B_SPLINE_CURVE ( 2, ( #21947, #4123, #27247, #18166, #33122, #33311, #26867 ),
 .UNSPECIFIED., .F., .F. ) 
 B_SPLINE_CURVE_WITH_KNOTS ( ( 3, 2, 2, 3 ),
 ( 0.7173913043478248319, 0.7246376811594200662, 0.7318840579710154115, 0.7391304347826105348 ),
 .UNSPECIFIED. ) 
 CURVE ( )  GEOMETRIC_REPRESENTATION_ITEM ( )  RATIONAL_B_SPLINE_CURVE ( ( 1.000000000000022649, 0.8660254037844161701, 1.000000000000000000, 0.8660254037844387076, 1.000000000000000000, 0.8660254037844038466, 1.000000000000034861 ) ) 
 REPRESENTATION_ITEM ( '' )  );
#7642 = ORIENTED_EDGE ( 'NONE', *, *, #35638, .T. ) ;
#7643 = CARTESIAN_POINT ( 'NONE',  ( 33.99951059573448475, -5.196152422706629359, 164.1639462825446003 ) ) ;
#7644 = DIRECTION ( 'NONE',  ( 1.000000000000000000, 0.000000000000000000, 0.000000000000000000 ) ) ;
#7645 = CARTESIAN_POINT ( 'NONE',  ( 25.14654753852813229, -3.604726614523244610, 169.0321829630285322 ) ) ;
#7646 = CARTESIAN_POINT ( 'NONE',  ( -49.00669563604516554, 209.8844732041982013, -6.500000000000000888 ) ) ;
#7647 = VECTOR ( 'NONE', #34495, 1000.000000000000000 ) ;
#7648 = CARTESIAN_POINT ( 'NONE',  ( -6.000000000000000888, -30.00000000000000000, -19.99999999999999289 ) ) ;
#7649 = CARTESIAN_POINT ( 'NONE',  ( 6.932735513424201024, 64.85231371789855359, -10.69584247140429412 ) ) ;
#7650 = CARTESIAN_POINT ( 'NONE',  ( -36.94122103062156981, 208.9097554298617752, -4.530955311639240257 ) ) ;
#7651 = CARTESIAN_POINT ( 'NONE',  ( -54.95163769728823411, 215.6869285224996986, -3.149950860017881382 ) ) ;
#7652 = DIRECTION ( 'NONE',  ( -1.000000000000000000, 0.000000000000000000, 0.000000000000000000 ) ) ;
#7653 = CYLINDRICAL_SURFACE ( 'NONE', #4660, 5.999999999999998224 ) ;
#7654 = CARTESIAN_POINT ( 'NONE',  ( 8.927990412390371944, 30.92731371789853867, 13.04141134922778811 ) ) ;
#7655 = CARTESIAN_POINT ( 'NONE',  ( -34.55877896937850124, 212.1620413398627534, -8.530955311639255356 ) ) ;
#7656 = CARTESIAN_POINT ( 'NONE',  ( 4.944772684328679446, 33.98518628210143788, -11.48171059495397373 ) ) ;
#7657 = DIRECTION ( 'NONE',  ( -1.000000000000000000, -6.123233995736766036E-17, -0.000000000000000000 ) ) ;
#7658 = CARTESIAN_POINT ( 'NONE',  ( -2.311890736173176641, 69.92268628210146630, -12.53471296425194836 ) ) ;
#7659 = CARTESIAN_POINT ( 'NONE',  ( 5.770363421893814682, 9.835186282101449962, 14.38691631536207183 ) ) ;
#7660 = AXIS2_PLACEMENT_3D ( 'NONE', #18457, #19723, #2259 ) ;
#7661 = CARTESIAN_POINT ( 'NONE',  ( 13.56230152254410903, 5.196152422706636465, -2.325000000000049027 ) ) ;
#7662 = CARTESIAN_POINT ( 'NONE',  ( -27.95091016768448000, 207.9223924231847604, -7.730003002181515370 ) ) ;
#7663 = ORIENTED_EDGE ( 'NONE', *, *, #24850, .T. ) ;
#7664 = CARTESIAN_POINT ( 'NONE',  ( -14.25334919248782306, 31.68518628210144428, -6.092822981423979378 ) ) ;
#7665 = CARTESIAN_POINT ( 'NONE',  ( 27.24356964374999279, 195.1156250006145285, -15.72908226750539207 ) ) ;
#7666 = CARTESIAN_POINT ( 'NONE',  ( -27.24356964375000345, 198.0593750006145513, 0.000000000000000000 ) ) ;
#7667 = DIRECTION ( 'NONE',  ( 1.000000000000000000, 0.000000000000000000, 0.000000000000000000 ) ) ;
#7668 = CARTESIAN_POINT ( 'NONE',  ( 33.63672481644027812, -5.196152422706635576, 160.0172858505133604 ) ) ;
#7669 = FACE_OUTER_BOUND ( 'NONE', #23163, .T. ) ;
#7670 = CARTESIAN_POINT ( 'NONE',  ( 15.00000000000000178, 247.7874999999999943, 3.464101615137757051 ) ) ;
#7671 = CARTESIAN_POINT ( 'NONE',  ( 21.00000000000000000, 246.5968750006145456, -6.646953231504538984 ) ) ;
#7672 = CARTESIAN_POINT ( 'NONE',  ( -8.843639120294245259, 108.2648137178985621, -3.474262827703533230 ) ) ;
#7673 = CARTESIAN_POINT ( 'NONE',  ( 18.12178482187500350, 244.5343750006145456, 4.985214923628407568 ) ) ;
#7674 = EDGE_LOOP ( 'NONE', ( #5556, #35476, #7550, #17939 ) ) ;
#7675 = CARTESIAN_POINT ( 'NONE',  ( 26.99999999999999645, 249.3812500012290343, -7.347880794884117764E-16 ) ) ;
#7676 = CARTESIAN_POINT ( 'NONE',  ( -4.622313124798826500, 124.3648137178985706, 11.61527771782809637 ) ) ;
#7677 = CARTESIAN_POINT ( 'NONE',  ( 22.80587116629410716, 3.604726614523238837, -8.878124999385544669 ) ) ;
#7678 = CARTESIAN_POINT ( 'NONE',  ( 30.98559686366965238, -7.209453229046475009, 164.1358944260424835 ) ) ;
#7679 = CARTESIAN_POINT ( 'NONE',  ( 15.24356964374999990, 0.000000000000000000, -0.7031249993854904456 ) ) ;
#7680 = CARTESIAN_POINT ( 'NONE',  ( -27.00000000000000355, 198.6125000000000398, -15.58845726811989429 ) ) ;
#7681 = ORIENTED_EDGE ( 'NONE', *, *, #25380, .F. ) ;
#7682 = CARTESIAN_POINT ( 'NONE',  ( -7.228626920339070061, 38.87268628210144072, 10.49813415415989404 ) ) ;
#7683 = ORIENTED_EDGE ( 'NONE', *, *, #10580, .T. ) ;
#7684 = ORIENTED_EDGE ( 'NONE', *, *, #25354, .T. ) ;
#7685 = CARTESIAN_POINT ( 'NONE',  ( 26.99999999999999645, 3.464101615137755275, -5.531249998770956466 ) ) ;
#7686 = CARTESIAN_POINT ( 'NONE',  ( 20.99999999999999645, 6.646953231504538984, -0.7031249993854685743 ) ) ;
#7687 = CARTESIAN_POINT ( 'NONE',  ( 20.99999999999999289, 241.8437500012290400, -5.999999999999997335 ) ) ;
#7688 = CARTESIAN_POINT ( 'NONE',  ( 23.87821517812499650, 249.1468750006145285, -4.985214923628404904 ) ) ;
#7689 = CARTESIAN_POINT ( 'NONE',  ( -11.48171059495397373, 68.48518628210145209, -4.944772684328680334 ) ) ;
#7690 = CARTESIAN_POINT ( 'NONE',  ( 11.08355503943142750, 135.7601862821014720, -10.83675517735155225 ) ) ;
#7691 = CARTESIAN_POINT ( 'NONE',  ( -61.47544563604515844, 214.8429017333602360, 4.673758765035156415 ) ) ;
#7692 = CARTESIAN_POINT ( 'NONE',  ( 5.025722718613374163, 215.9903539805198420, -0.3926987779611901819 ) ) ;
#7693 = CARTESIAN_POINT ( 'NONE',  ( -53.55877896937850124, 211.0902445701383101, -4.530955311639234040 ) ) ;
#7694 = CARTESIAN_POINT ( 'NONE',  ( 36.78872592836736288, 7.347880794884125653E-16, 161.6236836811924604 ) ) ;
#7695 = AXIS2_PLACEMENT_3D ( 'NONE', #15820, #33431, #19051 ) ;
#7696 = CARTESIAN_POINT ( 'NONE',  ( 25.09912511996950713, 0.000000000000000000, 165.6954939908422944 ) ) ;
#7697 = CARTESIAN_POINT ( 'NONE',  ( -11.61527771782809282, 126.6648137178985678, -4.622313124798832717 ) ) ;
#7698 = CARTESIAN_POINT ( 'NONE',  ( -68.40997103062156270, 213.8393509191290889, 2.350049139982164359 ) ) ;
#7699 = CARTESIAN_POINT ( 'NONE',  ( -59.70163769728823411, 217.4189793300686233, -4.149950860017907139 ) ) ;
#7700 = CARTESIAN_POINT ( 'NONE',  ( 15.24356964375000167, -3.323476615752272600, -2.465624999385486849 ) ) ;
#7701 = CARTESIAN_POINT ( 'NONE',  ( -13.62178482187498396, 196.7281250006145399, 23.59362340125808188 ) ) ;
#7702 = CARTESIAN_POINT ( 'NONE',  ( 8.632099005475788900, 101.6523137178985792, -13.23911966647199812 ) ) ;
#7703 = CARTESIAN_POINT ( 'NONE',  ( -47.42336230271183695, 215.6869285224997270, 3.149950860017831200 ) ) ;
#7704 = VECTOR ( 'NONE', #16006, 1000.000000000000000 ) ;
#7705 = VERTEX_POINT ( 'NONE', #5930 ) ;
#7706 = CARTESIAN_POINT ( 'NONE',  ( 27.74126513682283601, -5.196152422706632912, 161.4741528376846134 ) ) ;
#7707 = CARTESIAN_POINT ( 'NONE',  ( 7.228626920339068285, 117.0726862821014720, -10.49813415415989581 ) ) ;
#7708 = CARTESIAN_POINT ( 'NONE',  ( 6.092822981423978490, 61.58518628210146062, -14.25334919248782306 ) ) ;
#7709 = DIRECTION ( 'NONE',  ( 0.08715574274765150453, 0.000000000000000000, 0.9961946980917461003 ) ) ;
#7710 = CARTESIAN_POINT ( 'NONE',  ( 37.17109026623309376, 7.646167579472024665E-16, 163.1994798139711520 ) ) ;
#7711 = CARTESIAN_POINT ( 'NONE',  ( -0.1745138560725817967, 93.21018628210146062, 15.50000000000000533 ) ) ;
#7712 = CARTESIAN_POINT ( 'NONE',  ( -58.31622103062156270, 211.6261429550005744, 6.530955311639228711 ) ) ;
#7713 = CARTESIAN_POINT ( 'NONE',  ( 10.31873187879411446, 3.604726614523236616, -6.928124999385510741 ) ) ;
#7714 = CARTESIAN_POINT ( 'NONE',  ( -9.500000000000005329, 31.11018628210143433, -0.1745138560725176813 ) ) ;
#7715 = CARTESIAN_POINT ( 'NONE',  ( 19.39230484541326760, 246.4924038105676516, 5.999999999999999112 ) ) ;
#7716 = CARTESIAN_POINT ( 'NONE',  ( -60.29538769728823411, 211.8571965466039444, -6.469044688360768625 ) ) ;
#7717 = CARTESIAN_POINT ( 'NONE',  ( 15.00000000000000000, 243.2687500012290513, -3.464101615137752610 ) ) ;
#7718 = CARTESIAN_POINT ( 'NONE',  ( 11.61527771782819940, 62.73518628210145209, -4.622313124798573369 ) ) ;
#7719 = CARTESIAN_POINT ( 'NONE',  ( 5.727106289114498080E-15, 198.3125000000000000, 31.17691453623979214 ) ) ;
#7720 = CARTESIAN_POINT ( 'NONE',  ( 22.56230152254332921, 3.464101615138219348, -6.937500000000038192 ) ) ;
#7722 = CARTESIAN_POINT ( 'NONE',  ( 16.56230152254411436, -7.209453229046482114, -1.434374999385489735 ) ) ;
#7721 = CARTESIAN_POINT ( 'NONE',  ( 0.1745138560725194299, 33.41018628210144925, -9.500000000000005329 ) ) ;
#7723 = CARTESIAN_POINT ( 'NONE',  ( 20.99999999999999645, -6.928203230275506996, -6.131249998770972098 ) ) ;
#7724 = ORIENTED_EDGE ( 'NONE', *, *, #17525, .F. ) ;
#7725 = CARTESIAN_POINT ( 'NONE',  ( 26.99999999999999645, 7.347880794884117764E-16, -2.475000000000004974 ) ) ;
#7726 = DIRECTION ( 'NONE',  ( -1.000000000000000000, -4.130293990420971855E-17, 0.000000000000000000 ) ) ;
#7727 = CARTESIAN_POINT ( 'NONE',  ( 33.91084112185822619, 5.407089921784862696, 161.7531254346117464 ) ) ;
#7728 = CARTESIAN_POINT ( 'NONE',  ( 27.75760683848089982, 5.196152422706636465, 161.6609393423525205 ) ) ;
#7729 = CARTESIAN_POINT ( 'NONE',  ( 24.00000000000000000, 242.9499999999999886, 5.196152422706629359 ) ) ;
#7730 = DIRECTION ( 'NONE',  ( 0.08715574274765150453, 0.000000000000000000, 0.9961946980917461003 ) ) ;
#7731 = CARTESIAN_POINT ( 'NONE',  ( 8.715434833792128799, 83.53981371789856780, -8.962234695871567070 ) ) ;
#7732 = CARTESIAN_POINT ( 'NONE',  ( -11.61527771782819940, 85.73518628210143788, 4.622313124798574258 ) ) ;
#7733 = ORIENTED_EDGE ( 'NONE', *, *, #20597, .F. ) ;
#7734 = ORIENTED_EDGE ( 'NONE', *, *, #37267, .F. ) ;
#7735 = CARTESIAN_POINT ( 'NONE',  ( 26.99999999999999645, 198.1250000012290400, -15.58845726811990495 ) ) ;
#7736 = CARTESIAN_POINT ( 'NONE',  ( 15.00000000000008171, -3.464101615137802348, -4.012499999999994849 ) ) ;
#7737 = CARTESIAN_POINT ( 'NONE',  ( 15.50000000000000533, 57.08981371789855075, -0.1745138560722452326 ) ) ;
#7738 = CARTESIAN_POINT ( 'NONE',  ( 21.00000000000000000, 6.646953231504538984, -9.365624999385474325 ) ) ;
#7739 = CARTESIAN_POINT ( 'NONE',  ( 21.00000000000000000, 243.8968750006145001, -6.646953231504538984 ) ) ;
#7740 = CARTESIAN_POINT ( 'NONE',  ( -61.68080436395489841, 205.4999999999999716, -0.1155267958017894420 ) ) ;
#7741 = CARTESIAN_POINT ( 'NONE',  ( 34.43419986258128773, 5.196152422706637353, 169.1324673380528623 ) ) ;
#7742 = CARTESIAN_POINT ( 'NONE',  ( 7.954856959092311719, 47.02731371789855075, -5.529263428287300108 ) ) ;
#7743 = CARTESIAN_POINT ( 'NONE',  ( 19.68408634441910721, -5.407089921784855591, -6.740624999385547156 ) ) ;
#7744 = EDGE_CURVE ( 'NONE', #9886, #19776, #29044, .T. ) ;
#7745 = CARTESIAN_POINT ( 'NONE',  ( -6.840914352311947333, 99.63981371789857633, -6.594114490232462877 ) ) ;
#7746 = CARTESIAN_POINT ( 'NONE',  ( 5.778771075727756162E-15, 199.5218750006145854, 31.45816453501075927 ) ) ;
#7747 = CARTESIAN_POINT ( 'NONE',  ( -8.962234695871565293, 7.639813717898541690, -8.715434833792128799 ) ) ;
#7748 = CARTESIAN_POINT ( 'NONE',  ( 11.61527771782819940, 62.73518628210145209, -4.622313124798573369 ) ) ;
#7749 = CARTESIAN_POINT ( 'NONE',  ( 10.56230152254411436, -3.464101615137757051, -9.299999998770987375 ) ) ;
#7750 = ADVANCED_FACE ( 'NONE', ( #11440 ), #14657, .T. ) ;
#7751 = CARTESIAN_POINT ( 'NONE',  ( 0.000000000000000000, 143.0000000000000000, 0.000000000000000000 ) ) ;
#7752 = CARTESIAN_POINT ( 'NONE',  ( 27.71554269823568362, -5.407089921784859143, 162.5774681431477404 ) ) ;
#7753 = CARTESIAN_POINT ( 'NONE',  ( -12.50000000000000355, 141.5101862821014720, -0.1745138560725508214 ) ) ;
#7754 = CARTESIAN_POINT ( 'NONE',  ( 16.56230152254411436, -7.209453229046482114, -5.484374999385515537 ) ) ;
#7755 = CARTESIAN_POINT ( 'NONE',  ( 19.56230152254412502, -5.196152422706635576, -1.650000000000068079 ) ) ;
#7756 = VECTOR ( 'NONE', #11649, 1000.000000000000000 ) ;
#7757 = FACE_OUTER_BOUND ( 'NONE', #22189, .T. ) ;
#7758 = CARTESIAN_POINT ( 'NONE',  ( 0.1745138560725194299, 97.81018628210145494, -9.500000000000005329 ) ) ;
#7759 = CYLINDRICAL_SURFACE ( 'NONE', #14640, 6.000000000000001776 ) ;
#7760 = EDGE_CURVE ( 'NONE', #14209, #3896, #848, .T. ) ;
#7761 = CARTESIAN_POINT ( 'NONE',  ( -2.660918448318275509, 111.8976862821014606, 12.46528703574805874 ) ) ;
#7762 = CARTESIAN_POINT ( 'NONE',  ( -7.433878009488998906, 142.9999999999999716, 9.066021292333855897 ) ) ;
#7763 = CARTESIAN_POINT ( 'NONE',  ( 15.00000000000000000, 0.000000000000000000, -0.3937499987709536242 ) ) ;
#7764 = ORIENTED_EDGE ( 'NONE', *, *, #35157, .T. ) ;
#7765 = CARTESIAN_POINT ( 'NONE',  ( 24.71676078210377625, 0.000000000000000000, 164.1196978580636028 ) ) ;
#7766 = AXIS2_PLACEMENT_3D ( 'NONE', #31079, #4912, #36933 ) ;
#7767 = CARTESIAN_POINT ( 'NONE',  ( 26.75643035624999655, 3.323476615752271712, -5.728124999385479477 ) ) ;
#7768 = EDGE_CURVE ( 'NONE', #762, #9915, #37023, .T. ) ;
#7769 = CARTESIAN_POINT ( 'NONE',  ( -27.24356964375000345, 198.5093750006145399, 0.000000000000000000 ) ) ;
#7770 = CARTESIAN_POINT ( 'NONE',  ( 17.59114475875851014, 4.706365066813837039, -7.999999999999998224 ) ) ;
#7771 = FACE_OUTER_BOUND ( 'NONE', #23621, .T. ) ;
#7772 = FACE_OUTER_BOUND ( 'NONE', #770, .T. ) ;
#7773 = CARTESIAN_POINT ( 'NONE',  ( 23.87821517812500005, 241.0093750006145399, 4.985214923628404016 ) ) ;
#7774 = CARTESIAN_POINT ( 'NONE',  ( -77.00000000000002842, 210.0000000000000000, -5.000000000000001776 ) ) ;
#7775 = CARTESIAN_POINT ( 'NONE',  ( 10.49813415416005213, 139.0273137178985507, -7.228626920338837358 ) ) ;
#7776 = CARTESIAN_POINT ( 'NONE',  ( 13.62178482187499640, 195.2093750006145569, -23.59362340125807123 ) ) ;
#7778 = ORIENTED_EDGE ( 'NONE', *, *, #32767, .F. ) ;
#7777 = EDGE_LOOP ( 'NONE', ( #911, #8927, #21930, #4269 ) ) ;
#7779 = CARTESIAN_POINT ( 'NONE',  ( 26.75643035624999655, 244.9843750006145058, 3.323476615752267715 ) ) ;
#7780 = CARTESIAN_POINT ( 'NONE',  ( -7.228626920338836470, 7.927313717898537782, -10.49813415416005213 ) ) ;
#7781 = CARTESIAN_POINT ( 'NONE',  ( 26.75643035624999655, -3.323476615752267715, -3.553124999385494753 ) ) ;
#7782 = CARTESIAN_POINT ( 'NONE',  ( 8.927990412390371944, 113.7273137178985678, 13.04141134922778811 ) ) ;
#7783 = CYLINDRICAL_SURFACE ( 'NONE', #11933, 27.00000000000000355 ) ;
#7784 = CARTESIAN_POINT ( 'NONE',  ( 26.75643035624999655, -3.323476615752267715, -2.315624999385466509 ) ) ;
#7785 = AXIS2_PLACEMENT_3D ( 'NONE', #21330, #12780, #30219 ) ;
#7786 = CARTESIAN_POINT ( 'NONE',  ( 22.80587116629411781, 3.604726614523243278, -8.034374999385502036 ) ) ;
#7787 = VERTEX_POINT ( 'NONE', #25840 ) ;
#7788 = CARTESIAN_POINT ( 'NONE',  ( 26.99999999999999645, 198.1250000012290400, -15.58845726811990495 ) ) ;
#7789 = CARTESIAN_POINT ( 'NONE',  ( -11.61527771782819940, 113.3351862821014606, 4.622313124798574258 ) ) ;
#7790 = CARTESIAN_POINT ( 'NONE',  ( 16.56230152254411436, -7.209453229046475009, -1.378124999385542226 ) ) ;
#7791 = CARTESIAN_POINT ( 'NONE',  ( -47.22544563604517265, 216.3070033484980854, 6.137860380172893926 ) ) ;
#7792 = CARTESIAN_POINT ( 'NONE',  ( 23.87821517812500005, 245.3968750006145285, 4.985214923628404016 ) ) ;
#7793 = CARTESIAN_POINT ( 'NONE',  ( 22.56230152254429555, 3.464101615137640255, -2.774999998771005227 ) ) ;
#7794 = EDGE_CURVE ( 'NONE', #17216, #5013, #27491, .T. ) ;
#7795 = CARTESIAN_POINT ( 'NONE',  ( -34.36086230271182984, 212.1499508600178387, -3.954877714930852495 ) ) ;
#7796 = CARTESIAN_POINT ( 'NONE',  ( 8.962234695871762469, 117.3601862821014521, -8.715434833791931624 ) ) ;
#7797 = CARTESIAN_POINT ( 'NONE',  ( 16.56230152254411436, 6.928203230275506996, -1.349999998771021614 ) ) ;
#7798 = EDGE_LOOP ( 'NONE', ( #24788, #3254, #29673, #18802, #27135 ) ) ;
#7799 = EDGE_CURVE ( 'NONE', #35303, #34054, #19538, .T. ) ;
#7800 = CARTESIAN_POINT ( 'NONE',  ( -38.12872103062154849, 203.4690446883607535, 1.626142955000567936 ) ) ;
#7801 = CARTESIAN_POINT ( 'NONE',  ( -13.49999999999998401, 195.2375000012290229, 23.38268590217985476 ) ) ;
#7802 = CARTESIAN_POINT ( 'NONE',  ( 15.00000000000000000, 244.5625000000000000, -3.464101615137752610 ) ) ;
#7803 = CARTESIAN_POINT ( 'NONE',  ( 15.53471296425195369, 118.2226862821014493, -2.908627838312120684 ) ) ;
#7804 = EDGE_CURVE ( 'NONE', #11542, #28877, #6451, .T. ) ;
#7805 = DIRECTION ( 'NONE',  ( -1.000000000000000000, 0.000000000000000000, 0.000000000000000000 ) ) ;
#7806 = CARTESIAN_POINT ( 'NONE',  ( -9.500000000000005329, 141.5101862821014720, -0.1745138560725176813 ) ) ;
#7807 = CARTESIAN_POINT ( 'NONE',  ( 19.56230152254411792, 5.196152422706637353, -8.700000000000041922 ) ) ;
#7808 = VERTEX_POINT ( 'NONE', #1729 ) ;
#7809 = CARTESIAN_POINT ( 'NONE',  ( 10.56230152254410726, 0.000000000000000000, -3.600000000000047606 ) ) ;
#7810 = CARTESIAN_POINT ( 'NONE',  ( 6.840914352312096547, 89.76018628210145778, -6.594114490232313663 ) ) ;
#7811 = CARTESIAN_POINT ( 'NONE',  ( 38.04237167757703020, 114.1383727779938511, 0.5000000000000000000 ) ) ;
#7812 = CARTESIAN_POINT ( 'NONE',  ( 6.594114490232462877, 129.5398137178985678, -6.840914352311949109 ) ) ;
#7813 = CARTESIAN_POINT ( 'NONE',  ( -27.24356964374999635, 195.3406250006145513, 15.72908226750539384 ) ) ;
#7814 = CARTESIAN_POINT ( 'NONE',  ( 19.39230484541324984, 245.1424038105676857, 5.999999999999991118 ) ) ;
#7815 = CARTESIAN_POINT ( 'NONE',  ( 27.24356964375000700, 197.3468750006145740, 15.72908226750537075 ) ) ;
#7816 = CARTESIAN_POINT ( 'NONE',  ( -1.045839947578415010E-13, 195.1625000000000512, 27.00000000000000355 ) ) ;
#7817 = CARTESIAN_POINT ( 'NONE',  ( -9.534712964251895073, 52.77731371789855785, -1.715153634034446428 ) ) ;
#7818 = CARTESIAN_POINT ( 'NONE',  ( 21.00000000000000000, -6.928203230275506996, -9.787500000000010303 ) ) ;
#7819 = EDGE_LOOP ( 'NONE', ( #4410, #254 ) ) ;
#7820 = CARTESIAN_POINT ( 'NONE',  ( 15.00000000000000178, 242.4437500012290343, 3.464101615137757051 ) ) ;
#7821 = CARTESIAN_POINT ( 'NONE',  ( -8.962234695871565293, 62.83981371789855785, -8.715434833792128799 ) ) ;
#7822 = CARTESIAN_POINT ( 'NONE',  ( 22.80587116629411781, 7.646167579472024665E-16, -5.821874999385522997 ) ) ;
#7823 = CARTESIAN_POINT ( 'NONE',  ( 13.62178482187501416, 199.0531250006145285, 23.59362340125806767 ) ) ;
#7824 = CARTESIAN_POINT ( 'NONE',  ( 26.75643035624999655, 3.323476615752271712, -6.290624999385498128 ) ) ;
#7825 = CARTESIAN_POINT ( 'NONE',  ( 12.50000000000000355, 38.68981371789855217, -0.1745138560722771515 ) ) ;
#7826 = ORIENTED_EDGE ( 'NONE', *, *, #30917, .T. ) ;
#7827 = UNCERTAINTY_MEASURE_WITH_UNIT (LENGTH_MEASURE( 1.000000000000000082E-05 ), #25280, 'distance_accuracy_value', 'NONE');
#7828 = CARTESIAN_POINT ( 'NONE',  ( 22.80587116629412492, -3.604726614523238837, -2.259374999385487470 ) ) ;
#7829 = CARTESIAN_POINT ( 'NONE',  ( -81.00000000000002842, 214.0000000000000000, -2.499999999999998668 ) ) ;
#7830 = CARTESIAN_POINT ( 'NONE',  ( 10.56230152254581078, 3.464101615138732715, -9.374999998771002652 ) ) ;
#7831 = CARTESIAN_POINT ( 'NONE',  ( -48.01711230271182274, 216.4690446883607535, -1.857196546604089393 ) ) ;
#7832 = DIRECTION ( 'NONE',  ( 0.000000000000000000, 0.000000000000000000, 1.000000000000000000 ) ) ;
#7833 = CARTESIAN_POINT ( 'NONE',  ( 0.1745138560722779009, 59.38981371789856212, 12.50000000000000355 ) ) ;
#7834 = EDGE_CURVE ( 'NONE', #1338, #33602, #6901, .T. ) ;
#7835 = CARTESIAN_POINT ( 'NONE',  ( -37.53497103062155560, 206.1606490808709111, -2.350049139982163027 ) ) ;
#7836 =( BOUNDED_CURVE ( )  B_SPLINE_CURVE ( 2, ( #13330, #19225, #22056, #24888, #4974, #27914, #25072 ),
 .UNSPECIFIED., .F., .F. ) 
 B_SPLINE_CURVE_WITH_KNOTS ( ( 3, 2, 2, 3 ),
 ( 0.9130434782608684019, 0.9202898550724627480, 0.9275362318840569831, 0.9347826086956513292 ),
 .UNSPECIFIED. ) 
 CURVE ( )  GEOMETRIC_REPRESENTATION_ITEM ( )  RATIONAL_B_SPLINE_CURVE ( ( 1.000000000000020428, 0.8660254037844181685, 1.000000000000000000, 0.8660254037844387076, 1.000000000000000000, 0.8660254037844551389, 0.9999999999999835687 ) ) 
 REPRESENTATION_ITEM ( '' )  );
#7837 = CARTESIAN_POINT ( 'NONE',  ( -54.35788769728821279, 216.4690446883607535, 1.857196546604031662 ) ) ;
#7838 = DIRECTION ( 'NONE',  ( 1.000000000000000000, 0.000000000000000000, 0.000000000000000000 ) ) ;
#7839 = CARTESIAN_POINT ( 'NONE',  ( -81.00000000000002842, 214.0000000000000000, -2.499999999999998668 ) ) ;
#7840 = CARTESIAN_POINT ( 'NONE',  ( -13.04141134922778456, 42.42731371789855643, 8.927990412390377273 ) ) ;
#7841 = CARTESIAN_POINT ( 'NONE',  ( -37.32961230271184405, 212.3930949314663792, 8.469044688360751749 ) ) ;
#7842 = CARTESIAN_POINT ( 'NONE',  ( 2.660918448318279950, 33.69768628210145067, -12.46528703574805697 ) ) ;
#7843 = CARTESIAN_POINT ( 'NONE',  ( 30.93902301358532014, 6.928203230275514990, 163.6035528836375477 ) ) ;
#7844 = CARTESIAN_POINT ( 'NONE',  ( 11.48171059495397728, 73.08518628210144641, 4.944772684328674117 ) ) ;
#7845 = CARTESIAN_POINT ( 'NONE',  ( -8.927990412390661490, 11.27268628210142865, 13.04141134922759804 ) ) ;
#7846 = CARTESIAN_POINT ( 'NONE',  ( 19.56230152254411792, 5.196152422706637353, -2.850000000000019185 ) ) ;
#7847 = CARTESIAN_POINT ( 'NONE',  ( 19.39230484541326049, 244.1138461906614054, -5.999999999999997335 ) ) ;
#7848 = ORIENTED_EDGE ( 'NONE', *, *, #15755, .T. ) ;
#7849 = CARTESIAN_POINT ( 'NONE',  ( 10.83675517735155225, 27.66018628210143859, 11.08355503943142573 ) ) ;
#7850 = CARTESIAN_POINT ( 'NONE',  ( 5.778771075727756162E-15, 195.8656250006145285, 31.45816453501076637 ) ) ;
#7851 = CARTESIAN_POINT ( 'NONE',  ( -1.926257025242585782E-15, 199.2968750006145342, -31.45816453501075927 ) ) ;
#7852 = CARTESIAN_POINT ( 'NONE',  ( 25.12854018303972126, 0.000000000000000000, 166.0317097002238995 ) ) ;
#7853 = CARTESIAN_POINT ( 'NONE',  ( 30.64487238181199658, -6.928203230275514990, 160.2413957775779068 ) ) ;
#7854 = DIRECTION ( 'NONE',  ( -0.000000000000000000, 1.000000000000000000, -0.000000000000000000 ) ) ;
#7855 = CARTESIAN_POINT ( 'NONE',  ( -4.622313124798576922, 5.235186282101428112, -11.61527771782819762 ) ) ;
#7856 =( BOUNDED_CURVE ( )  B_SPLINE_CURVE ( 2, ( #4081, #15653, #15273, #9955, #1608, #23996, #35725 ),
 .UNSPECIFIED., .F., .F. ) 
 B_SPLINE_CURVE_WITH_KNOTS ( ( 3, 2, 2, 3 ),
 ( 0.1956521739130460125, 0.2028985507246403308, 0.2101449275362346492, 0.2173913043478289675 ),
 .UNSPECIFIED. ) 
 CURVE ( )  GEOMETRIC_REPRESENTATION_ITEM ( )  RATIONAL_B_SPLINE_CURVE ( ( 0.9999999999999533706, 0.8660254037844854480, 1.000000000000000000, 0.8660254037844387076, 1.000000000000000000, 0.8660254037843853059, 1.000000000000053291 ) ) 
 REPRESENTATION_ITEM ( '' )  );
#7857 = CARTESIAN_POINT ( 'NONE',  ( 23.87821517812500005, 248.2093750006145285, 4.985214923628404016 ) ) ;
#7858 = CARTESIAN_POINT ( 'NONE',  ( 9.465287035748106703, 112.0023137178985451, -2.064181346179063237 ) ) ;
#7859 = CARTESIAN_POINT ( 'NONE',  ( 18.12178482187500350, 240.9343750006145513, 4.985214923628407568 ) ) ;
#7860 = VERTEX_POINT ( 'NONE', #25593 ) ;
#7861 = LINE ( 'NONE', #30983, #27840 ) ;
#7862 = CARTESIAN_POINT ( 'NONE',  ( 18.00000000000000000, 248.6312500012290343, -5.196152422706630247 ) ) ;
#7863 = CARTESIAN_POINT ( 'NONE',  ( 11.61527771782809637, 122.0648137178985735, 4.622313124798827388 ) ) ;
#7864 = CARTESIAN_POINT ( 'NONE',  ( 10.31873187879410914, 0.000000000000000000, -8.240624999385548932 ) ) ;
#7865 = CARTESIAN_POINT ( 'NONE',  ( 27.78090950529641745, 5.407089921784856479, 163.3246141667165716 ) ) ;
#7866 = CARTESIAN_POINT ( 'NONE',  ( -70.65404437008254490, 216.5466800865261234, 7.500000000000000000 ) ) ;
#7867 = CARTESIAN_POINT ( 'NONE',  ( 5.727106289114498080E-15, 196.9625000000000057, 31.17691453623979214 ) ) ;
#7868 = VERTEX_POINT ( 'NONE', #4574 ) ;
#7869 = CARTESIAN_POINT ( 'NONE',  ( -2.311890736173176641, 33.12268628210144072, -12.53471296425194659 ) ) ;
#7870 = EDGE_LOOP ( 'NONE', ( #17169, #11442, #33548, #35305, #29193, #8556, #27146 ) ) ;
#7871 = VECTOR ( 'NONE', #7944, 1000.000000000000000 ) ;
#7872 = VERTEX_POINT ( 'NONE', #1912 ) ;
#7873 = CARTESIAN_POINT ( 'NONE',  ( 24.00000000000000000, -5.196152422706629359, -4.743749998770946164 ) ) ;
#7874 = CARTESIAN_POINT ( 'NONE',  ( 26.75643035624999655, -3.323476615752267271, -2.203124999385475569 ) ) ;
#7875 = CARTESIAN_POINT ( 'NONE',  ( 22.56230152254412147, 7.347880794884125653E-16, -4.275000000000028777 ) ) ;
#7876 = CARTESIAN_POINT ( 'NONE',  ( 15.24356964375000167, 248.4343750006145228, 3.323476615752272600 ) ) ;
#7877 = CARTESIAN_POINT ( 'NONE',  ( 12.50000000000000355, 63.31018628210144072, 0.1745138560725507937 ) ) ;
#7878 = ADVANCED_FACE ( 'NONE', ( #19378 ), #5128, .F. ) ;
#7879 = CARTESIAN_POINT ( 'NONE',  ( -64.44419563604516554, 203.5000000000000000, 0.1155267958017914542 ) ) ;
#7880 = CARTESIAN_POINT ( 'NONE',  ( 15.00964601948014021, 225.9742772813838769, 0.3926987779608852036 ) ) ;
#7881 = CARTESIAN_POINT ( 'NONE',  ( -51.38169563604516554, 210.1155267958017703, 4.499999999999996447 ) ) ;
#7882 = VECTOR ( 'NONE', #31668, 1000.000000000000114 ) ;
#7883 = CARTESIAN_POINT ( 'NONE',  ( 30.96843807686976291, -6.928203230275506996, 163.9397685954678536 ) ) ;
#7884 = CARTESIAN_POINT ( 'NONE',  ( -2.311890736173448424, 114.8773137178985735, 12.53471296425189330 ) ) ;
#7885 = CARTESIAN_POINT ( 'NONE',  ( -66.62872103062156270, 205.4690446883607535, 1.090244570138264368 ) ) ;
#7886 = MANIFOLD_SOLID_BREP ( 'Cavity1', #13224 ) ;
#7888 = EDGE_CURVE ( 'NONE', #28581, #14336, #16520, .T. ) ;
#7887 = CARTESIAN_POINT ( 'NONE',  ( -60.09747103062157692, 214.3500491399821044, -7.303452534266878793 ) ) ;
#7889 = CARTESIAN_POINT ( 'NONE',  ( 15.24356964375000167, -3.323476615752272600, -1.115624999385467442 ) ) ;
#7890 = CARTESIAN_POINT ( 'NONE',  ( 13.62178482187499640, 196.0531250006145285, -23.59362340125807123 ) ) ;
#7891 = CARTESIAN_POINT ( 'NONE',  ( -2.908627838312453306, 96.47731371789852517, 15.53471296425188797 ) ) ;
#7892 = CARTESIAN_POINT ( 'NONE',  ( -67.41294563604516554, 216.1378603801729241, -6.307003348498026796 ) ) ;
#7893 = EDGE_LOOP ( 'NONE', ( #8702, #29721, #25430, #8762 ) ) ;
#7894 = CARTESIAN_POINT ( 'NONE',  ( 22.60769515458673595, 248.8388461906613998, 5.999999999999999112 ) ) ;
#7895 = CARTESIAN_POINT ( 'NONE',  ( -12.46528703574805697, 114.1976862821014720, -2.660918448318280838 ) ) ;
#7896 = CARTESIAN_POINT ( 'NONE',  ( 0.1745138560725837118, 61.01018628210145067, -15.50000000000000533 ) ) ;
#7897 = CARTESIAN_POINT ( 'NONE',  ( 15.02283181144952628, 7.347880794884122694E-16, 50.52293445648592751 ) ) ;
#7898 = CARTESIAN_POINT ( 'NONE',  ( 31.07874456373121319, 7.209453229046482114, 165.2005775096280615 ) ) ;
#7899 = CARTESIAN_POINT ( 'NONE',  ( -11.08355503943142573, 94.36018628210146630, 10.83675517735155402 ) ) ;
#7900 =( BOUNDED_CURVE ( )  B_SPLINE_CURVE ( 2, ( #565, #14802, #26916, #20680, #35064, #8921, #35249 ),
 .UNSPECIFIED., .F., .F. ) 
 B_SPLINE_CURVE_WITH_KNOTS ( ( 3, 2, 2, 3 ),
 ( 0.4130434782608697342, 0.4202898550724640248, 0.4275362318840583153, 0.4347826086956526059 ),
 .UNSPECIFIED. ) 
 CURVE ( )  GEOMETRIC_REPRESENTATION_ITEM ( )  RATIONAL_B_SPLINE_CURVE ( ( 0.9999999999999968914, 0.8660254037844418162, 1.000000000000000000, 0.8660254037844387076, 1.000000000000000000, 0.8660254037844304920, 1.000000000000008216 ) ) 
 REPRESENTATION_ITEM ( '' )  );
#7901 = CARTESIAN_POINT ( 'NONE',  ( -42.87872103062156981, 203.4690446883607535, 1.626142955000567936 ) ) ;
#7902 = CARTESIAN_POINT ( 'NONE',  ( 19.68408634441910365, -5.407089921784855591, -6.290624999385540761 ) ) ;
#7903 = CARTESIAN_POINT ( 'NONE',  ( 3.796722387233379514, 15.58518628210145351, -8.710071997420127943 ) ) ;
#7904 = CARTESIAN_POINT ( 'NONE',  ( 26.99999999999999645, 7.347880794884117764E-16, -3.374999999999989342 ) ) ;
#7905 = CARTESIAN_POINT ( 'NONE',  ( -68.21205436395489130, 214.6737587650352168, 4.842901733360204908 ) ) ;
#7906 = DIRECTION ( 'NONE',  ( -0.1219804832088935975, -0.9925324990730152175, 0.000000000000000000 ) ) ;
#7907 = CARTESIAN_POINT ( 'NONE',  ( -12.53471296425194836, 58.42268628210145209, 2.311890736173176641 ) ) ;
#7908 = CARTESIAN_POINT ( 'NONE',  ( -27.00000000000000355, 198.2000000000000171, 0.000000000000000000 ) ) ;
#7909 = CARTESIAN_POINT ( 'NONE',  ( 21.00000000000000355, 0.000000000000000000, 50.00000000000001421 ) ) ;
#7911 = CARTESIAN_POINT ( 'NONE',  ( 16.56230152254411436, -7.209453229046482114, -1.884374999385517446 ) ) ;
#7910 = CARTESIAN_POINT ( 'NONE',  ( 8.710071997420127943, 27.08518628210144996, 3.796722387233375073 ) ) ;
#7912 = VERTEX_POINT ( 'NONE', #8175 ) ;
#7913 = CARTESIAN_POINT ( 'NONE',  ( 23.99999999999999645, 5.196152422706631135, -2.849999999999991651 ) ) ;
#7914 = CARTESIAN_POINT ( 'NONE',  ( 25.83310289917887559, -3.320084631957848309, -8.000000000000000000 ) ) ;
#7915 = VECTOR ( 'NONE', #20232, 1000.000000000000000 ) ;
#7916 = CARTESIAN_POINT ( 'NONE',  ( 33.75396078491245078, 5.407089921784862696, 159.9599749780466027 ) ) ;
#7917 = CARTESIAN_POINT ( 'NONE',  ( 22.80587116629411071, 3.604726614523238837, -2.128124999385546001 ) ) ;
#7918 = CARTESIAN_POINT ( 'NONE',  ( 33.59750473220383071, -5.196152422706635576, 159.5689982363720674 ) ) ;
#7919 = CARTESIAN_POINT ( 'NONE',  ( 21.00000000000000000, 244.0374999999999943, -6.928203230275506996 ) ) ;
#7920 = FACE_OUTER_BOUND ( 'NONE', #36758, .T. ) ;
#7921 = CARTESIAN_POINT ( 'NONE',  ( 12.50000000000000355, 93.88981371789856212, -0.1745138560722771515 ) ) ;
#7922 = CARTESIAN_POINT ( 'NONE',  ( 12.53471296425194659, 81.42268628210145209, -2.311890736173178418 ) ) ;
#7923 = ORIENTED_EDGE ( 'NONE', *, *, #24856, .F. ) ;
#7924 = VERTEX_POINT ( 'NONE', #19189 ) ;
#7925 = CARTESIAN_POINT ( 'NONE',  ( 27.00000000000000355, 198.5375000012290627, -3.306546357697854128E-15 ) ) ;
#7926 = FACE_OUTER_BOUND ( 'NONE', #9169, .T. ) ;
#7927 = CARTESIAN_POINT ( 'NONE',  ( 3.257655550456945548, 49.90231371789854364, 15.46528703574811736 ) ) ;
#7928 = CARTESIAN_POINT ( 'NONE',  ( 26.75643035624999655, 7.049594010296217766E-16, -9.928124999385474325 ) ) ;
#7929 = CARTESIAN_POINT ( 'NONE',  ( 15.24356964375000167, 242.2468750006145228, 3.323476615752272600 ) ) ;
#7930 = AXIS2_PLACEMENT_3D ( 'NONE', #31281, #1906, #30550 ) ;
#7931 = CARTESIAN_POINT ( 'NONE',  ( -55.34747103062157692, 212.3500491399821613, -3.839350919129076445 ) ) ;
#7932 = CARTESIAN_POINT ( 'NONE',  ( -1.715153634034442431, 41.27731371789855075, 9.534712964251900402 ) ) ;
#7933 = CARTESIAN_POINT ( 'NONE',  ( -68.21205436395489130, 214.6737587650352168, 4.842901733360204908 ) ) ;
#7934 = CARTESIAN_POINT ( 'NONE',  ( 6.840914352311949109, 85.83981371789856496, 6.594114490232462877 ) ) ;
#7935 = CARTESIAN_POINT ( 'NONE',  ( 13.62178482187501416, 198.6593750006145456, 23.59362340125806767 ) ) ;
#7936 = CARTESIAN_POINT ( 'NONE',  ( -8.962234695871565293, 16.83981371789855430, -8.715434833792128799 ) ) ;
#7937 = CARTESIAN_POINT ( 'NONE',  ( -0.1745138560725500443, 56.41018628210145636, 12.50000000000000355 ) ) ;
#7938 = CARTESIAN_POINT ( 'NONE',  ( 13.56230152254411436, -5.196152422706632912, -8.362499998771033560 ) ) ;
#7939 = CARTESIAN_POINT ( 'NONE',  ( 22.60769515458672529, 245.3674038105676800, -6.000000000000004441 ) ) ;
#7940 = CARTESIAN_POINT ( 'NONE',  ( 36.89818384675449892, -3.604726614523235284, 160.0801451655713663 ) ) ;
#7941 = CARTESIAN_POINT ( 'NONE',  ( 34.16946429409239983, 5.196152422706631135, 166.1065259438235557 ) ) ;
#7942 = CARTESIAN_POINT ( 'NONE',  ( 19.68408634441911431, -5.407089921784861808, -6.346874999385549110 ) ) ;
#7943 = CARTESIAN_POINT ( 'NONE',  ( 27.00000000000001421, 197.1500000012290172, 15.58845726811988897 ) ) ;
#7944 = DIRECTION ( 'NONE',  ( 0.000000000000000000, 0.000000000000000000, 1.000000000000000000 ) ) ;
#7945 = CARTESIAN_POINT ( 'NONE',  ( 9.465287035748067623, 72.79768628210145209, 2.064181346179272847 ) ) ;
#7946 = LINE ( 'NONE', #33719, #1332 ) ;
#7947 = CARTESIAN_POINT ( 'NONE',  ( -7.228626920339069173, 121.6726862821014521, 10.49813415415989581 ) ) ;
#7948 = CARTESIAN_POINT ( 'NONE',  ( -7.234628195640328663, 197.3924038105676857, 26.99999999999999289 ) ) ;
#7949 = FACE_OUTER_BOUND ( 'NONE', #5096, .T. ) ;
#7951 = ORIENTED_EDGE ( 'NONE', *, *, #20756, .F. ) ;
#7950 = CIRCLE ( 'NONE', #27315, 8.000000000000000000 ) ;
#7952 = CARTESIAN_POINT ( 'NONE',  ( 30.98559686366964883, -7.209453229046475009, 164.1358944260424835 ) ) ;
#7953 = CARTESIAN_POINT ( 'NONE',  ( 18.12178482187500350, -4.985214923628407568, -5.915624999385471483 ) ) ;
#7954 = CARTESIAN_POINT ( 'NONE',  ( -27.24356964375000345, 197.1593750006145456, 0.000000000000000000 ) ) ;
#7955 = CARTESIAN_POINT ( 'NONE',  ( 28.16820783713129472, 5.407089921784862696, 167.7514543563617622 ) ) ;
#7956 = CARTESIAN_POINT ( 'NONE',  ( 37.41951561650348168, 3.464101615137759271, 168.8336428086314527 ) ) ;
#7957 = DIRECTION ( 'NONE',  ( 1.000000000000000000, 0.000000000000000000, 0.000000000000000000 ) ) ;
#7958 = CARTESIAN_POINT ( 'NONE',  ( 23.87821517812499650, 240.7093750006145285, -4.985214923628404904 ) ) ;
#7959 = CYLINDRICAL_SURFACE ( 'NONE', #35405, 6.000000000000005329 ) ;
#7960 = EDGE_CURVE ( 'NONE', #23722, #5552, #2792, .T. ) ;
#7961 = CARTESIAN_POINT ( 'NONE',  ( -11.61527771782809282, 135.8648137178985849, -4.622313124798832717 ) ) ;
#7962 = CARTESIAN_POINT ( 'NONE',  ( 7.228626920339069173, 135.4726862821014493, -10.49813415415989404 ) ) ;
#7964 = ORIENTED_EDGE ( 'NONE', *, *, #25867, .T. ) ;
#7963 = VERTEX_POINT ( 'NONE', #31288 ) ;
#7965 = CARTESIAN_POINT ( 'NONE',  ( 15.24356964374999990, 243.8968750006145285, 0.000000000000000000 ) ) ;
#7966 = DIRECTION ( 'NONE',  ( 1.000000000000000000, 0.000000000000000000, 0.000000000000000000 ) ) ;
#7967 = CARTESIAN_POINT ( 'NONE',  ( 18.12178482187499640, 4.985214923628404904, -5.165624999385470595 ) ) ;
#7968 = CARTESIAN_POINT ( 'NONE',  ( -13.04141134922778456, 116.0273137178985792, 8.927990412390377273 ) ) ;
#7969 = CARTESIAN_POINT ( 'NONE',  ( -42.15435043487494227, 254.8329415120769852, 5.000000000000000000 ) ) ;
#7970 = CARTESIAN_POINT ( 'NONE',  ( 15.24356964374999990, 3.323476615752268604, -2.990624999385476102 ) ) ;
#7971 = CARTESIAN_POINT ( 'NONE',  ( 13.44051670066911264, -5.407089921784865361, -8.221874999385537564 ) ) ;
#7972 = CARTESIAN_POINT ( 'NONE',  ( 13.62178482187501416, 195.0031250006145456, 23.59362340125806767 ) ) ;
#7973 = AXIS2_PLACEMENT_3D ( 'NONE', #28857, #238, #14843 ) ;
#7974 = CARTESIAN_POINT ( 'NONE',  ( 0.1745138560725515708, 107.0101862821014578, -12.50000000000000355 ) ) ;
#7975 = CARTESIAN_POINT ( 'NONE',  ( 22.80587116629410360, 7.646167579472015790E-16, -2.615624999385557370 ) ) ;
#7976 = EDGE_CURVE ( 'NONE', #36216, #15548, #5315, .T. ) ;
#7977 = CARTESIAN_POINT ( 'NONE',  ( -47.62127896937850124, 218.5309553116392465, 2.162041339862725842 ) ) ;
#7978 = CARTESIAN_POINT ( 'NONE',  ( 23.87821517812499650, 244.1968750006145115, -4.985214923628404904 ) ) ;
#7979 = CARTESIAN_POINT ( 'NONE',  ( -4.500000000000000888, 210.0000000000000284, 2.500000000000000000 ) ) ;
#7980 = CARTESIAN_POINT ( 'NONE',  ( -37.52752896937849414, 212.3500491399821613, 3.839350919129088435 ) ) ;
#7981 = CARTESIAN_POINT ( 'NONE',  ( 12.46528703574805874, 127.9976862821014407, 2.660918448318279950 ) ) ;
#7982 = CARTESIAN_POINT ( 'NONE',  ( 13.56230152254411436, -5.196152422706632912, -1.612499998771027565 ) ) ;
#7983 = EDGE_CURVE ( 'NONE', #15182, #21163, #23391, .T. ) ;
#7984 = CARTESIAN_POINT ( 'NONE',  ( -42.48288769728824121, 203.5309553116391612, -1.857196546604028775 ) ) ;
#7985 = DIRECTION ( 'NONE',  ( 0.000000000000000000, 1.000000000000000000, 0.000000000000000000 ) ) ;
#7986 = CARTESIAN_POINT ( 'NONE',  ( -14.38691631536207183, 122.5351862821014493, 5.770363421893814682 ) ) ;
#7987 = CARTESIAN_POINT ( 'NONE',  ( 16.56230152254410726, 0.000000000000000000, 10.00000000000000000 ) ) ;
#7988 = CARTESIAN_POINT ( 'NONE',  ( 2.311890736173175753, 10.12268628210144428, 12.53471296425194836 ) ) ;
#7989 = CARTESIAN_POINT ( 'NONE',  ( 16.56230152254411081, 6.928203230275514990, -9.112500000000034461 ) ) ;
#7990 = CARTESIAN_POINT ( 'NONE',  ( 22.60769515458672529, 245.8736538117967143, -6.000000000000004441 ) ) ;
#7991 = ORIENTED_EDGE ( 'NONE', *, *, #23485, .T. ) ;
#7992 = FACE_OUTER_BOUND ( 'NONE', #6735, .T. ) ;
#7993 = CARTESIAN_POINT ( 'NONE',  ( -6.840914352312096547, 75.96018628210144641, 6.594114490232313663 ) ) ;
#7994 = VECTOR ( 'NONE', #5834, 1000.000000000000000 ) ;
#7995 = FILL_AREA_STYLE_COLOUR ( '', #23641 ) ;
#7996 = CARTESIAN_POINT ( 'NONE',  ( 27.24356964375000345, 196.4281250006145569, -3.336375036156643733E-15 ) ) ;
#7997 = CARTESIAN_POINT ( 'NONE',  ( 20.99999999999999645, 0.000000000000000000, -8.000000000000000000 ) ) ;
#7998 = CARTESIAN_POINT ( 'NONE',  ( -13.62178482187500528, 197.0843750006145285, -23.59362340125807123 ) ) ;
#7999 = DIRECTION ( 'NONE',  ( 0.000000000000000000, 0.000000000000000000, -1.000000000000000000 ) ) ;
#8000 = CARTESIAN_POINT ( 'NONE',  ( 10.56230152254379107, 3.464101615137573198, -3.637500000000023714 ) ) ;
#8001 = CARTESIAN_POINT ( 'NONE',  ( -3.474262827703527901, 50.76481371789856212, 8.843639120294245259 ) ) ;
#8002 = CARTESIAN_POINT ( 'NONE',  ( 18.00000000000000355, -5.196152422706632912, -8.475000000000010303 ) ) ;
#8003 = ORIENTED_EDGE ( 'NONE', *, *, #9607, .F. ) ;
#8004 = CARTESIAN_POINT ( 'NONE',  ( 18.00000000000000000, 240.9812500012290570, -5.196152422706630247 ) ) ;
#8005 = CARTESIAN_POINT ( 'NONE',  ( -11.48171059495408208, 61.11481371789854933, 4.944772684328421875 ) ) ;
#8006 = CARTESIAN_POINT ( 'NONE',  ( 19.68408634441911431, -5.407089921784861808, -5.896874999385542715 ) ) ;
#8007 = CARTESIAN_POINT ( 'NONE',  ( 15.24356964374999990, 0.000000000000000000, -6.553124999385484983 ) ) ;
#8008 = CARTESIAN_POINT ( 'NONE',  ( 10.49813415416005213, 28.62731371789854506, -7.228626920338837358 ) ) ;
#8009 = ORIENTED_EDGE ( 'NONE', *, *, #25166, .F. ) ;
#8010 = CARTESIAN_POINT ( 'NONE',  ( 13.44051670066911264, -5.407089921784865361, -2.371874999385514826 ) ) ;
#8011 = LINE ( 'NONE', #7829, #22826 ) ;
#8012 = EDGE_CURVE ( 'NONE', #29322, #6148, #10771, .T. ) ;
#8013 = CARTESIAN_POINT ( 'NONE',  ( 37.56002276824448671, -3.604726614523238837, 167.6449986542055797 ) ) ;
#8014 = CARTESIAN_POINT ( 'NONE',  ( -40.89211230271181563, 203.5309553116391612, 1.857196546604092280 ) ) ;
#8015 = CARTESIAN_POINT ( 'NONE',  ( 19.56230152254410726, 5.196152422706631135, -0.4874999987710126881 ) ) ;
#8016 = ADVANCED_FACE ( 'NONE', ( #31652 ), #28613, .F. ) ;
#8017 = DIRECTION ( 'NONE',  ( -0.8083506638593009885, -0.5887012860850802110, 1.927470528863119295E-16 ) ) ;
#8018 = CARTESIAN_POINT ( 'NONE',  ( 11.61527771782809637, 76.06481371789855928, 4.622313124798827388 ) ) ;
#8019 = CARTESIAN_POINT ( 'NONE',  ( -66.02752896937849414, 212.3500491399821613, 3.839350919129088435 ) ) ;
#8020 = CARTESIAN_POINT ( 'NONE',  ( -44.85788769728821990, 216.4690446883607535, 1.857196546604031662 ) ) ;
#8021 = EDGE_LOOP ( 'NONE', ( #24673, #27021, #28004, #25561 ) ) ;
#8022 = DIRECTION ( 'NONE',  ( 1.000000000000000000, 0.000000000000000000, 0.000000000000000000 ) ) ;
#8023 = CARTESIAN_POINT ( 'NONE',  ( -14.29273924364230908, 215.8523247127875493, -5.456133016108021927 ) ) ;
#8024 = CARTESIAN_POINT ( 'NONE',  ( 11.08355503943118769, 39.83981371789855075, 10.83675517735179028 ) ) ;
#8025 = CARTESIAN_POINT ( 'NONE',  ( -67.02455436395489130, 203.6929966515020283, 6.137860380172978303 ) ) ;
#8026 = PRODUCT_DEFINITION_SHAPE ( 'NONE', 'NONE',  #37502 ) ;
#8027 = CARTESIAN_POINT ( 'NONE',  ( 6.932735513423970097, 9.547686282101453870, 10.69584247140445044 ) ) ;
#8028 = CARTESIAN_POINT ( 'NONE',  ( -12.50000000000000355, 58.71018628210145351, -0.1745138560725492671 ) ) ;
#8029 = CARTESIAN_POINT ( 'NONE',  ( -15.50000000000000533, 3.510186282101451560, -0.1745138560725808530 ) ) ;
#8031 = EDGE_CURVE ( 'NONE', #26868, #30804, #17810, .T. ) ;
#8030 = CARTESIAN_POINT ( 'NONE',  ( 10.56230152254411614, -3.464101615137761048, -2.662500000000041833 ) ) ;
#8032 = CARTESIAN_POINT ( 'NONE',  ( 7.234628195640269155, 194.8450961906613941, 27.00000000000003197 ) ) ;
#8033 = VERTEX_POINT ( 'NONE', #34496 ) ;
#8034 = CARTESIAN_POINT ( 'NONE',  ( 6.092822981423978490, 24.78518628210144215, -14.25334919248782306 ) ) ;
#8035 = CARTESIAN_POINT ( 'NONE',  ( 13.62178482187499640, 196.0531250006145285, -23.59362340125807123 ) ) ;
#8036 = CARTESIAN_POINT ( 'NONE',  ( -13.62178482187498396, 199.4843750006145626, 23.59362340125808188 ) ) ;
#8037 = CARTESIAN_POINT ( 'NONE',  ( -27.24356964375000345, 199.8593750006145342, 0.000000000000000000 ) ) ;
#8038 = CARTESIAN_POINT ( 'NONE',  ( 20.99999999999999645, 210.0000000000000284, -8.000000000000000000 ) ) ;
#8039 = CYLINDRICAL_SURFACE ( 'NONE', #14032, 8.000000000000000000 ) ;
#8040 = CARTESIAN_POINT ( 'NONE',  ( 7.228626920339068285, 6.672686282101436106, -10.49813415415989581 ) ) ;
#8041 = CARTESIAN_POINT ( 'NONE',  ( 21.00000000000000000, 248.3968750006145285, -6.646953231504538984 ) ) ;
#8042 = CARTESIAN_POINT ( 'NONE',  ( -8.152565276336593669, 108.5523137178985422, -5.233372021372610483 ) ) ;
#8043 = CARTESIAN_POINT ( 'NONE',  ( 23.87821517812500005, 241.9093750006145456, 4.985214923628404016 ) ) ;
#8044 = ORIENTED_EDGE ( 'NONE', *, *, #16436, .T. ) ;
#8045 = CARTESIAN_POINT ( 'NONE',  ( -64.25372103062154849, 216.5309553116391612, -1.626142955000564383 ) ) ;
#8046 = CARTESIAN_POINT ( 'NONE',  ( 16.56230152254411436, -6.928203230275514990, -7.087500000000036771 ) ) ;
#8047 = CARTESIAN_POINT ( 'NONE',  ( -27.00000000000000355, 200.0000000000000000, 0.000000000000000000 ) ) ;
#8048 = EDGE_CURVE ( 'NONE', #31903, #16958, #26041, .T. ) ;
#8049 = CARTESIAN_POINT ( 'NONE',  ( -11.48171059495408208, 125.5148137178985763, 4.944772684328421875 ) ) ;
#8050 = CARTESIAN_POINT ( 'NONE',  ( 19.68408634441910365, 5.407089921784857367, -9.740624999385548932 ) ) ;
#8051 = CARTESIAN_POINT ( 'NONE',  ( 37.02238078016989675, 3.604726614523238837, 161.4997226103520802 ) ) ;
#8052 = CARTESIAN_POINT ( 'NONE',  ( 36.90311784072428480, -3.464101615137388013, 162.9311892224378369 ) ) ;
#8053 = CARTESIAN_POINT ( 'NONE',  ( -27.00000000000000355, 196.4000000000000057, 0.000000000000000000 ) ) ;
#8054 = CIRCLE ( 'NONE', #28598, 4.899999999999999467 ) ;
#8055 = VERTEX_POINT ( 'NONE', #3214 ) ;
#8056 = VERTEX_POINT ( 'NONE', #25965 ) ;
#8057 = ORIENTED_EDGE ( 'NONE', *, *, #11411, .T. ) ;
#8058 = CARTESIAN_POINT ( 'NONE',  ( 15.00000000000000000, 0.000000000000000000, -3.993749998770945719 ) ) ;
#8059 = CARTESIAN_POINT ( 'NONE',  ( 26.75643035624999655, 7.049594010296217766E-16, -1.715624999385462202 ) ) ;
#8060 = CARTESIAN_POINT ( 'NONE',  ( 15.00000000000000000, 241.9187500012290570, -3.464101615137752610 ) ) ;
#8061 = CARTESIAN_POINT ( 'NONE',  ( -77.00000000000002842, 210.0000000000000000, 2.500000000000001332 ) ) ;
#8062 = CARTESIAN_POINT ( 'NONE',  ( 23.87821517812499650, 248.6968750006145115, -4.985214923628404904 ) ) ;
#8063 = CARTESIAN_POINT ( 'NONE',  ( 2.311890736173175753, 56.12268628210144072, 12.53471296425194836 ) ) ;
#8064 =( BOUNDED_CURVE ( )  B_SPLINE_CURVE ( 2, ( #30609, #16945, #14651, #17133, #26391, #14097, #28669, #5366, #37202 ),
 .UNSPECIFIED., .F., .F. ) 
 B_SPLINE_CURVE_WITH_KNOTS ( ( 3, 2, 2, 2, 3 ),
 ( 0.9021739130434782705, 0.9057971014492753881, 0.9130434782608695121, 0.9202898550724637472, 0.9239130434782608647 ),
 .UNSPECIFIED. ) 
 CURVE ( )  GEOMETRIC_REPRESENTATION_ITEM ( )  RATIONAL_B_SPLINE_CURVE ( ( 0.9330127018922194093, 0.9330127018922194093, 1.000000000000000000, 0.8660254037844387076, 1.000000000000000000, 0.8660254037844387076, 1.000000000000000000, 0.9330127018922194093, 0.9330127018922194093 ) ) 
 REPRESENTATION_ITEM ( '' )  );
#8065 = CARTESIAN_POINT ( 'NONE',  ( -59.69419563604516554, 203.5000000000000000, 0.1155267958017914542 ) ) ;
#8066 = CARTESIAN_POINT ( 'NONE',  ( 15.38158308873937585, 224.9824450966943061, 2.114697272284774776 ) ) ;
#8067 = CARTESIAN_POINT ( 'NONE',  ( -42.87127896937849414, 214.5309553116392749, 1.090244570138288127 ) ) ;
#8068 = DIRECTION ( 'NONE',  ( -0.000000000000000000, 1.000000000000000000, -0.000000000000000000 ) ) ;
#8069 = COLOUR_RGB ( '',0.8941176470588234615, 0.8941176470588234615, 0.8941176470588234615 ) ;
#8070 = CARTESIAN_POINT ( 'NONE',  ( 36.99463137071579411, 7.347880794884117764E-16, 163.9771936566585566 ) ) ;
#8071 = CARTESIAN_POINT ( 'NONE',  ( -8.715434833792127023, 124.9398137178985593, 8.962234695871568846 ) ) ;
#8072 = CARTESIAN_POINT ( 'NONE',  ( -35.95163769728823411, 215.6869285224996986, -3.149950860017881382 ) ) ;
#8073 = CIRCLE ( 'NONE', #177, 8.000000000000000000 ) ;
#8074 = CARTESIAN_POINT ( 'NONE',  ( -40.70163769728823411, 217.4189793300686233, -4.149950860017907139 ) ) ;
#8075 = CARTESIAN_POINT ( 'NONE',  ( 20.99999999999999645, -6.646953231504538984, -1.940624999385496929 ) ) ;
#8076 = CARTESIAN_POINT ( 'NONE',  ( -27.24356964375000345, 195.7531250006145456, 0.000000000000000000 ) ) ;
#8077 = CARTESIAN_POINT ( 'NONE',  ( -8.927990412390371944, 90.72731371789855359, -13.04141134922778988 ) ) ;
#8078 = CARTESIAN_POINT ( 'NONE',  ( -65.23586230271183695, 205.8500491399821613, 7.418979330068642852 ) ) ;
#8079 = EDGE_LOOP ( 'NONE', ( #18501, #24789, #750, #15110 ) ) ;
#8080 = DIRECTION ( 'NONE',  ( 0.08715574274765150453, 0.000000000000000000, 0.9961946980917461003 ) ) ;
#8081 = CARTESIAN_POINT ( 'NONE',  ( 11.48171059495397728, 119.0851862821014606, 4.944772684328674117 ) ) ;
#8082 = CARTESIAN_POINT ( 'NONE',  ( -13.23911966647218463, 57.84768628210144925, 8.632099005475506459 ) ) ;
#8083 = CARTESIAN_POINT ( 'NONE',  ( 25.13507686385270290, 3.464101615137630485, 166.1064243038051416 ) ) ;
#8084 =( BOUNDED_CURVE ( )  B_SPLINE_CURVE ( 2, ( #27537, #21116, #997, #33225, #24140, #13134, #6696, #35682, #15606 ),
 .UNSPECIFIED., .F., .F. ) 
 B_SPLINE_CURVE_WITH_KNOTS ( ( 3, 2, 2, 2, 3 ),
 ( 0.6847826086956522174, 0.6884057971014492239, 0.6956521739130434590, 0.7028985507246376940, 0.7065217391304348116 ),
 .UNSPECIFIED. ) 
 CURVE ( )  GEOMETRIC_REPRESENTATION_ITEM ( )  RATIONAL_B_SPLINE_CURVE ( ( 0.9330127018922192983, 0.9330127018922202975, 1.000000000000000000, 0.8660254037844387076, 1.000000000000000000, 0.8660254037844387076, 1.000000000000000000, 0.9330127018922194093, 0.9330127018922194093 ) ) 
 REPRESENTATION_ITEM ( '' )  );
#8085 = CARTESIAN_POINT ( 'NONE',  ( 24.55497793462844669, 0.000000000000000000, 162.2705114497308045 ) ) ;
#8086 = CARTESIAN_POINT ( 'NONE',  ( 6.092822981423978490, 89.18518628210145494, -14.25334919248782306 ) ) ;
#8087 = CARTESIAN_POINT ( 'NONE',  ( -40.70163769728823411, 215.6869285224996986, -3.149950860017881382 ) ) ;
#8088 = EDGE_CURVE ( 'NONE', #24310, #17657, #14639, .T. ) ;
#8089 = CARTESIAN_POINT ( 'NONE',  ( 22.80587116629410716, -3.604726614523235284, -6.703124999385561722 ) ) ;
#8090 = CARTESIAN_POINT ( 'NONE',  ( -6.840914352312096547, 20.76018628210144001, 6.594114490232313663 ) ) ;
#8091 = ADVANCED_FACE ( 'NONE', ( #29363 ), #25778, .F. ) ;
#8092 = DIRECTION ( 'NONE',  ( 0.000000000000000000, 0.000000000000000000, -1.000000000000000000 ) ) ;
#8093 = CARTESIAN_POINT ( 'NONE',  ( -58.31622103062155560, 211.6261429550005744, 6.530955311639227823 ) ) ;
#8094 = DIRECTION ( 'NONE',  ( 2.168404344971009176E-17, 0.000000000000000000, 1.000000000000000000 ) ) ;
#8095 = CARTESIAN_POINT ( 'NONE',  ( -4.622313124798576922, 60.43518628210145494, -11.61527771782819762 ) ) ;
#8096 = CARTESIAN_POINT ( 'NONE',  ( -13.49999999999998401, 197.3750000000000284, 23.38268590217985476 ) ) ;
#8097 = CARTESIAN_POINT ( 'NONE',  ( 10.56230152254410726, 0.000000000000000000, -6.637499998771001941 ) ) ;
#8098 = CARTESIAN_POINT ( 'NONE',  ( 2.064181346179272847, 33.69768628210143646, -9.465287035748065847 ) ) ;
#8099 = CARTESIAN_POINT ( 'NONE',  ( 23.87821517812500005, 248.6593750006145171, 4.985214923628404016 ) ) ;
#8100 = ORIENTED_EDGE ( 'NONE', *, *, #17818, .F. ) ;
#8101 = CARTESIAN_POINT ( 'NONE',  ( 21.00000000000000000, 6.928203230275506996, -3.712500000000020339 ) ) ;
#8102 = CARTESIAN_POINT ( 'NONE',  ( 26.60793733450167053, 1.299049382686714882, -8.000000000000000000 ) ) ;
#8103 = CARTESIAN_POINT ( 'NONE',  ( 36.93576976081443775, 7.646167579472024665E-16, 160.5097541291234506 ) ) ;
#8104 = CARTESIAN_POINT ( 'NONE',  ( 10.31873187879410914, 0.000000000000000000, -1.490624999385542493 ) ) ;
#8105 = CARTESIAN_POINT ( 'NONE',  ( 25.15145004905768644, -3.604726614523240613, 169.0882189147961583 ) ) ;
#8106 = CARTESIAN_POINT ( 'NONE',  ( 26.99999999999999645, 243.9625000000000057, -3.464101615137755275 ) ) ;
#8107 = CARTESIAN_POINT ( 'NONE',  ( -13.50000000000000533, 198.5749999999999886, -23.38268590217984411 ) ) ;
#8108 = AXIS2_PLACEMENT_3D ( 'NONE', #5196, #1795, #28317 ) ;
#8109 = ADVANCED_FACE ( 'NONE', ( #37328 ), #3026, .T. ) ;
#8110 = CARTESIAN_POINT ( 'NONE',  ( 12.46528703574805874, 91.19768628210145778, 2.660918448318279950 ) ) ;
#8111 = ORIENTED_EDGE ( 'NONE', *, *, #36354, .F. ) ;
#8112 = ORIENTED_EDGE ( 'NONE', *, *, #32567, .F. ) ;
#8113 = PRODUCT_RELATED_PRODUCT_CATEGORY ( 'part', '', ( #5602 ) ) ;
#8114 = CARTESIAN_POINT ( 'NONE',  ( 26.99999999999999645, 195.4250000012290229, -15.58845726811990495 ) ) ;
#8115 = DIRECTION ( 'NONE',  ( 0.000000000000000000, 1.000000000000000000, 0.000000000000000000 ) ) ;
#8116 = CARTESIAN_POINT ( 'NONE',  ( 15.53471296425188797, 66.57731371789853370, 2.908627838312457747 ) ) ;
#8117 = CARTESIAN_POINT ( 'NONE',  ( 21.00000000000000000, 6.646953231504538984, -8.465624999385484628 ) ) ;
#8118 = CARTESIAN_POINT ( 'NONE',  ( 26.75643035624999655, 242.3968750006145001, 3.323476615752267715 ) ) ;
#8119 = APPLICATION_CONTEXT ( 'automotive_design' ) ;
#8120 = CARTESIAN_POINT ( 'NONE',  ( -44.65997103062156981, 213.8393509191290889, 2.350049139982164359 ) ) ;
#8121 = CARTESIAN_POINT ( 'NONE',  ( -50.22894823740646331, 235.3444610600932094, 7.500000000000000000 ) ) ;
#8122 = CARTESIAN_POINT ( 'NONE',  ( 24.63341810310133084, 0.000000000000000000, 163.1670866780133906 ) ) ;
#8123 = CARTESIAN_POINT ( 'NONE',  ( -6.840914352311947333, 44.43981371789855928, -6.594114490232462877 ) ) ;
#8124 = CARTESIAN_POINT ( 'NONE',  ( -66.03497103062157692, 204.4285982733020148, -3.350049139982115509 ) ) ;
#8125 = CARTESIAN_POINT ( 'NONE',  ( 8.152565276336593669, 85.55231371789855643, 5.233372021372610483 ) ) ;
#8126 = CARTESIAN_POINT ( 'NONE',  ( 27.24356964375000345, 197.8343750006145569, -3.336375036156643733E-15 ) ) ;
#8127 = CARTESIAN_POINT ( 'NONE',  ( -13.04141134922778456, 143.6273137178985451, 8.927990412390377273 ) ) ;
#8128 =( BOUNDED_CURVE ( )  B_SPLINE_CURVE ( 2, ( #29843, #7479, #35530, #10133, #1597, #843, #21338, #23986, #15828 ),
 .UNSPECIFIED., .F., .F. ) 
 B_SPLINE_CURVE_WITH_KNOTS ( ( 3, 2, 2, 2, 3 ),
 ( 0.8125000000000000000, 0.8194444444444444198, 0.8333333333333333703, 0.8472222222222222099, 0.8541666666666667407 ),
 .UNSPECIFIED. ) 
 CURVE ( )  GEOMETRIC_REPRESENTATION_ITEM ( )  RATIONAL_B_SPLINE_CURVE ( ( 0.9330127018922194093, 0.9330127018922194093, 1.000000000000000000, 0.8660254037844387076, 1.000000000000000000, 0.8660254037844387076, 1.000000000000000000, 0.9330127018922187432, 0.9330127018922192983 ) ) 
 REPRESENTATION_ITEM ( '' )  );
#8129 = CARTESIAN_POINT ( 'NONE',  ( 22.60769515458672885, 239.8388461906613429, 5.999999999999997335 ) ) ;
#8130 = CARTESIAN_POINT ( 'NONE',  ( -10.49813415415989581, 68.77268628210146062, -7.228626920339068285 ) ) ;
#8131 = CARTESIAN_POINT ( 'NONE',  ( 0.000000000000000000, 222.9518338469886203, -2.500000000000000000 ) ) ;
#8132 = FACE_OUTER_BOUND ( 'NONE', #18180, .T. ) ;
#8133 = CARTESIAN_POINT ( 'NONE',  ( 37.05833252405330569, 7.646167579472015790E-16, 161.9106529233149274 ) ) ;
#8134 = DIRECTION ( 'NONE',  ( 0.000000000000000000, 0.000000000000000000, 1.000000000000000000 ) ) ;
#8135 = CARTESIAN_POINT ( 'NONE',  ( 13.44051670066911441, -5.407089921784865361, -7.321874999385524774 ) ) ;
#8136 = CARTESIAN_POINT ( 'NONE',  ( 16.56230152254410726, 0.000000000000000000, -10.00000000000000000 ) ) ;
#8137 = CARTESIAN_POINT ( 'NONE',  ( 10.56230152254410903, 7.347880794884117764E-16, -10.00000000000000000 ) ) ;
#8138 = CARTESIAN_POINT ( 'NONE',  ( -8.152565276336710909, 76.24768628210145494, 5.233372021372435512 ) ) ;
#8139 = DIRECTION ( 'NONE',  ( 0.000000000000000000, 0.000000000000000000, -1.000000000000000000 ) ) ;
#8140 = CARTESIAN_POINT ( 'NONE',  ( 12.46528703574805874, 118.7976862821014663, 2.660918448318279950 ) ) ;
#8141 = DIRECTION ( 'NONE',  ( -0.8083506638593009885, -0.5887012860850802110, 1.927470528863119295E-16 ) ) ;
#8142 = CARTESIAN_POINT ( 'NONE',  ( 22.60769515458672885, 240.2888461906613884, 5.999999999999997335 ) ) ;
#8143 = ORIENTED_EDGE ( 'NONE', *, *, #26746, .T. ) ;
#8144 = CARTESIAN_POINT ( 'NONE',  ( 24.55988044515800439, 0.000000000000000000, 162.3265474014984591 ) ) ;
#8145 = CARTESIAN_POINT ( 'NONE',  ( 15.24356964374999990, 0.000000000000000000, -6.440624999385469174 ) ) ;
#8146 = CARTESIAN_POINT ( 'NONE',  ( -27.24356964375000345, 198.0218750006145569, -15.72908226750537786 ) ) ;
#8147 = CARTESIAN_POINT ( 'NONE',  ( 37.56329110859752518, 7.646167579472024665E-16, 167.6823559553839971 ) ) ;
#8148 = CARTESIAN_POINT ( 'NONE',  ( 28.20210112649392542, -5.196152422706638241, 166.7415323026203851 ) ) ;
#8149 = DIRECTION ( 'NONE',  ( -0.000000000000000000, 1.000000000000000000, -0.000000000000000000 ) ) ;
#8150 = CARTESIAN_POINT ( 'NONE',  ( 21.00000000000000000, 241.6468750006145285, -6.646953231504538984 ) ) ;
#8151 = CARTESIAN_POINT ( 'NONE',  ( -89.59418277001439890, 62.43429747954478159, 5.000000000000000000 ) ) ;
#8152 = CARTESIAN_POINT ( 'NONE',  ( 12.46528703574811558, 130.4023137178985792, -2.660918448318005503 ) ) ;
#8153 = CARTESIAN_POINT ( 'NONE',  ( -12.50000000000000355, 141.5101862821014720, -0.1745138560725508214 ) ) ;
#8155 = VERTEX_POINT ( 'NONE', #2837 ) ;
#8154 = EDGE_LOOP ( 'NONE', ( #28821, #2546, #20599, #10061, #36654 ) ) ;
#8156 = CIRCLE ( 'NONE', #17840, 2.649999999999999467 ) ;
#8157 = CARTESIAN_POINT ( 'NONE',  ( 15.24356964374999990, 245.2093750006145285, -3.323476615752268604 ) ) ;
#8158 = CARTESIAN_POINT ( 'NONE',  ( 10.69584247140429589, 11.95231371789853902, 6.932735513424201024 ) ) ;
#8159 = CARTESIAN_POINT ( 'NONE',  ( 15.24356964374999990, 0.000000000000000000, -2.840624999385477079 ) ) ;
#8160 = CARTESIAN_POINT ( 'NONE',  ( 5.770363421894130873, 110.5648137178985593, -14.38691631536193860 ) ) ;
#8161 = CARTESIAN_POINT ( 'NONE',  ( 13.70341545108635195, -5.565789069430963742, -9.999999999999987566 ) ) ;
#8162 = CARTESIAN_POINT ( 'NONE',  ( 18.12178482187499640, 4.985214923628404904, -1.228124999385488136 ) ) ;
#8163 = CARTESIAN_POINT ( 'NONE',  ( 22.80587116629411781, -3.604726614523238837, -8.559374999385489957 ) ) ;
#8164 = CARTESIAN_POINT ( 'NONE',  ( -27.00000000000000355, 199.6625000012290343, 0.000000000000000000 ) ) ;
#8165 = CARTESIAN_POINT ( 'NONE',  ( -11.48171059495397373, 105.2851862821014493, -4.944772684328680334 ) ) ;
#8166 = CARTESIAN_POINT ( 'NONE',  ( 19.68408634441910721, 5.407089921784857367, -3.890624999385555505 ) ) ;
#8167 = CARTESIAN_POINT ( 'NONE',  ( -45.04836230271183695, 202.5810206699313767, -4.149950860017804111 ) ) ;
#8168 = CARTESIAN_POINT ( 'NONE',  ( 15.24356964374999990, 243.8968750006145285, 0.000000000000000000 ) ) ;
#8169 = CARTESIAN_POINT ( 'NONE',  ( 22.56230152254410015, 7.347880794884117764E-16, -2.812499998771006204 ) ) ;
#8170 = CARTESIAN_POINT ( 'NONE',  ( -35.94419563604516554, 205.4999999999999716, 0.1155267958017633378 ) ) ;
#8171 = CARTESIAN_POINT ( 'NONE',  ( -10.69584247140444866, 122.2476862821014549, 6.932735513423972762 ) ) ;
#8172 = CARTESIAN_POINT ( 'NONE',  ( 22.56230152254410370, 7.347880794884117764E-16, -4.612499998771030008 ) ) ;
#8173 = CARTESIAN_POINT ( 'NONE',  ( -46.04538769728823411, 211.8571965466039444, -6.469044688360768625 ) ) ;
#8174 = DIRECTION ( 'NONE',  ( 0.000000000000000000, 0.000000000000000000, 1.000000000000000000 ) ) ;
#8175 = CARTESIAN_POINT ( 'NONE',  ( 36.60243052835136268, 7.347880794884117764E-16, 159.4943175152456831 ) ) ;
#8176 = CARTESIAN_POINT ( 'NONE',  ( 0.1745138560725837118, 97.81018628210145494, -15.50000000000000533 ) ) ;
#8177 = CARTESIAN_POINT ( 'NONE',  ( -11.48171059495397373, 13.28518628210142971, -4.944772684328680334 ) ) ;
#8178 = CARTESIAN_POINT ( 'NONE',  ( 27.00000000000000355, 197.9750000000000227, -3.306546357697854128E-15 ) ) ;
#8179 = CARTESIAN_POINT ( 'NONE',  ( -0.1745138560725182642, 130.0101862821014436, 9.500000000000005329 ) ) ;
#8180 = CARTESIAN_POINT ( 'NONE',  ( 10.31873187879411091, 0.000000000000000000, -2.840624999385532590 ) ) ;
#8181 = CARTESIAN_POINT ( 'NONE',  ( 0.000000000000000000, 148.0000000000000000, 0.000000000000000000 ) ) ;
#8182 = ORIENTED_EDGE ( 'NONE', *, *, #23582, .F. ) ;
#8183 = CARTESIAN_POINT ( 'NONE',  ( 22.56230152254411792, 7.347880794884125653E-16, -7.875000000000048850 ) ) ;
#8184 = CARTESIAN_POINT ( 'NONE',  ( 8.843639120294328748, 62.73518628210145920, -3.474262827703334722 ) ) ;
#8185 = PRESENTATION_STYLE_ASSIGNMENT (( #36412 ) ) ;
#8186 = CARTESIAN_POINT ( 'NONE',  ( -13.62178482187500528, 196.5781250006145342, -23.59362340125807123 ) ) ;
#8187 = CARTESIAN_POINT ( 'NONE',  ( 36.67106567565804198, 7.347880794884125653E-16, 160.2788208387686097 ) ) ;
#8188 = CARTESIAN_POINT ( 'NONE',  ( -27.24356964375000345, 195.8093750006145513, 0.000000000000000000 ) ) ;
#8189 = CARTESIAN_POINT ( 'NONE',  ( 30.99785313993998059, -6.928203230275514990, 164.2759843048494588 ) ) ;
#8190 = DIRECTION ( 'NONE',  ( 0.9961946980917462113, 0.000000000000000000, -0.08715574274765118534 ) ) ;
#8191 = CARTESIAN_POINT ( 'NONE',  ( -2.064181346179062349, 54.50231371789855928, -9.465287035748106703 ) ) ;
#8192 = CARTESIAN_POINT ( 'NONE',  ( 19.95811783012620566, 5.908847734042487865, -9.999476472876560607 ) ) ;
#8193 = ORIENTED_EDGE ( 'NONE', *, *, #34880, .F. ) ;
#8194 = CARTESIAN_POINT ( 'NONE',  ( 15.00000000000000000, 242.3687500012290457, -3.464101615137752166 ) ) ;
#8195 = CARTESIAN_POINT ( 'NONE',  ( 11.61527771782809637, 66.86481371789855643, 4.622313124798827388 ) ) ;
#8196 = CARTESIAN_POINT ( 'NONE',  ( 16.56230152254411436, 7.209453229046482114, -6.609374999385519978 ) ) ;
#8197 = CARTESIAN_POINT ( 'NONE',  ( 18.12178482187499640, 4.985214923628404904, -7.078124999385481786 ) ) ;
#8198 = CARTESIAN_POINT ( 'NONE',  ( -6.932735513424201912, 23.45231371789854791, 10.69584247140429412 ) ) ;
#8199 = VERTEX_POINT ( 'NONE', #22765 ) ;
#8200 = CARTESIAN_POINT ( 'NONE',  ( 13.44051670066911264, -5.407089921784865361, -1.471874999385502925 ) ) ;
#8201 = CARTESIAN_POINT ( 'NONE',  ( 19.39230484541326760, 246.0986538117967086, 5.999999999999999112 ) ) ;
#8202 = CARTESIAN_POINT ( 'NONE',  ( 13.56230152254410370, 5.196152422706630247, -9.412499998771028942 ) ) ;
#8203 = VECTOR ( 'NONE', #29101, 1000.000000000000000 ) ;
#8204 = CARTESIAN_POINT ( 'NONE',  ( -45.04836230271183695, 204.3130714775002446, -3.149950860017828091 ) ) ;
#8205 = CARTESIAN_POINT ( 'NONE',  ( 30.67428744509644289, 6.928203230275506996, 160.5776114894081559 ) ) ;
#8206 = FILL_AREA_STYLE ('',( #14443 ) ) ;
#8207 = DIRECTION ( 'NONE',  ( 1.000000000000000000, 0.000000000000000000, 0.000000000000000000 ) ) ;
#8208 = CARTESIAN_POINT ( 'NONE',  ( -39.11830436395489841, 209.8844732041982297, 4.499999999999996447 ) ) ;
#8210 = EDGE_CURVE ( 'NONE', #30563, #7963, #29282, .T. ) ;
#8209 = CARTESIAN_POINT ( 'NONE',  ( -39.51413769728823411, 213.1499508600178672, 5.686928522499718142 ) ) ;
#8211 = VERTEX_POINT ( 'NONE', #17074 ) ;
#8212 = LINE ( 'NONE', #31324, #18573 ) ;
#8213 = CARTESIAN_POINT ( 'NONE',  ( 37.26263527955736521, 3.464101615137958667, 167.0404923520663090 ) ) ;
#8214 = CARTESIAN_POINT ( 'NONE',  ( -15.53471296425188442, 34.37731371789854506, -2.908627838312459080 ) ) ;
#8215 = CARTESIAN_POINT ( 'NONE',  ( -37.13169563604516554, 210.1155267958018271, 8.500000000000003553 ) ) ;
#8216 = CARTESIAN_POINT ( 'NONE',  ( -8.715434833791929847, 4.660186282101435928, -8.962234695871762469 ) ) ;
#8217 = CARTESIAN_POINT ( 'NONE',  ( -11.48171059495397373, 50.08518628210144641, -4.944772684328680334 ) ) ;
#8218 = CARTESIAN_POINT ( 'NONE',  ( -11.08355503943142573, 11.56018628210145316, 10.83675517735155402 ) ) ;
#8219 = CARTESIAN_POINT ( 'NONE',  ( 19.56230152254412147, 5.196152422706637353, -1.050000000000023137 ) ) ;
#8220 = CARTESIAN_POINT ( 'NONE',  ( 16.56230152254410726, 0.000000000000000000, -10.00000000000000000 ) ) ;
#8221 = ORIENTED_EDGE ( 'NONE', *, *, #32635, .T. ) ;
#8222 = CARTESIAN_POINT ( 'NONE',  ( -13.23911966647218463, 11.84768628210144747, 8.632099005475506459 ) ) ;
#8223 = CIRCLE ( 'NONE', #7606, 2.649999999999992806 ) ;
#8224 = CARTESIAN_POINT ( 'NONE',  ( -13.62178482187500528, 195.2281250006145399, -23.59362340125807123 ) ) ;
#8225 = CARTESIAN_POINT ( 'NONE',  ( 27.24356964375000345, 197.8343750006145569, -3.336375036156643733E-15 ) ) ;
#8226 = CARTESIAN_POINT ( 'NONE',  ( 27.91448717542667168, 5.196152422706636465, 163.4540897989176642 ) ) ;
#8227 =( NAMED_UNIT ( * ) PLANE_ANGLE_UNIT ( ) SI_UNIT ( $, .RADIAN. ) );
#8228 = LINE ( 'NONE', #10875, #19489 ) ;
#8229 = DIRECTION ( 'NONE',  ( 0.000000000000000000, 0.000000000000000000, 1.000000000000000000 ) ) ;
#8230 = CARTESIAN_POINT ( 'NONE',  ( 18.12178482187499640, 248.4343750006145228, -4.985214923628404904 ) ) ;
#8231 = CARTESIAN_POINT ( 'NONE',  ( 5.529263428287300108, 104.5273137178985650, 7.954856959092309943 ) ) ;
#8232 = CARTESIAN_POINT ( 'NONE',  ( 15.24356964375000167, 241.7968750006145342, 3.323476615752272600 ) ) ;
#8233 = ORIENTED_EDGE ( 'NONE', *, *, #62, .T. ) ;
#8234 = CARTESIAN_POINT ( 'NONE',  ( -69.20163769728823411, 215.6869285224996986, -3.149950860017881382 ) ) ;
#8235 = DIRECTION ( 'NONE',  ( 0.9961946980917462113, 0.000000000000000000, -0.08715574274765118534 ) ) ;
#8236 = EDGE_CURVE ( 'NONE', #3985, #11470, #5445, .T. ) ;
#8237 = CARTESIAN_POINT ( 'NONE',  ( 21.00000000000000000, 248.3687500012290457, 6.928203230275506996 ) ) ;
#8238 = CARTESIAN_POINT ( 'NONE',  ( 2.660918448318003282, 123.5023137178985593, 12.46528703574811558 ) ) ;
#8239 = CARTESIAN_POINT ( 'NONE',  ( 15.47811703177229070, 6.148715791637009431, -10.14010138606053424 ) ) ;
#8240 = CARTESIAN_POINT ( 'NONE',  ( 27.67632261399923976, -5.407089921784859143, 162.1291805290064474 ) ) ;
#8241 = CARTESIAN_POINT ( 'NONE',  ( 26.99999999999999645, 7.347880794884117764E-16, -2.024999999999999023 ) ) ;
#8242 = CARTESIAN_POINT ( 'NONE',  ( 13.62178482187501416, 199.5593750006145513, 23.59362340125806767 ) ) ;
#8243 = VERTEX_POINT ( 'NONE', #13964 ) ;
#8244 = ORIENTED_EDGE ( 'NONE', *, *, #7271, .F. ) ;
#8245 = VERTEX_POINT ( 'NONE', #37432 ) ;
#8246 = CARTESIAN_POINT ( 'NONE',  ( 18.00000000000000355, -5.196152422706632912, -5.268749998770943854 ) ) ;
#8247 = CARTESIAN_POINT ( 'NONE',  ( 26.75643035624999655, 7.049594010296217766E-16, -3.515624999385458249 ) ) ;
#8248 = DIRECTION ( 'NONE',  ( 0.000000000000000000, -0.000000000000000000, 1.000000000000000000 ) ) ;
#8249 = DIRECTION ( 'NONE',  ( 1.000000000000000000, 0.000000000000000000, 0.000000000000000000 ) ) ;
#8250 = CARTESIAN_POINT ( 'NONE',  ( 18.12178482187500350, 249.3718750006145228, 4.985214923628407568 ) ) ;
#8251 = CARTESIAN_POINT ( 'NONE',  ( 0.1745138560725515708, 51.81018628210144783, -12.50000000000000355 ) ) ;
#8252 = CARTESIAN_POINT ( 'NONE',  ( -57.12127896937849414, 216.5309553116392181, 1.626142955000506429 ) ) ;
#8253 = CARTESIAN_POINT ( 'NONE',  ( 14.20575797955546626, 216.7942420204377925, 0.4629122958924736242 ) ) ;
#8254 = CARTESIAN_POINT ( 'NONE',  ( -43.66294563604516554, 213.2096571498974527, -3.378800118222469617 ) ) ;
#8255 = DIRECTION ( 'NONE',  ( 1.000000000000000000, 0.000000000000000000, 0.000000000000000000 ) ) ;
#8256 = CARTESIAN_POINT ( 'NONE',  ( 25.13834520420595098, 0.000000000000000000, 166.1437816049835874 ) ) ;
#8257 = CARTESIAN_POINT ( 'NONE',  ( -0.1745138560722763466, 128.3898137178985621, -12.50000000000000355 ) ) ;
#8258 = CARTESIAN_POINT ( 'NONE',  ( -39.90997103062156270, 215.5714017266979852, 3.350049139982118618 ) ) ;
#8259 = CARTESIAN_POINT ( 'NONE',  ( -49.21205436395490551, 216.1378603801730094, 6.307003348497944195 ) ) ;
#8260 = AXIS2_PLACEMENT_3D ( 'NONE', #19386, #30564, #22590 ) ;
#8261 = CARTESIAN_POINT ( 'NONE',  ( 18.12178482187500350, -4.985214923628407568, -4.678124999385496530 ) ) ;
#8262 = CARTESIAN_POINT ( 'NONE',  ( 13.62178482187499640, 196.9531250006145342, -23.59362340125807123 ) ) ;
#8263 = CARTESIAN_POINT ( 'NONE',  ( 5.770363421894130873, 92.16481371789855359, -14.38691631536193860 ) ) ;
#8264 = CARTESIAN_POINT ( 'NONE',  ( -33.17336230271182984, 215.6869285224997270, 3.149950860017831200 ) ) ;
#8265 = ORIENTED_EDGE ( 'NONE', *, *, #8947, .F. ) ;
#8266 = CARTESIAN_POINT ( 'NONE',  ( -4.622313124798576922, 115.6351862821014578, -11.61527771782819762 ) ) ;
#8267 = CARTESIAN_POINT ( 'NONE',  ( 5.770363421893814682, 55.83518628210145351, 14.38691631536207183 ) ) ;
#8268 = FACE_OUTER_BOUND ( 'NONE', #23646, .T. ) ;
#8269 = CARTESIAN_POINT ( 'NONE',  ( 37.05669835387680422, 3.604726614523243278, 161.8919742727257187 ) ) ;
#8270 = CARTESIAN_POINT ( 'NONE',  ( -15.46528703574804986, 77.39768628210144641, -3.257655550457287497 ) ) ;
#8271 = VECTOR ( 'NONE', #11231, 1000.000000000000000 ) ;
#8272 = CARTESIAN_POINT ( 'NONE',  ( 13.44051670066911619, -5.407089921784859143, -6.815624999385539340 ) ) ;
#8273 = CARTESIAN_POINT ( 'NONE',  ( -2.064181346179269738, 19.89768628210143930, 9.465287035748067623 ) ) ;
#8274 = FACE_OUTER_BOUND ( 'NONE', #335, .T. ) ;
#8275 = CARTESIAN_POINT ( 'NONE',  ( -65.63913769728823411, 206.8500491399821044, -5.686928522499717253 ) ) ;
#8276 = LINE ( 'NONE', #22868, #22656 ) ;
#8277 = CARTESIAN_POINT ( 'NONE',  ( -10.69584247140444866, 57.84768628210144925, 6.932735513423972762 ) ) ;
#8278 = CARTESIAN_POINT ( 'NONE',  ( 5.727106289114498080E-15, 198.7625000000000455, 31.17691453623979214 ) ) ;
#8279 = DIRECTION ( 'NONE',  ( -1.000000000000000000, 0.000000000000000000, 0.000000000000000000 ) ) ;
#8281 = CARTESIAN_POINT ( 'NONE',  ( 22.80587116629411426, 7.646167579472024665E-16, -2.671874999385509319 ) ) ;
#8280 = CARTESIAN_POINT ( 'NONE',  ( -9.500000000000005329, 31.11018628210143433, -0.1745138560725176813 ) ) ;
#8282 = CARTESIAN_POINT ( 'NONE',  ( 26.75643035624999655, 248.7343750006145342, -7.049594010296217766E-16 ) ) ;
#8283 = ORIENTED_EDGE ( 'NONE', *, *, #30986, .T. ) ;
#8284 = CARTESIAN_POINT ( 'NONE',  ( 18.00000000000000000, 5.196152422706630247, -3.675000000000011369 ) ) ;
#8285 = CARTESIAN_POINT ( 'NONE',  ( 34.15639093268026016, -5.196152422706629359, 165.9570967391097440 ) ) ;
#8286 = CARTESIAN_POINT ( 'NONE',  ( 36.93250142046139928, -3.604726614523238837, 160.4723968279449480 ) ) ;
#8287 = CARTESIAN_POINT ( 'NONE',  ( 13.44051670066911441, -5.407089921784859143, -1.865624999385528948 ) ) ;
#8288 = CARTESIAN_POINT ( 'NONE',  ( 27.65301994718372569, -5.196152422706638241, 160.4655057046423678 ) ) ;
#8289 =( BOUNDED_CURVE ( )  B_SPLINE_CURVE ( 2, ( #14465, #47, #22819, #25648, #34368, #11614, #8779, #239, #19980 ),
 .UNSPECIFIED., .F., .F. ) 
 B_SPLINE_CURVE_WITH_KNOTS ( ( 3, 2, 2, 2, 3 ),
 ( 0.3152173913043477826, 0.3188405797101449002, 0.3260869565217391353, 0.3333333333333333148, 0.3369565217391304324 ),
 .UNSPECIFIED. ) 
 CURVE ( )  GEOMETRIC_REPRESENTATION_ITEM ( )  RATIONAL_B_SPLINE_CURVE ( ( 0.9330127018922191873, 0.9330127018922187432, 1.000000000000000000, 0.8660254037844387076, 1.000000000000000000, 0.8660254037844387076, 1.000000000000000000, 0.9330127018922194093, 0.9330127018922194093 ) ) 
 REPRESENTATION_ITEM ( '' )  );
#8290 = CARTESIAN_POINT ( 'NONE',  ( 26.99999999999999645, 242.5750000000000171, -7.347880794884117764E-16 ) ) ;
#8291 = LINE ( 'NONE', #14712, #29370 ) ;
#8292 = CARTESIAN_POINT ( 'NONE',  ( 11.48171059495397728, 63.88518628210145067, 4.944772684328674117 ) ) ;
#8293 = ORIENTED_EDGE ( 'NONE', *, *, #13054, .F. ) ;
#8294 = ORIENTED_EDGE ( 'NONE', *, *, #3854, .T. ) ;
#8295 = CARTESIAN_POINT ( 'NONE',  ( 27.00000000000001066, 195.3500000012290343, 15.58845726811988897 ) ) ;
#8296 = CARTESIAN_POINT ( 'NONE',  ( 15.00000000000000000, 0.000000000000000000, -4.893749998770957177 ) ) ;
#8297 = CARTESIAN_POINT ( 'NONE',  ( 10.83675517735179206, 46.73981371789855643, -11.08355503943118769 ) ) ;
#8298 = CARTESIAN_POINT ( 'NONE',  ( 15.24356964374999990, 3.323476615752268604, -8.390624999385488891 ) ) ;
#8299 = EDGE_CURVE ( 'NONE', #18605, #13555, #34233, .T. ) ;
#8300 = CARTESIAN_POINT ( 'NONE',  ( 18.12178482187499640, 241.6843750006145513, -4.985214923628404904 ) ) ;
#8301 = CARTESIAN_POINT ( 'NONE',  ( -43.86830436395490551, 209.8844732041982297, 4.499999999999996447 ) ) ;
#8302 = VECTOR ( 'NONE', #308, 1000.000000000000000 ) ;
#8303 = CARTESIAN_POINT ( 'NONE',  ( 20.99999999999999289, 240.8874999999999886, -5.999999999999997335 ) ) ;
#8304 = CARTESIAN_POINT ( 'NONE',  ( 27.63220001923324176, -5.407089921784865361, 161.6248569630975283 ) ) ;
#8305 = CARTESIAN_POINT ( 'NONE',  ( 0.1745138560723095977, 31.78981371789855004, 9.500000000000005329 ) ) ;
#8306 = CARTESIAN_POINT ( 'NONE',  ( 37.06653485837505713, 3.464101615138019508, 164.7990542813599006 ) ) ;
#8307 =( BOUNDED_CURVE ( )  B_SPLINE_CURVE ( 2, ( #9977, #3542, #21183, #18721, #21370, #32909, #24573 ),
 .UNSPECIFIED., .F., .F. ) 
 B_SPLINE_CURVE_WITH_KNOTS ( ( 3, 2, 2, 3 ),
 ( 0.7391304347826077592, 0.7463768115942017722, 0.7536231884057958963, 0.7608695652173899093 ),
 .UNSPECIFIED. ) 
 CURVE ( )  GEOMETRIC_REPRESENTATION_ITEM ( )  RATIONAL_B_SPLINE_CURVE ( ( 1.000000000000016431, 0.8660254037844222763, 1.000000000000000000, 0.8660254037844387076, 1.000000000000000000, 0.8660254037844653530, 0.9999999999999733546 ) ) 
 REPRESENTATION_ITEM ( '' )  );
#8308 = CARTESIAN_POINT ( 'NONE',  ( -3.474262827703527901, 96.76481371789854791, 8.843639120294245259 ) ) ;
#8309 = CARTESIAN_POINT ( 'NONE',  ( 27.24356964374999635, 197.4218750006145342, -15.72908226750539029 ) ) ;
#8310 = CARTESIAN_POINT ( 'NONE',  ( 2.660918448318002838, 13.10231371789855004, 12.46528703574811558 ) ) ;
#8311 = EDGE_CURVE ( 'NONE', #5701, #32041, #8276, .T. ) ;
#8312 = CARTESIAN_POINT ( 'NONE',  ( 2.311890736173175753, 65.32268628210144357, 12.53471296425194836 ) ) ;
#8313 = CARTESIAN_POINT ( 'NONE',  ( 19.39230484541326760, 240.6424038105676573, 5.999999999999999112 ) ) ;
#8314 = EDGE_CURVE ( 'NONE', #4722, #22653, #31026, .T. ) ;
#8315 = CARTESIAN_POINT ( 'NONE',  ( 37.02404643378602600, 7.347880794884125653E-16, 164.3134093660401618 ) ) ;
#8316 = CARTESIAN_POINT ( 'NONE',  ( 34.49914238540488043, 5.407089921784862696, 168.4774396467310282 ) ) ;
#8317 = CARTESIAN_POINT ( 'NONE',  ( 22.80587116629411071, 3.604726614523243278, -8.934374999385493510 ) ) ;
#8318 = SURFACE_STYLE_FILL_AREA ( #22728 ) ;
#8319 = CARTESIAN_POINT ( 'NONE',  ( -1.715153634034234598, 79.12268628210145494, -9.534712964251941258 ) ) ;
#8321 = MANIFOLD_SOLID_BREP ( 'Sweep1', #35605 ) ;
#8320 = CYLINDRICAL_SURFACE ( 'NONE', #24338, 6.000000000000001776 ) ;
#8322 = EDGE_CURVE ( 'NONE', #2775, #1851, #21471, .T. ) ;
#8323 = CARTESIAN_POINT ( 'NONE',  ( -7.228626920339069173, 112.4726862821014493, 10.49813415415989581 ) ) ;
#8324 = CARTESIAN_POINT ( 'NONE',  ( 13.49999999999999645, 195.0125000012290570, -23.38268590217984766 ) ) ;
#8325 = CARTESIAN_POINT ( 'NONE',  ( 24.00000000000000000, 248.4062500012290400, 5.196152422706629359 ) ) ;
#8326 = ORIENTED_EDGE ( 'NONE', *, *, #13190, .T. ) ;
#8327 = CARTESIAN_POINT ( 'NONE',  ( 36.97662401522738662, -3.604726614523235284, 160.9767203938538955 ) ) ;
#8328 = CARTESIAN_POINT ( 'NONE',  ( 26.75643035624999655, 7.049594010296217766E-16, -8.015624999385462246 ) ) ;
#8329 = VECTOR ( 'NONE', #20193, 1000.000000000000000 ) ;
#8330 = CARTESIAN_POINT ( 'NONE',  ( -27.24356964374999279, 195.8468750006145740, 15.72908226750539384 ) ) ;
#8331 = CARTESIAN_POINT ( 'NONE',  ( 34.34226204845910502, 5.407089921784862696, 166.6842891901658845 ) ) ;
#8332 = CARTESIAN_POINT ( 'NONE',  ( 37.21687851461520324, -3.464101615137755275, 166.5174901355681527 ) ) ;
#8333 = CARTESIAN_POINT ( 'NONE',  ( 20.99999999999997868, 246.5687500012290343, 5.999999999999999112 ) ) ;
#8334 = CARTESIAN_POINT ( 'NONE',  ( 15.24356964375000167, 239.9968750006145513, 3.323476615752272600 ) ) ;
#8335 = CARTESIAN_POINT ( 'NONE',  ( -27.24356964374999279, 198.4906250006145569, 15.72908226750539384 ) ) ;
#8336 = CARTESIAN_POINT ( 'NONE',  ( 12.50000000000000355, 121.4898137178985564, -0.1745138560722771515 ) ) ;
#8337 = CARTESIAN_POINT ( 'NONE',  ( 11.48171059495397728, 128.2851862821014493, 4.944772684328674117 ) ) ;
#8339 = ORIENTED_EDGE ( 'NONE', *, *, #19918, .F. ) ;
#8338 = EDGE_LOOP ( 'NONE', ( #34435, #30896, #849, #29628 ) ) ;
#8340 = CARTESIAN_POINT ( 'NONE',  ( 23.87821517812499650, 241.9468750006145115, -4.985214923628404904 ) ) ;
#8341 = CARTESIAN_POINT ( 'NONE',  ( 10.49999999999999467, 237.0000000000000000, -2.500000000000000000 ) ) ;
#8342 = CARTESIAN_POINT ( 'NONE',  ( 8.632099005475788900, 101.6523137178985792, -13.23911966647199812 ) ) ;
#8343 = CARTESIAN_POINT ( 'NONE',  ( -2.311890736173176641, 97.52268628210144641, -12.53471296425194836 ) ) ;
#8344 = CARTESIAN_POINT ( 'NONE',  ( 15.24356964374999990, 0.000000000000000000, -2.503124999385486493 ) ) ;
#8345 =( BOUNDED_CURVE ( )  B_SPLINE_CURVE ( 2, ( #26112, #8869, #9060, #6017, #14748, #25743, #6211, #31434, #17601 ),
 .UNSPECIFIED., .F., .F. ) 
 B_SPLINE_CURVE_WITH_KNOTS ( ( 3, 2, 2, 2, 3 ),
 ( 0.03260869565217391908, 0.03623188405797101580, 0.04347826086956521618, 0.05072463768115942351, 0.05434782608695652023 ),
 .UNSPECIFIED. ) 
 CURVE ( )  GEOMETRIC_REPRESENTATION_ITEM ( )  RATIONAL_B_SPLINE_CURVE ( ( 0.9330127018922192983, 0.9330127018922194093, 1.000000000000000000, 0.8660254037844387076, 1.000000000000000000, 0.8660254037844387076, 1.000000000000000000, 0.9330127018922194093, 0.9330127018922191873 ) ) 
 REPRESENTATION_ITEM ( '' )  );
#8346 = CARTESIAN_POINT ( 'NONE',  ( 5.727106289114498080E-15, 199.3250000012290570, 31.17691453623979214 ) ) ;
#8347 = CARTESIAN_POINT ( 'NONE',  ( 4.622313124798573369, 120.2351862821014663, 11.61527771782819940 ) ) ;
#8348 = CARTESIAN_POINT ( 'NONE',  ( 10.31873187879411091, 3.604726614523236616, -2.428124999385521843 ) ) ;
#8349 = EDGE_CURVE ( 'NONE', #36021, #9298, #17086, .T. ) ;
#8350 = CARTESIAN_POINT ( 'NONE',  ( 23.87821517812499650, 245.5468750006145058, -4.985214923628404904 ) ) ;
#8351 = CARTESIAN_POINT ( 'NONE',  ( 10.56230152254328125, -3.464101615137274326, -1.649999998771008114 ) ) ;
#8352 = CARTESIAN_POINT ( 'NONE',  ( -54.54836230271182984, 204.3130714775002446, -3.149950860017828091 ) ) ;
#8353 = CARTESIAN_POINT ( 'NONE',  ( 2.660918448318279950, 116.4976862821014549, -12.46528703574805697 ) ) ;
#8354 = CARTESIAN_POINT ( 'NONE',  ( 22.56230152254411436, -3.464101615137751278, -2.849999998770996967 ) ) ;
#8355 = EDGE_CURVE ( 'NONE', #14365, #16958, #6929, .T. ) ;
#8356 = CARTESIAN_POINT ( 'NONE',  ( -41.88913769728823411, 206.8500491399821044, -5.686928522499717253 ) ) ;
#8357 = CYLINDRICAL_SURFACE ( 'NONE', #36095, 5.999999999999994671 ) ;
#8358 = DIRECTION ( 'NONE',  ( 0.000000000000000000, 0.000000000000000000, -1.000000000000000000 ) ) ;
#8359 = AXIS2_PLACEMENT_3D ( 'NONE', #34142, #22224, #1744 ) ;
#8360 = CARTESIAN_POINT ( 'NONE',  ( 3.257655550457285720, 107.2976862821014521, -15.46528703574804986 ) ) ;
#8361 = CARTESIAN_POINT ( 'NONE',  ( 11.48171059495397728, 8.685186282101437172, 4.944772684328674117 ) ) ;
#8362 = DIRECTION ( 'NONE',  ( -0.9925324990730152175, 0.1219804832088933616, 0.000000000000000000 ) ) ;
#8363 = CARTESIAN_POINT ( 'NONE',  ( -9.500000000000005329, 123.1101862821014663, -0.1745138560725176813 ) ) ;
#8364 = CARTESIAN_POINT ( 'NONE',  ( 13.44051670066911086, 5.407089921784856479, -2.015624999385540406 ) ) ;
#8365 = CARTESIAN_POINT ( 'NONE',  ( 14.99999999999992184, 3.464101615137706425, -4.481249998770945098 ) ) ;
#8366 = ORIENTED_EDGE ( 'NONE', *, *, #26319, .F. ) ;
#8367 = FACE_OUTER_BOUND ( 'NONE', #17324, .T. ) ;
#8368 = CARTESIAN_POINT ( 'NONE',  ( -9.500000000000005329, 58.71018628210145351, -0.1745138560725176813 ) ) ;
#8369 = CARTESIAN_POINT ( 'NONE',  ( 18.12178482187499640, 4.985214923628404904, -0.6656249993854668201 ) ) ;
#8370 = CARTESIAN_POINT ( 'NONE',  ( -13.62178482187498396, 194.9281250006145569, 23.59362340125808188 ) ) ;
#8371 = CARTESIAN_POINT ( 'NONE',  ( 0.000000000000000000, 2.000000000000000000, 0.000000000000000000 ) ) ;
#8372 = CARTESIAN_POINT ( 'NONE',  ( 13.62178482187501416, 195.9593750006145569, 23.59362340125806767 ) ) ;
#8373 = CARTESIAN_POINT ( 'NONE',  ( 36.95541128647934670, 7.347880794884117764E-16, 163.5289060425172636 ) ) ;
#8374 = CARTESIAN_POINT ( 'NONE',  ( 0.1745138560723095977, 31.78981371789855004, 9.500000000000005329 ) ) ;
#8375 = DIRECTION ( 'NONE',  ( -0.000000000000000000, -0.000000000000000000, 1.000000000000000000 ) ) ;
#8376 = CIRCLE ( 'NONE', #34985, 27.00000000000000355 ) ;
#8377 = ORIENTED_EDGE ( 'NONE', *, *, #5296, .F. ) ;
#8378 = CARTESIAN_POINT ( 'NONE',  ( 26.75643035624999655, 249.1093750006145058, -3.323476615752271712 ) ) ;
#8379 = CARTESIAN_POINT ( 'NONE',  ( 8.962234695871567070, 58.23981371789854933, 8.715434833792127023 ) ) ;
#8380 = CARTESIAN_POINT ( 'NONE',  ( 22.80587116629411781, 3.604726614523243278, -8.034374999385502036 ) ) ;
#8381 = CARTESIAN_POINT ( 'NONE',  ( 21.00000000000000000, 6.646953231504538984, -8.915624999385478588 ) ) ;
#8382 = CARTESIAN_POINT ( 'NONE',  ( -12.50000000000000355, 6.489813717898557321, 0.1745138560722786503 ) ) ;
#8383 = ORIENTED_EDGE ( 'NONE', *, *, #24319, .T. ) ;
#8384 = AXIS2_PLACEMENT_3D ( 'NONE', #14201, #25752, #15323 ) ;
#8385 = CARTESIAN_POINT ( 'NONE',  ( 22.80587116629412492, -3.604726614523238837, -0.4593749993855362757 ) ) ;
#8386 = CARTESIAN_POINT ( 'NONE',  ( 2.660918448318279950, 6.097686282101443922, -12.46528703574805697 ) ) ;
#8387 =( BOUNDED_CURVE ( )  B_SPLINE_CURVE ( 2, ( #28360, #25337, #28912, #11305, #11118, #22695, #36885, #19673, #22506, #10931, #5417, #2396, #25519, #16636, #37257, #14518, #17185, #31576, #31761, #16998, #34053, #34239, #20212, #2208, #28538, #13970, #37438, #23240, #31398, #2581, #8282, #28725, #8099, #19855, #11487, #31212, #5241, #23056, #22873, #5599, #14151, #11666, #34424, #8461, #20031, #5791, #34602, #2763, #14335, #8644, #2948, #31032, #26074, #102, #34788, #8832, #5053, #35336, #3321, #12227, #32690, #12607, #17929, #9393, #26440, #15265, #20404, #32500, #26818, #1036, #21153, #23607, #20967, #14892, #23799, #6734, #17741, #31945, #20773, #6546, #35153, #5977, #26252, #9204, #34973, #23990, #17557, #18307, #3883, #15077, #9016, #6167, #3135, #24173, #32129, #29847, #32317, #3509, #20586, #6358, #14703, #847, #35717, #29092, #9579, #287, #15457, #11853, #29473, #29281, #26626, #656, #23422, #472, #18119, #29661, #12040, #27009, #12419, #3697, #35534, #22082, #25096, #36093, #1411, #30039, #27381, #18873, #16023, #33442, #12987, #7119, #36275, #15645, #21529, #10137, #9765, #30422, #6928, #9948, #13169, #4073, #7673, #27572, #24544, #15833, #27195, #35905, #1220, #12793, #21710, #33075, #4257, #32881, #4444, #30792, #7483, #10320, #10504, #33260, #24362, #7299, #36462, #18500, #1601, #18690, #4629, #1970, #24724, #21893, #19061, #30613, #30232, #16209, #27757, #1787, #13355, #24910, #33634, #19252, #4815, #27940, #16395, #13543, #21342, #11437, #31525, #10879, #34553, #11066, #19807, #13737, #25470, #19431, #34371, #2348, #2156, #31712, #5551, #8593, #25285, #13920, #22452, #31342, #37020, #36836, #14468, #22640, #34187, #33999, #25837, #17136, #8043, #5369, #5739, #8232, #16948, #4999, #31165, #28490, #19983, #2534, #22822, #28309, #19619, #25652, #16581, #5188, #14100, #36653, #37205, #33821, #16762, #11252, #30981, #8414, #28672, #2710, #7859, #23004, #14286, #28126, #37385, #20164, #17319, #28861, #22268, #2895, #10690, #12180, #26582, #26773, #11993, #8783, #23565, #11806, #3839, #14847, #31897, #9349, #9158, #26395, #428, #20541, #23754, #5926, #6113, #20920, #20355 ),
 .UNSPECIFIED., .F., .F. ) 
 B_SPLINE_CURVE_WITH_KNOTS ( ( 3, 2, 2, 2, 2, 2, 2, 2, 2, 2, 2, 2, 2, 2, 2, 2, 2, 2, 2, 2, 2, 2, 2, 2, 2, 2, 2, 2, 2, 2, 2, 2, 2, 2, 2, 2, 2, 2, 2, 2, 2, 2, 2, 2, 2, 2, 2, 2, 2, 2, 2, 2, 2, 2, 2, 2, 2, 2, 2, 2, 2, 2, 2, 2, 2, 2, 2, 2, 2, 2, 2, 2, 2, 2, 2, 2, 2, 2, 2, 2, 2, 2, 2, 2, 2, 2, 2, 2, 2, 2, 2, 2, 2, 2, 2, 2, 2, 2, 2, 2, 2, 2, 2, 2, 2, 2, 2, 2, 2, 2, 2, 2, 2, 2, 2, 2, 2, 2, 2, 2, 2, 2, 2, 2, 2, 2, 2, 2, 2, 2, 2, 2, 2, 2, 3 ),
 ( 0.000000000000000000, 0.007246376811594202987, 0.01449275362318840597, 0.02173913043478260809, 0.02898550724637681195, 0.03623188405797101580, 0.04347826086956521618, 0.05072463768115942351, 0.05797101449275362389, 0.06521739130434782428, 0.07246376811594203160, 0.07971014492753622505, 0.08695652173913043237, 0.09420289855072463969, 0.1014492753623188470, 0.1086956521739130405, 0.1159420289855072478, 0.1231884057971014412, 0.1304347826086956486, 0.1376811594202898559, 0.1449275362318840632, 0.1521739130434782705, 0.1594202898550724501, 0.1666666666666666574, 0.1739130434782608647, 0.1811594202898550721, 0.1884057971014492794, 0.1956521739130434867, 0.2028985507246376940, 0.2101449275362318736, 0.2173913043478260809, 0.2246376811594202882, 0.2318840579710144956, 0.2391304347826087306, 0.2463768115942028825, 0.2536231884057971175, 0.2608695652173912971, 0.2681159420289855322, 0.2753623188405797118, 0.2826086956521738913, 0.2898550724637681264, 0.2971014492753623060, 0.3043478260869565410, 0.3115942028985507206, 0.3188405797101449002, 0.3260869565217391353, 0.3333333333333333148, 0.3405797101449275499, 0.3478260869565217295, 0.3550724637681159646, 0.3623188405797101441, 0.3695652173913043237, 0.3768115942028985588, 0.3840579710144927383, 0.3913043478260869734, 0.3985507246376811530, 0.4057971014492753881, 0.4130434782608695676, 0.4202898550724637472, 0.4275362318840579823, 0.4347826086956521618, 0.4420289855072463969, 0.4492753623188405765, 0.4565217391304347561, 0.4637681159420289911, 0.4710144927536231707, 0.4782608695652174613, 0.4855072463768115854, 0.4927536231884057649, 0.5000000000000000000, 0.5072463768115942351, 0.5144927536231883591, 0.5217391304347825942, 0.5289855072463768293, 0.5362318840579710644, 0.5434782608695651884, 0.5507246376811594235, 0.5579710144927536586, 0.5652173913043477826, 0.5724637681159420177, 0.5797101449275362528, 0.5869565217391304879, 0.5942028985507246119, 0.6014492753623188470, 0.6086956521739130821, 0.6159420289855072062, 0.6231884057971014412, 0.6304347826086956763, 0.6376811594202898004, 0.6449275362318840354, 0.6521739130434782705, 0.6594202898550725056, 0.6666666666666666297, 0.6739130434782608647, 0.6811594202898550998, 0.6884057971014492239, 0.6956521739130434590, 0.7028985507246376940, 0.7101449275362319291, 0.7173913043478260532, 0.7246376811594202882, 0.7318840579710145233, 0.7391304347826086474, 0.7463768115942028825, 0.7536231884057971175, 0.7608695652173913526, 0.7681159420289854767, 0.7753623188405797118, 0.7826086956521739468, 0.7898550724637680709, 0.7971014492753623060, 0.8043478260869565410, 0.8115942028985507761, 0.8188405797101449002, 0.8260869565217391353, 0.8333333333333333703, 0.8405797101449274944, 0.8478260869565217295, 0.8550724637681159646, 0.8623188405797101996, 0.8695652173913043237, 0.8768115942028985588, 0.8840579710144927938, 0.8913043478260869179, 0.8985507246376811530, 0.9057971014492753881, 0.9130434782608695121, 0.9202898550724637472, 0.9275362318840579823, 0.9347826086956522174, 0.9420289855072463414, 0.9492753623188405765, 0.9565217391304349226, 0.9637681159420289356, 0.9662082973083875315 ),
 .UNSPECIFIED. ) 
 CURVE ( )  GEOMETRIC_REPRESENTATION_ITEM ( )  RATIONAL_B_SPLINE_CURVE ( ( 1.000000000000000000, 0.8660254037844387076, 1.000000000000000000, 0.8660254037844387076, 1.000000000000000000, 0.8660254037844387076, 1.000000000000000000, 0.8660254037844387076, 1.000000000000000000, 0.8660254037844387076, 1.000000000000000000, 0.8660254037844387076, 1.000000000000000000, 0.8660254037844387076, 1.000000000000000000, 0.8660254037844387076, 1.000000000000000000, 0.8660254037844387076, 1.000000000000000000, 0.8660254037844387076, 1.000000000000000000, 0.8660254037844387076, 1.000000000000000000, 0.8660254037844387076, 1.000000000000000000, 0.8660254037844387076, 1.000000000000000000, 0.8660254037844387076, 1.000000000000000000, 0.8660254037844387076, 1.000000000000000000, 0.8660254037844387076, 1.000000000000000000, 0.8660254037844387076, 1.000000000000000000, 0.8660254037844387076, 1.000000000000000000, 0.8660254037844387076, 1.000000000000000000, 0.8660254037844387076, 1.000000000000000000, 0.8660254037844387076, 1.000000000000000000, 0.8660254037844387076, 1.000000000000000000, 0.8660254037844387076, 1.000000000000000000, 0.8660254037844387076, 1.000000000000000000, 0.8660254037844387076, 1.000000000000000000, 0.8660254037844387076, 1.000000000000000000, 0.8660254037844387076, 1.000000000000000000, 0.8660254037844387076, 1.000000000000000000, 0.8660254037844387076, 1.000000000000000000, 0.8660254037844387076, 1.000000000000000000, 0.8660254037844387076, 1.000000000000000000, 0.8660254037844387076, 1.000000000000000000, 0.8660254037844387076, 1.000000000000000000, 0.8660254037844387076, 1.000000000000000000, 0.8660254037844387076, 1.000000000000000000, 0.8660254037844387076, 1.000000000000000000, 0.8660254037844387076, 1.000000000000000000, 0.8660254037844387076, 1.000000000000000000, 0.8660254037844387076, 1.000000000000000000, 0.8660254037844387076, 1.000000000000000000, 0.8660254037844387076, 1.000000000000000000, 0.8660254037844387076, 1.000000000000000000, 0.8660254037844387076, 1.000000000000000000, 0.8660254037844387076, 1.000000000000000000, 0.8660254037844387076, 1.000000000000000000, 0.8660254037844387076, 1.000000000000000000, 0.8660254037844387076, 1.000000000000000000, 0.8660254037844387076, 1.000000000000000000, 0.8660254037844387076, 1.000000000000000000, 0.8660254037844387076, 1.000000000000000000, 0.8660254037844387076, 1.000000000000000000, 0.8660254037844387076, 1.000000000000000000, 0.8660254037844387076, 1.000000000000000000, 0.8660254037844387076, 1.000000000000000000, 0.8660254037844387076, 1.000000000000000000, 0.8660254037844387076, 1.000000000000000000, 0.8660254037844387076, 1.000000000000000000, 0.8660254037844387076, 1.000000000000000000, 0.8660254037844387076, 1.000000000000000000, 0.8660254037844387076, 1.000000000000000000, 0.8660254037844387076, 1.000000000000000000, 0.8660254037844387076, 1.000000000000000000, 0.8660254037844387076, 1.000000000000000000, 0.8660254037844387076, 1.000000000000000000, 0.8660254037844387076, 1.000000000000000000, 0.8660254037844387076, 1.000000000000000000, 0.8660254037844387076, 1.000000000000000000, 0.8660254037844387076, 1.000000000000000000, 0.8660254037844387076, 1.000000000000000000, 0.8660254037844387076, 1.000000000000000000, 0.8660254037844387076, 1.000000000000000000, 0.8660254037844387076, 1.000000000000000000, 0.8660254037844387076, 1.000000000000000000, 0.8660254037844387076, 1.000000000000000000, 0.8660254037844387076, 1.000000000000000000, 0.8660254037844387076, 1.000000000000000000, 0.8660254037844387076, 1.000000000000000000, 0.8660254037844387076, 1.000000000000000000, 0.8660254037844387076, 1.000000000000000000, 0.8660254037844387076, 1.000000000000000000, 0.8660254037844387076, 1.000000000000000000, 0.8660254037844387076, 1.000000000000000000, 0.8660254037844387076, 1.000000000000000000, 0.8660254037844387076, 1.000000000000000000, 0.8660254037844387076, 1.000000000000000000, 0.8660254037844387076, 1.000000000000000000, 0.8660254037844387076, 1.000000000000000000, 0.8660254037844387076, 1.000000000000000000, 0.8660254037844387076, 1.000000000000000000, 0.8660254037844387076, 1.000000000000000000, 0.8660254037844387076, 1.000000000000000000, 0.8660254037844387076, 1.000000000000000000, 0.8660254037844387076, 1.000000000000000000, 0.8660254037844387076, 1.000000000000000000, 0.8660254037844387076, 1.000000000000000000, 0.8660254037844387076, 1.000000000000000000, 0.8660254037844387076, 1.000000000000000000, 0.8660254037844387076, 1.000000000000000000, 0.8660254037844387076, 1.000000000000000000, 0.8660254037844387076, 1.000000000000000000, 0.8660254037844387076, 1.000000000000000000, 0.8660254037844387076, 1.000000000000000000, 0.8660254037844387076, 1.000000000000000000, 0.8660254037844387076, 1.000000000000000000, 0.8660254037844387076, 1.000000000000000000, 0.8660254037844387076, 1.000000000000000000, 0.8660254037844387076, 1.000000000000000000, 0.8660254037844387076, 1.000000000000000000, 0.8660254037844387076, 1.000000000000000000, 0.8660254037844387076, 1.000000000000000000, 0.8660254037844387076, 1.000000000000000000, 0.8660254037844387076, 1.000000000000000000, 0.8660254037844387076, 1.000000000000000000, 0.8660254037844387076, 1.000000000000000000, 0.8660254037844387076, 1.000000000000000000, 0.8660254037844387076, 1.000000000000000000, 0.8660254037844387076, 1.000000000000000000, 0.8660254037844387076, 1.000000000000000000, 0.8660254037844387076, 1.000000000000000000, 0.8660254037844387076, 1.000000000000000000, 0.8660254037844387076, 1.000000000000000000, 0.8660254037844387076, 1.000000000000000000, 0.8660254037844387076, 1.000000000000000000, 0.8660254037844387076, 1.000000000000000000, 0.8660254037844387076, 1.000000000000000000, 0.8660254037844387076, 1.000000000000000000, 0.8660254037844387076, 1.000000000000000000, 0.8660254037844387076, 1.000000000000000000, 0.8660254037844387076, 1.000000000000000000, 0.8660254037844387076, 1.000000000000000000, 0.8660254037844387076, 1.000000000000000000, 0.8660254037844387076, 1.000000000000000000, 0.8660254037844387076, 1.000000000000000000, 0.9548847207714133978, 0.9401541335272454170 ) ) 
 REPRESENTATION_ITEM ( '' )  );
#8388 = CARTESIAN_POINT ( 'NONE',  ( 28.01132750018552287, 5.407089921784862696, 165.9583038997966185 ) ) ;
#8389 = CARTESIAN_POINT ( 'NONE',  ( -48.61086230271182984, 213.1499508600178387, -5.686928522499747451 ) ) ;
#8390 = CARTESIAN_POINT ( 'NONE',  ( 24.70692427760507570, 0.000000000000000000, 161.2126178494294493 ) ) ;
#8391 = CARTESIAN_POINT ( 'NONE',  ( -1.045839947578415010E-13, 196.5125000000000455, 27.00000000000000355 ) ) ;
#8392 = CARTESIAN_POINT ( 'NONE',  ( -39.51413769728823411, 212.1499508600178387, 3.954877714930865817 ) ) ;
#8393 = CARTESIAN_POINT ( 'NONE',  ( -45.45163769728822700, 215.6869285224996986, -3.149950860017881382 ) ) ;
#8394 = CARTESIAN_POINT ( 'NONE',  ( 37.61068204371655099, 3.604726614523238837, 168.2240368224713620 ) ) ;
#8395 = VERTEX_POINT ( 'NONE', #2017 ) ;
#8396 = VECTOR ( 'NONE', #24396, 1000.000000000000000 ) ;
#8397 = DIRECTION ( 'NONE',  ( 0.000000000000000000, 0.000000000000000000, 1.000000000000000000 ) ) ;
#8398 = CARTESIAN_POINT ( 'NONE',  ( 37.25936693920468201, 7.347880794884125653E-16, 167.0031350508878631 ) ) ;
#8399 = CARTESIAN_POINT ( 'NONE',  ( -3.257655550456946880, 17.70231371789854435, -15.46528703574811736 ) ) ;
#8400 = CARTESIAN_POINT ( 'NONE',  ( -32.77752896937849414, 214.3500491399821897, 7.303452534266821949 ) ) ;
#8401 = CARTESIAN_POINT ( 'NONE',  ( -2.311890736173176641, 5.522686282101451738, -12.53471296425194836 ) ) ;
#8402 = CARTESIAN_POINT ( 'NONE',  ( -10.69584247140444866, 48.64768628210144641, 6.932735513423972762 ) ) ;
#8403 = CARTESIAN_POINT ( 'NONE',  ( 22.56230152254412857, -3.464101615137755275, -3.412500000000044942 ) ) ;
#8404 = SHAPE_REPRESENTATION ( 'follower', ( #17215 ), #5638 ) ;
#8405 = ORIENTED_EDGE ( 'NONE', *, *, #15976, .T. ) ;
#8406 = CARTESIAN_POINT ( 'NONE',  ( -11.08355503943142573, 20.76018628210144001, 10.83675517735155402 ) ) ;
#8407 = CARTESIAN_POINT ( 'NONE',  ( -27.00000000000000355, 196.0625000012290400, 0.000000000000000000 ) ) ;
#8408 = CARTESIAN_POINT ( 'NONE',  ( -20.86978604919638869, 194.8588513911398081, -17.51182792271053046 ) ) ;
#8409 = CARTESIAN_POINT ( 'NONE',  ( -27.00000000000000355, 199.0625000000000000, -15.58845726811989429 ) ) ;
#8410 = CARTESIAN_POINT ( 'NONE',  ( 27.00000000000063238, 3.464101615137388013, -5.531249998770964460 ) ) ;
#8411 = DIRECTION ( 'NONE',  ( -1.558072081575740353E-16, -1.134704379232807653E-16, -1.000000000000000000 ) ) ;
#8412 = CARTESIAN_POINT ( 'NONE',  ( 26.75643035624999655, 244.1968750006145399, 3.323476615752267715 ) ) ;
#8413 = CARTESIAN_POINT ( 'NONE',  ( -0.1745138560723084320, 100.7898137178985536, -9.500000000000005329 ) ) ;
#8414 = CARTESIAN_POINT ( 'NONE',  ( 26.75643035624999655, 241.0468750006145342, 3.323476615752267271 ) ) ;
#8415 = VERTEX_POINT ( 'NONE', #4862 ) ;
#8416 = CARTESIAN_POINT ( 'NONE',  ( -65.44122103062157692, 208.3738570449993404, -6.530955311639226935 ) ) ;
#8417 = CARTESIAN_POINT ( 'NONE',  ( 23.99999999999999645, 249.0062500012290627, -5.196152422706631135 ) ) ;
#8418 = ORIENTED_EDGE ( 'NONE', *, *, #18682, .F. ) ;
#8419 = CARTESIAN_POINT ( 'NONE',  ( 8.962234695871567070, 113.4398137178985593, 8.715434833792127023 ) ) ;
#8420 = CARTESIAN_POINT ( 'NONE',  ( 22.80587116629412847, -3.604726614523238837, -2.259374999385487026 ) ) ;
#8421 = CARTESIAN_POINT ( 'NONE',  ( 27.70246933682352974, 5.407089921784856479, 162.4280389384339855 ) ) ;
#8422 = CARTESIAN_POINT ( 'NONE',  ( 15.24356964374999990, 3.323476615752268604, -1.190624999385493377 ) ) ;
#8423 = CARTESIAN_POINT ( 'NONE',  ( 5.778771075727756162E-15, 199.5218750006145854, 31.45816453501075927 ) ) ;
#8424 = EDGE_CURVE ( 'NONE', #15950, #113, #8156, .T. ) ;
#8425 = ORIENTED_EDGE ( 'NONE', *, *, #25413, .T. ) ;
#8426 = ORIENTED_EDGE ( 'NONE', *, *, #9103, .F. ) ;
#8427 = VERTEX_POINT ( 'NONE', #13783 ) ;
#8428 = CARTESIAN_POINT ( 'NONE',  ( 21.00000000000000000, 6.928203230275506996, -6.806249998770949716 ) ) ;
#8429 = CARTESIAN_POINT ( 'NONE',  ( 18.12178482187500350, -4.985214923628407568, -1.865624999385473437 ) ) ;
#8430 = CARTESIAN_POINT ( 'NONE',  ( 20.99999999999999645, 185.0294372515228645, 0.000000000000000000 ) ) ;
#8431 = CARTESIAN_POINT ( 'NONE',  ( 15.24356964374999990, 0.000000000000000000, -10.04062499938546082 ) ) ;
#8432 = CARTESIAN_POINT ( 'NONE',  ( 8.962234695871762469, 52.96018628210144641, -8.715434833791931624 ) ) ;
#8433 = CARTESIAN_POINT ( 'NONE',  ( -52.56919563604516554, 216.5000000000000000, -0.1155267958017906493 ) ) ;
#8434 = CARTESIAN_POINT ( 'NONE',  ( 6.642437016335149380, 215.3840861188750750, -2.655215585727014993 ) ) ;
#8435 = CARTESIAN_POINT ( 'NONE',  ( -48.21502896937850124, 213.8393509191290889, -2.350049139982142155 ) ) ;
#8436 = CARTESIAN_POINT ( 'NONE',  ( 27.97658564224149558, -5.196152422706632912, 164.1638785225323431 ) ) ;
#8437 = CARTESIAN_POINT ( 'NONE',  ( -12.46528703574811558, 107.4023137178985650, 2.660918448318003726 ) ) ;
#8438 = CARTESIAN_POINT ( 'NONE',  ( -69.00372103062157692, 214.5309553116392749, -1.090244570138262148 ) ) ;
#8439 = CARTESIAN_POINT ( 'NONE',  ( -47.62872103062157692, 201.4690446883607819, 2.162041339862843525 ) ) ;
#8440 = EDGE_CURVE ( 'NONE', #28968, #12845, #25513, .T. ) ;
#8441 = CARTESIAN_POINT ( 'NONE',  ( 23.87821517812500005, -4.985214923628404016, -4.153124999385471305 ) ) ;
#8442 = CARTESIAN_POINT ( 'NONE',  ( -13.62178482187498396, 194.9281250006145569, 23.59362340125808188 ) ) ;
#8443 = CARTESIAN_POINT ( 'NONE',  ( 3.257655550456945548, 68.30231371789852801, 15.46528703574811736 ) ) ;
#8444 = CARTESIAN_POINT ( 'NONE',  ( -34.16294563604515133, 214.6737587650350747, -4.842901733360249317 ) ) ;
#8445 = VERTEX_POINT ( 'NONE', #36879 ) ;
#8446 = CARTESIAN_POINT ( 'NONE',  ( -47.00000000000000711, 244.5000000000000000, -2.499999999999997780 ) ) ;
#8447 = CARTESIAN_POINT ( 'NONE',  ( 0.1745138560725515708, 97.81018628210144072, -12.50000000000000355 ) ) ;
#8448 = CARTESIAN_POINT ( 'NONE',  ( 11.08355503943142750, 71.36018628210143788, -10.83675517735155225 ) ) ;
#8449 = EDGE_CURVE ( 'NONE', #25376, #23017, #10323, .T. ) ;
#8450 = CARTESIAN_POINT ( 'NONE',  ( 15.00000000000000178, 243.2874999999999943, 3.464101615137757051 ) ) ;
#8451 = CARTESIAN_POINT ( 'NONE',  ( 27.67142010346968561, -5.407089921784865361, 162.0731445772388213 ) ) ;
#8452 = CARTESIAN_POINT ( 'NONE',  ( 3.257655550457285720, 61.29768628210142367, -15.46528703574804986 ) ) ;
#8453 = CARTESIAN_POINT ( 'NONE',  ( 13.44051670066911264, 5.407089921784856479, -5.615624999385532057 ) ) ;
#8454 = DIRECTION ( 'NONE',  ( -0.000000000000000000, -1.000000000000000000, -0.000000000000000000 ) ) ;
#8455 = CARTESIAN_POINT ( 'NONE',  ( -65.24330436395489130, 210.1155267958017134, -6.500000000000000888 ) ) ;
#8456 = SURFACE_STYLE_USAGE ( .BOTH. , #19299 ) ;
#8457 = CARTESIAN_POINT ( 'NONE',  ( 11.48171059495397728, 36.28518628210144925, 4.944772684328674117 ) ) ;
#8458 = CARTESIAN_POINT ( 'NONE',  ( -13.49999999999998401, 198.2750000000000057, 23.38268590217985476 ) ) ;
#8459 = LINE ( 'NONE', #34422, #29898 ) ;
#8460 = CARTESIAN_POINT ( 'NONE',  ( -8.710071997420127943, 31.68518628210144428, -3.796722387233380402 ) ) ;
#8461 = CARTESIAN_POINT ( 'NONE',  ( 26.75643035624999655, 248.2468750006145797, 3.323476615752267271 ) ) ;
#8462 = ORIENTED_EDGE ( 'NONE', *, *, #35322, .F. ) ;
#8463 = CARTESIAN_POINT ( 'NONE',  ( 26.99999999999999645, -3.464101615137751278, -4.312500000000005329 ) ) ;
#8464 = DIRECTION ( 'NONE',  ( -0.000000000000000000, -0.000000000000000000, 1.000000000000000000 ) ) ;
#8465 = CARTESIAN_POINT ( 'NONE',  ( 33.78010750773675852, -5.407089921784861808, 160.2588333874741124 ) ) ;
#8466 = CARTESIAN_POINT ( 'NONE',  ( 22.80587116629410716, 3.604726614523238837, -3.028124999385537475 ) ) ;
#8467 = CARTESIAN_POINT ( 'NONE',  ( 31.31896757967941625, 7.209453229046475009, 167.9463391462434174 ) ) ;
#8468 = CARTESIAN_POINT ( 'NONE',  ( 18.00000000000000355, 244.2249999999999943, 5.196152422706632912 ) ) ;
#8469 = FACE_OUTER_BOUND ( 'NONE', #34614, .T. ) ;
#8470 = CARTESIAN_POINT ( 'NONE',  ( 10.69584247140445221, 62.44768628210145778, -6.932735513423970097 ) ) ;
#8471 = ORIENTED_EDGE ( 'NONE', *, *, #22948, .F. ) ;
#8472 = ORIENTED_EDGE ( 'NONE', *, *, #19639, .T. ) ;
#8473 = DIRECTION ( 'NONE',  ( 0.08715574274765150453, 0.000000000000000000, 0.9961946980917461003 ) ) ;
#8474 = CARTESIAN_POINT ( 'NONE',  ( 27.00000000000001066, 196.7000000012290286, 15.58845726811988897 ) ) ;
#8475 = CARTESIAN_POINT ( 'NONE',  ( 1.069080835302379631E-14, 196.6250000012290400, 27.00000000000000000 ) ) ;
#8476 = AXIS2_PLACEMENT_3D ( 'NONE', #26202, #26019, #17315 ) ;
#8477 = EDGE_CURVE ( 'NONE', #21699, #31946, #11872, .T. ) ;
#8478 = CARTESIAN_POINT ( 'NONE',  ( -15.50000000000000533, 43.28981371789856070, 0.1745138560722471477 ) ) ;
#8479 = CARTESIAN_POINT ( 'NONE',  ( 15.24356964374999990, 0.000000000000000000, -9.253124999385493155 ) ) ;
#8480 = CARTESIAN_POINT ( 'NONE',  ( 26.75643035624999655, 243.2968750006145342, 3.323476615752267715 ) ) ;
#8481 = CARTESIAN_POINT ( 'NONE',  ( -42.48288769728823411, 205.5309553116392465, -1.321298161741839117 ) ) ;
#8482 = CYLINDRICAL_SURFACE ( 'NONE', #35502, 3.500000000000003109 ) ;
#8483 = CARTESIAN_POINT ( 'NONE',  ( 30.72576380560321851, 7.209453229046482114, 161.1659889823564811 ) ) ;
#8484 = CARTESIAN_POINT ( 'NONE',  ( -1.715153634034442431, 13.67731371789853867, 9.534712964251900402 ) ) ;
#8485 = EDGE_CURVE ( 'NONE', #18678, #24310, #356, .T. ) ;
#8486 = CARTESIAN_POINT ( 'NONE',  ( -69.00372103062157692, 216.5309553116391612, -1.626142955000564383 ) ) ;
#8487 = DIRECTION ( 'NONE',  ( 0.000000000000000000, 0.000000000000000000, 1.000000000000000000 ) ) ;
#8488 = AXIS2_PLACEMENT_3D ( 'NONE', #19193, #24858, #36222 ) ;
#8489 = CARTESIAN_POINT ( 'NONE',  ( 26.23080272481033148, 195.0000000000000568, 6.985708249719166041 ) ) ;
#8490 = CARTESIAN_POINT ( 'NONE',  ( -27.24356964374999990, 195.3218750006145399, -15.72908226750537786 ) ) ;
#8491 = CARTESIAN_POINT ( 'NONE',  ( 8.962234695871567070, 12.23981371789853512, 8.715434833792127023 ) ) ;
#8492 = EDGE_CURVE ( 'NONE', #805, #407, #14210, .T. ) ;
#8493 = ORIENTED_EDGE ( 'NONE', *, *, #27064, .F. ) ;
#8494 = CARTESIAN_POINT ( 'NONE',  ( 7.228626920339068285, 71.07268628210144357, -10.49813415415989581 ) ) ;
#8495 = CARTESIAN_POINT ( 'NONE',  ( 10.56230152254410726, 0.000000000000000000, -7.087499998771007448 ) ) ;
#8496 = CARTESIAN_POINT ( 'NONE',  ( -44.35000000000001563, 244.5000000000000000, -0.4999999999999982792 ) ) ;
#8497 = CARTESIAN_POINT ( 'NONE',  ( 30.59339602130522096, -7.209453229046475009, 159.6530182846296384 ) ) ;
#8498 = CARTESIAN_POINT ( 'NONE',  ( 18.00000000000000355, -5.196152422706632912, -3.468749998770948029 ) ) ;
#8499 = CARTESIAN_POINT ( 'NONE',  ( 22.80587116629412492, 3.604726614523243278, -8.484374999385497773 ) ) ;
#8500 = CARTESIAN_POINT ( 'NONE',  ( -26.99999999999999645, 197.0000000012290116, 15.58845726811991561 ) ) ;
#8501 = AXIS2_PLACEMENT_3D ( 'NONE', #19783, #13896, #30589 ) ;
#8502 =( BOUNDED_CURVE ( )  B_SPLINE_CURVE ( 2, ( #37494, #5664, #3525, #31635, #29487, #8523, #15090, #34660, #12433 ),
 .UNSPECIFIED., .F., .F. ) 
 B_SPLINE_CURVE_WITH_KNOTS ( ( 3, 2, 2, 2, 3 ),
 ( 0.5978260869565217295, 0.6014492753623188470, 0.6086956521739130821, 0.6159420289855072062, 0.6195652173913043237 ),
 .UNSPECIFIED. ) 
 CURVE ( )  GEOMETRIC_REPRESENTATION_ITEM ( )  RATIONAL_B_SPLINE_CURVE ( ( 0.9330127018922194093, 0.9330127018922194093, 1.000000000000000000, 0.8660254037844387076, 1.000000000000000000, 0.8660254037844387076, 1.000000000000000000, 0.9330127018922194093, 0.9330127018922194093 ) ) 
 REPRESENTATION_ITEM ( '' )  );
#8503 = CARTESIAN_POINT ( 'NONE',  ( -8.843639120294326972, 76.53518628210146346, 3.474262827703335166 ) ) ;
#8504 = DIRECTION ( 'NONE',  ( 0.000000000000000000, 0.000000000000000000, -1.000000000000000000 ) ) ;
#8505 = EDGE_CURVE ( 'NONE', #23955, #22812, #12990, .T. ) ;
#8506 = CARTESIAN_POINT ( 'NONE',  ( -0.1745138560725500443, 120.8101862821014691, 12.50000000000000355 ) ) ;
#8507 = DIRECTION ( 'NONE',  ( -1.000000000000000000, 0.000000000000000000, 0.000000000000000000 ) ) ;
#8508 = ORIENTED_EDGE ( 'NONE', *, *, #23537, .T. ) ;
#8509 = CARTESIAN_POINT ( 'NONE',  ( 37.06160086440634416, 3.604726614523238837, 161.9480102244933732 ) ) ;
#8510 = CARTESIAN_POINT ( 'NONE',  ( 26.75643035624999655, 3.323476615752271712, -7.978124999385458160 ) ) ;
#8511 = CARTESIAN_POINT ( 'NONE',  ( -27.24356964375000345, 196.2593750006145399, 0.000000000000000000 ) ) ;
#8512 = CARTESIAN_POINT ( 'NONE',  ( 37.48158259977161322, -3.604726614523238837, 166.7484234259230220 ) ) ;
#8513 = CARTESIAN_POINT ( 'NONE',  ( 37.10575494261194507, 3.464101615137759271, 165.2473418955011937 ) ) ;
#8514 = CARTESIAN_POINT ( 'NONE',  ( 20.99999999999999645, 185.0294372515228645, 0.000000000000000000 ) ) ;
#8515 = CARTESIAN_POINT ( 'NONE',  ( 26.75643035624999655, 240.1843750006145513, -7.049594010296217766E-16 ) ) ;
#8516 = CARTESIAN_POINT ( 'NONE',  ( 13.62178482187499640, 198.3031250006145285, -23.59362340125807123 ) ) ;
#8517 = CARTESIAN_POINT ( 'NONE',  ( -11.48171059495408208, 116.3148137178985593, 4.944772684328421875 ) ) ;
#8518 = CARTESIAN_POINT ( 'NONE',  ( 8.962234695871762469, 126.5601862821014691, -8.715434833791931624 ) ) ;
#8520 = ORIENTED_EDGE ( 'NONE', *, *, #36496, .T. ) ;
#8519 = ORIENTED_EDGE ( 'NONE', *, *, #20040, .F. ) ;
#8521 = CARTESIAN_POINT ( 'NONE',  ( -27.24356964375000345, 197.5531250006145285, 0.000000000000000000 ) ) ;
#8522 = CARTESIAN_POINT ( 'NONE',  ( 15.24356964375000167, 241.6843750006144944, 3.323476615752272600 ) ) ;
#8523 = CARTESIAN_POINT ( 'NONE',  ( 15.00000000000000000, 243.6625000000000227, -3.464101615137752610 ) ) ;
#8524 = EDGE_CURVE ( 'NONE', #30424, #23066, #282, .T. ) ;
#8525 = CARTESIAN_POINT ( 'NONE',  ( 6.092822981423662299, 95.61481371789857064, 14.25334919248795096 ) ) ;
#8526 = CARTESIAN_POINT ( 'NONE',  ( 6.932735513423970097, 101.5476862821014379, 10.69584247140445044 ) ) ;
#8527 = CARTESIAN_POINT ( 'NONE',  ( 15.24356964374999990, 3.323476615752268604, -2.540624999385480809 ) ) ;
#8528 = CARTESIAN_POINT ( 'NONE',  ( 13.50000000000001421, 196.2125000012290172, 23.38268590217984055 ) ) ;
#8529 = CARTESIAN_POINT ( 'NONE',  ( 9.534712964251900402, 75.77731371789855075, 1.715153634034445540 ) ) ;
#8530 = CARTESIAN_POINT ( 'NONE',  ( 10.31873187879410381, 3.604726614523236616, -2.878124999385517135 ) ) ;
#8531 = CARTESIAN_POINT ( 'NONE',  ( 18.12178482187500350, 242.6218750006145228, 4.985214923628407568 ) ) ;
#8532 = CARTESIAN_POINT ( 'NONE',  ( 22.60769515458672174, 246.5888461906613998, 6.000000000000004441 ) ) ;
#8533 = CARTESIAN_POINT ( 'NONE',  ( 7.228626920339068285, 126.2726862821014606, -10.49813415415989581 ) ) ;
#8534 = CARTESIAN_POINT ( 'NONE',  ( 22.56230152254410370, 3.464101615137755275, -4.124999998771022192 ) ) ;
#8535 = CARTESIAN_POINT ( 'NONE',  ( -43.07663769728823411, 204.3130714775002730, 3.149950860017883603 ) ) ;
#8536 = CARTESIAN_POINT ( 'NONE',  ( 2.999999999999997335, 252.0000000000000000, 5.000000000000000000 ) ) ;
#8537 = VECTOR ( 'NONE', #8473, 1000.000000000000000 ) ;
#8538 = CARTESIAN_POINT ( 'NONE',  ( 18.00000000000000000, 240.9812500012290570, -5.196152422706630247 ) ) ;
#8539 = CARTESIAN_POINT ( 'NONE',  ( 2.908627838312118019, 102.1226862821014549, 15.53471296425195369 ) ) ;
#8540 = CARTESIAN_POINT ( 'NONE',  ( -2.660918448318275509, 19.89768628210143575, 12.46528703574805874 ) ) ;
#8541 = CARTESIAN_POINT ( 'NONE',  ( -20.72401335767156638, 195.0000000000000000, -17.30627455141886983 ) ) ;
#8542 = CARTESIAN_POINT ( 'NONE',  ( 22.60769515458671108, 244.3388461906613429, 6.000000000000010658 ) ) ;
#8543 = CARTESIAN_POINT ( 'NONE',  ( -1.715153634034234598, 134.3226862821014436, -9.534712964251941258 ) ) ;
#8544 = CARTESIAN_POINT ( 'NONE',  ( 13.56230152254410548, 5.196152422706630247, -8.962499998770995902 ) ) ;
#8545 = EDGE_LOOP ( 'NONE', ( #21634, #17320, #12168, #8842 ) ) ;
#8546 = CARTESIAN_POINT ( 'NONE',  ( 28.30384396178233075, -5.407089921784859143, 169.3017823552670507 ) ) ;
#8547 = CARTESIAN_POINT ( 'NONE',  ( 8.152565276336714462, 71.64768628210146062, -5.233372021372432847 ) ) ;
#8548 = CARTESIAN_POINT ( 'NONE',  ( 26.75643035624999655, -3.323476615752267715, -0.4031249993854607028 ) ) ;
#8549 = LINE ( 'NONE', #17274, #3522 ) ;
#8550 = CARTESIAN_POINT ( 'NONE',  ( 16.56230152254410726, 0.000000000000000000, 10.00000000000000000 ) ) ;
#8551 = CARTESIAN_POINT ( 'NONE',  ( -27.24356964374999635, 194.9468750006145399, 15.72908226750539384 ) ) ;
#8552 = CARTESIAN_POINT ( 'NONE',  ( 2.999999999999997335, 244.5000000000000000, 0.000000000000000000 ) ) ;
#8553 = CARTESIAN_POINT ( 'NONE',  ( 13.56230152254411436, -5.196152422706632912, -5.662499998771053811 ) ) ;
#8554 = CARTESIAN_POINT ( 'NONE',  ( 8.843639120294245259, 30.06481371789855572, 3.474262827703527901 ) ) ;
#8555 = CARTESIAN_POINT ( 'NONE',  ( 22.56230152254410370, 7.347880794884117764E-16, -1.912499998771022280 ) ) ;
#8556 = ORIENTED_EDGE ( 'NONE', *, *, #29518, .T. ) ;
#8557 = EDGE_LOOP ( 'NONE', ( #35033, #7027, #19253, #14070 ) ) ;
#8558 =( BOUNDED_CURVE ( )  B_SPLINE_CURVE ( 2, ( #10125, #10491, #18677, #13530, #24900, #33248, #7288, #1209, #27561 ),
 .UNSPECIFIED., .F., .F. ) 
 B_SPLINE_CURVE_WITH_KNOTS ( ( 3, 2, 2, 2, 3 ),
 ( 0.3958333333333333703, 0.4027777777777777901, 0.4166666666666666852, 0.4305555555555555802, 0.4375000000000000000 ),
 .UNSPECIFIED. ) 
 CURVE ( )  GEOMETRIC_REPRESENTATION_ITEM ( )  RATIONAL_B_SPLINE_CURVE ( ( 0.9330127018922194093, 0.9330127018922196314, 1.000000000000000000, 0.8660254037844387076, 1.000000000000000000, 0.8660254037844387076, 1.000000000000000000, 0.9330127018922194093, 0.9330127018922194093 ) ) 
 REPRESENTATION_ITEM ( '' )  );
#8559 = CARTESIAN_POINT ( 'NONE',  ( 15.00000000000000178, 240.1937500012290627, 3.464101615137757051 ) ) ;
#8560 = CARTESIAN_POINT ( 'NONE',  ( 7.228626920338837358, 40.12731371789853796, 10.49813415416005036 ) ) ;
#8561 = CARTESIAN_POINT ( 'NONE',  ( 16.56230152254411436, 7.209453229046482114, -9.309374999385527261 ) ) ;
#8562 = CARTESIAN_POINT ( 'NONE',  ( 21.00000000000000000, -6.646953231504538984, -8.240624999385500971 ) ) ;
#8563 = CARTESIAN_POINT ( 'NONE',  ( 6.092822981423662299, 141.6148137178985849, 14.25334919248795096 ) ) ;
#8564 = ADVANCED_FACE ( 'NONE', ( #32125 ), #6162, .T. ) ;
#8565 = VERTEX_POINT ( 'NONE', #26434 ) ;
#8566 = CARTESIAN_POINT ( 'NONE',  ( 10.31873187879410736, 3.604726614523240613, -2.034374999385505145 ) ) ;
#8567 = CARTESIAN_POINT ( 'NONE',  ( -27.24356964375000345, 199.8031250006145285, 0.000000000000000000 ) ) ;
#8568 = CARTESIAN_POINT ( 'NONE',  ( 31.09835460584942624, -7.209453229046482114, 165.4247213166987081 ) ) ;
#8569 = CARTESIAN_POINT ( 'NONE',  ( -36.73586230271183695, 206.8500491399821328, 5.686928522499748340 ) ) ;
#8570 = FACE_OUTER_BOUND ( 'NONE', #34385, .T. ) ;
#8571 = CARTESIAN_POINT ( 'NONE',  ( -20.01834529145943620, 195.0000000000000000, 18.41905743281650132 ) ) ;
#8572 = CARTESIAN_POINT ( 'NONE',  ( -56.13169563604517265, 210.1155267958017703, 4.499999999999996447 ) ) ;
#8573 = CARTESIAN_POINT ( 'NONE',  ( -39.71205436395490551, 214.6737587650352168, 4.842901733360204908 ) ) ;
#8574 = CARTESIAN_POINT ( 'NONE',  ( 25.18413345258806046, 3.604726614523236616, 169.4617919265805881 ) ) ;
#8575 = ORIENTED_EDGE ( 'NONE', *, *, #34130, .T. ) ;
#8576 = CARTESIAN_POINT ( 'NONE',  ( -27.24356964375000345, 199.8312500006145171, 0.000000000000000000 ) ) ;
#8577 = CARTESIAN_POINT ( 'NONE',  ( 15.00000000000000000, 0.000000000000000000, -7.200000000000011724 ) ) ;
#8578 = CARTESIAN_POINT ( 'NONE',  ( 11.08355503943118769, 21.43981371789854506, 10.83675517735179028 ) ) ;
#8579 = CARTESIAN_POINT ( 'NONE',  ( -63.06622103062156270, 212.1620413398628671, 8.530955311639223382 ) ) ;
#8580 = CARTESIAN_POINT ( 'NONE',  ( 12.53471296425194836, 17.02268628210144996, -2.311890736173178418 ) ) ;
#8581 = CARTESIAN_POINT ( 'NONE',  ( -7.228626920339069173, 48.07268628210143646, 10.49813415415989581 ) ) ;
#8582 = CARTESIAN_POINT ( 'NONE',  ( 16.56230152254411436, 6.928203230275514990, -4.612500000000012257 ) ) ;
#8583 = ORIENTED_EDGE ( 'NONE', *, *, #8896, .F. ) ;
#8584 = VECTOR ( 'NONE', #11480, 1000.000000000000000 ) ;
#8585 = DIRECTION ( 'NONE',  ( -1.000000000000000000, -6.123233995736766036E-17, 0.000000000000000000 ) ) ;
#8586 = CARTESIAN_POINT ( 'NONE',  ( 27.24356964375000345, 196.9343750006145228, -3.336375036156643733E-15 ) ) ;
#8587 = CARTESIAN_POINT ( 'NONE',  ( 31.28219875076131018, -6.928203230275506996, 167.5260695085981411 ) ) ;
#8588 = CARTESIAN_POINT ( 'NONE',  ( 13.49999999999999645, 196.3625000012290513, -23.38268590217984766 ) ) ;
#8589 = CARTESIAN_POINT ( 'NONE',  ( -27.00000000000000355, 195.0500000000000114, 0.000000000000000000 ) ) ;
#8590 = CARTESIAN_POINT ( 'NONE',  ( 0.000000000000000000, 210.0000000000000284, 0.000000000000000000 ) ) ;
#8591 = CARTESIAN_POINT ( 'NONE',  ( 26.75643035624999655, 245.0968750006145456, 3.323476615752267715 ) ) ;
#8592 = CARTESIAN_POINT ( 'NONE',  ( 5.233372021372610483, 101.6523137178985792, -8.152565276336593669 ) ) ;
#8593 = CARTESIAN_POINT ( 'NONE',  ( 26.75643035624999655, 242.3968750006145285, 3.323476615752267271 ) ) ;
#8594 = VERTEX_POINT ( 'NONE', #468 ) ;
#8595 = CARTESIAN_POINT ( 'NONE',  ( -55.54538769728823411, 211.8571965466039444, -6.469044688360768625 ) ) ;
#8596 = CARTESIAN_POINT ( 'NONE',  ( 28.15961270201155742, 5.196152422706630247, 166.2558873885250250 ) ) ;
#8597 = CARTESIAN_POINT ( 'NONE',  ( 21.00000000000000000, 245.2187500012290400, 6.928203230275506996 ) ) ;
#8598 = VERTEX_POINT ( 'NONE', #30418 ) ;
#8599 = CARTESIAN_POINT ( 'NONE',  ( -8.715434833792127023, 106.5398137178985536, 8.962234695871568846 ) ) ;
#8600 = CARTESIAN_POINT ( 'NONE',  ( 13.44051670066911264, -5.407089921784865361, -1.921874999385508875 ) ) ;
#8601 = CARTESIAN_POINT ( 'NONE',  ( 24.60236886974748316, -3.604726614523240613, 162.8121923168181695 ) ) ;
#8602 =( BOUNDED_CURVE ( )  B_SPLINE_CURVE ( 2, ( #21794, #10220, #15729, #22352, #30316, #18956, #33901, #27658, #27279 ),
 .UNSPECIFIED., .F., .F. ) 
 B_SPLINE_CURVE_WITH_KNOTS ( ( 3, 2, 2, 2, 3 ),
 ( 0.3958333333333333703, 0.4027777777777777901, 0.4166666666666666852, 0.4305555555555555802, 0.4375000000000000000 ),
 .UNSPECIFIED. ) 
 CURVE ( )  GEOMETRIC_REPRESENTATION_ITEM ( )  RATIONAL_B_SPLINE_CURVE ( ( 0.9330127018922194093, 0.9330127018922196314, 1.000000000000000000, 0.8660254037844387076, 1.000000000000000000, 0.8660254037844387076, 1.000000000000000000, 0.9330127018922194093, 0.9330127018922194093 ) ) 
 REPRESENTATION_ITEM ( '' )  );
#8603 = CARTESIAN_POINT ( 'NONE',  ( 15.24356964374999990, 3.323476615752268604, -2.990624999385476102 ) ) ;
#8604 = CARTESIAN_POINT ( 'NONE',  ( 11.48171059495408208, 65.71481371789855075, -4.944772684328420986 ) ) ;
#8605 = CARTESIAN_POINT ( 'NONE',  ( 27.24356964375000700, 199.1468750006145285, 15.72908226750537075 ) ) ;
#8606 = ORIENTED_EDGE ( 'NONE', *, *, #35270, .T. ) ;
#8607 = VERTEX_POINT ( 'NONE', #4439 ) ;
#8608 = EDGE_LOOP ( 'NONE', ( #3986, #5370, #2864, #5429 ) ) ;
#8609 = CARTESIAN_POINT ( 'NONE',  ( 15.00000000000000000, 0.000000000000000000, -6.693749998770953447 ) ) ;
#8610 = CARTESIAN_POINT ( 'NONE',  ( 23.87821517812499650, 4.985214923628404904, -2.090624999385476634 ) ) ;
#8611 = LINE ( 'NONE', #34014, #2750 ) ;
#8612 = CARTESIAN_POINT ( 'NONE',  ( 15.24356964375000167, 247.0843750006145285, 3.323476615752272600 ) ) ;
#8613 = CARTESIAN_POINT ( 'NONE',  ( 11.61527771782819940, 62.73518628210145209, -4.622313124798573369 ) ) ;
#8614 = CARTESIAN_POINT ( 'NONE',  ( -50.39211230271182984, 203.5309553116391896, 1.857196546604092724 ) ) ;
#8615 = EDGE_CURVE ( 'NONE', #15843, #24049, #26284, .T. ) ;
#8616 = CARTESIAN_POINT ( 'NONE',  ( 8.945811011643066024, 214.5203208706302291, -3.964960503608339959 ) ) ;
#8617 = CARTESIAN_POINT ( 'NONE',  ( -40.69419563604516554, 205.4999999999999716, 0.1155267958017633378 ) ) ;
#8618 =( NAMED_UNIT ( * ) SI_UNIT ( $, .STERADIAN. ) SOLID_ANGLE_UNIT ( ) );
#8619 = CARTESIAN_POINT ( 'NONE',  ( 36.87697111800645899, 7.347880794884117764E-16, 162.6323308142347059 ) ) ;
#8620 = CARTESIAN_POINT ( 'NONE',  ( -0.1745138560722763466, 100.7898137178985536, -12.50000000000000355 ) ) ;
#8621 = CARTESIAN_POINT ( 'NONE',  ( -62.67038769728824121, 208.6787018382581778, 4.469044688360752637 ) ) ;
#8622 = CARTESIAN_POINT ( 'NONE',  ( -42.28497103062156270, 202.6965474657331185, -4.350049139982091084 ) ) ;
#8623 =( BOUNDED_CURVE ( )  B_SPLINE_CURVE ( 2, ( #3150, #31226, #11133, #16831, #17200, #28373, #22711 ),
 .UNSPECIFIED., .F., .F. ) 
 B_SPLINE_CURVE_WITH_KNOTS ( ( 3, 2, 2, 3 ),
 ( 0.7391304347826076482, 0.7463768115942017722, 0.7536231884057957853, 0.7608695652173899093 ),
 .UNSPECIFIED. ) 
 CURVE ( )  GEOMETRIC_REPRESENTATION_ITEM ( )  RATIONAL_B_SPLINE_CURVE ( ( 1.000000000000018430, 0.8660254037844202779, 1.000000000000000000, 0.8660254037844387076, 1.000000000000000000, 0.8660254037844653530, 0.9999999999999733546 ) ) 
 REPRESENTATION_ITEM ( '' )  );
#8624 = CARTESIAN_POINT ( 'NONE',  ( 18.12178482187500350, -4.985214923628407568, -5.128124999385475391 ) ) ;
#8625 = CARTESIAN_POINT ( 'NONE',  ( 20.99999999999998579, 247.6374999999999886, -5.999999999999997335 ) ) ;
#8626 = CARTESIAN_POINT ( 'NONE',  ( -6.092822981423666739, 81.81481371789855928, -14.25334919248795096 ) ) ;
#8627 = CARTESIAN_POINT ( 'NONE',  ( -30.99627896937850124, 203.4690446883607535, -1.626142955000504209 ) ) ;
#8628 = ORIENTED_EDGE ( 'NONE', *, *, #33294, .T. ) ;
#8629 = CARTESIAN_POINT ( 'NONE',  ( 22.60769515458672885, 249.0236538117967200, -5.999999999999997335 ) ) ;
#8630 = CARTESIAN_POINT ( 'NONE',  ( 6.932735513423970097, 101.5476862821014379, 10.69584247140445044 ) ) ;
#8631 = EDGE_CURVE ( 'NONE', #9681, #2980, #21968, .T. ) ;
#8632 = CARTESIAN_POINT ( 'NONE',  ( 13.23911966647218996, 44.04768628210143788, -8.632099005475504683 ) ) ;
#8633 = FACE_OUTER_BOUND ( 'NONE', #3706, .T. ) ;
#8634 = CARTESIAN_POINT ( 'NONE',  ( 37.05016167317072728, -3.604726614523238837, 161.8172596703688555 ) ) ;
#8635 = CARTESIAN_POINT ( 'NONE',  ( 2.908627838312118019, 74.52268628210144641, 15.53471296425195369 ) ) ;
#8636 = CARTESIAN_POINT ( 'NONE',  ( 10.31873187879410914, 0.000000000000000000, -9.590624999385537919 ) ) ;
#8637 = DIRECTION ( 'NONE',  ( 1.000000000000000000, 0.000000000000000000, 0.000000000000000000 ) ) ;
#8638 = CARTESIAN_POINT ( 'NONE',  ( -48.42038769728821990, 208.1428034533959703, 6.469044688360770401 ) ) ;
#8639 = CARTESIAN_POINT ( 'NONE',  ( 7.234628195640322446, 195.6325961894323484, 26.99999999999999645 ) ) ;
#8640 = CARTESIAN_POINT ( 'NONE',  ( -6.932735513423968321, 41.74768628210144783, -10.69584247140445221 ) ) ;
#8641 = CARTESIAN_POINT ( 'NONE',  ( -13.49999999999998401, 196.0250000000000057, 23.38268590217985476 ) ) ;
#8642 = FACE_OUTER_BOUND ( 'NONE', #20757, .T. ) ;
#8643 = CARTESIAN_POINT ( 'NONE',  ( -1.715153634034234598, 5.522686282101450850, -9.534712964251941258 ) ) ;
#8644 = CARTESIAN_POINT ( 'NONE',  ( 15.24356964374999990, 248.0218750006145285, -3.323476615752268604 ) ) ;
#8645 = ORIENTED_EDGE ( 'NONE', *, *, #20704, .T. ) ;
#8646 = CARTESIAN_POINT ( 'NONE',  ( 23.99999999999999645, 5.196152422706631135, -5.099999999999993427 ) ) ;
#8648 = DIRECTION ( 'NONE',  ( -0.000000000000000000, -0.000000000000000000, -1.000000000000000000 ) ) ;
#8647 = PRODUCT_DEFINITION_SHAPE ( 'NONE', 'NONE',  #37509 ) ;
#8649 = CARTESIAN_POINT ( 'NONE',  ( 36.93903810116746911, 3.604726614523243278, 160.5471114303018680 ) ) ;
#8650 = CARTESIAN_POINT ( 'NONE',  ( 16.56230152254411081, -7.209453229046475009, -3.628124999385552663 ) ) ;
#8651 = CARTESIAN_POINT ( 'NONE',  ( 25.19067013329413385, -3.604726614523240613, 169.5365065289374797 ) ) ;
#8652 = CARTESIAN_POINT ( 'NONE',  ( 15.00000000000000000, 242.3500000000000227, 0.000000000000000000 ) ) ;
#8653 = CYLINDRICAL_SURFACE ( 'NONE', #36033, 6.000000000000001776 ) ;
#8654 = CARTESIAN_POINT ( 'NONE',  ( 11.61527771782819940, 71.93518628210145494, -4.622313124798573369 ) ) ;
#8655 = ORIENTED_EDGE ( 'NONE', *, *, #31634, .F. ) ;
#8656 = ORIENTED_EDGE ( 'NONE', *, *, #11802, .T. ) ;
#8657 = CARTESIAN_POINT ( 'NONE',  ( 27.62360488411350801, -5.196152422706632912, 160.1292899952607627 ) ) ;
#8658 = CARTESIAN_POINT ( 'NONE',  ( 13.49999999999999645, 195.4625000012290172, -23.38268590217984766 ) ) ;
#8660 = CARTESIAN_POINT ( 'NONE',  ( 20.99999999999999645, 250.0000000000000000, -8.000000000000000000 ) ) ;
#8659 = AXIS2_PLACEMENT_3D ( 'NONE', #17413, #8870, #31989 ) ;
#8661 = CARTESIAN_POINT ( 'NONE',  ( 15.50000000000000533, 47.88981371789855501, -0.1745138560722452326 ) ) ;
#8662 = CARTESIAN_POINT ( 'NONE',  ( 14.99999999999952394, -3.464101615137481716, -5.306249998770948828 ) ) ;
#8663 = ADVANCED_FACE ( 'NONE', ( #33438 ), #35713, .F. ) ;
#8664 = CARTESIAN_POINT ( 'NONE',  ( 23.87821517812500005, 241.4593750006145285, 4.985214923628404016 ) ) ;
#8665 = CARTESIAN_POINT ( 'NONE',  ( -48.02455436395490551, 206.6211998817774997, 3.209657149897401585 ) ) ;
#8666 = CARTESIAN_POINT ( 'NONE',  ( 22.56230152254411792, 7.347880794884125653E-16, -7.425000000000042455 ) ) ;
#8667 = CARTESIAN_POINT ( 'NONE',  ( 28.36878648460592700, -5.196152422706632912, 168.6467546639452166 ) ) ;
#8668 = CARTESIAN_POINT ( 'NONE',  ( 7.954856959092311719, 19.42731371789854933, -5.529263428287300108 ) ) ;
#8669 = CARTESIAN_POINT ( 'NONE',  ( 10.31873187879411269, 3.604726614523236616, -9.178124999385522287 ) ) ;
#8670 = SHAPE_DEFINITION_REPRESENTATION ( #32253, #29986 ) ;
#8671 = CARTESIAN_POINT ( 'NONE',  ( 24.06985121900113000, 194.9999999999999432, -12.35451244266598181 ) ) ;
#8672 = CARTESIAN_POINT ( 'NONE',  ( 27.24356964375000700, 195.0968750006145456, 15.72908226750537075 ) ) ;
#8673 = CARTESIAN_POINT ( 'NONE',  ( 13.04141134922778988, 139.0273137178985507, -8.927990412390371944 ) ) ;
#8674 = VECTOR ( 'NONE', #12592, 1000.000000000000000 ) ;
#8675 = VERTEX_POINT ( 'NONE', #21888 ) ;
#8676 = CARTESIAN_POINT ( 'NONE',  ( -12.46528703574805697, 40.59768628210144215, -2.660918448318280838 ) ) ;
#8677 = DIRECTION ( 'NONE',  ( 0.8083506638593009885, 0.5887012860850800999, 0.000000000000000000 ) ) ;
#8678 = EDGE_CURVE ( 'NONE', #19208, #17150, #4625, .T. ) ;
#8679 = CARTESIAN_POINT ( 'NONE',  ( -77.00000000000002842, 214.0000000000000000, 2.500000000000000000 ) ) ;
#8680 = CARTESIAN_POINT ( 'NONE',  ( 25.17923094205850276, 3.604726614523240613, 169.4057559748129336 ) ) ;
#8681 = CARTESIAN_POINT ( 'NONE',  ( 26.99999999999999645, 3.464101615137755275, -2.831249998770950072 ) ) ;
#8682 = CARTESIAN_POINT ( 'NONE',  ( 19.68408634441911431, -5.407089921784861808, -9.946874999385540761 ) ) ;
#8683 = CARTESIAN_POINT ( 'NONE',  ( 9.534712964251941258, 72.22268628210143504, -1.715153634034235708 ) ) ;
#8684 = FACE_OUTER_BOUND ( 'NONE', #16949, .T. ) ;
#8685 = FACE_BOUND ( 'NONE', #9692, .T. ) ;
#8686 = CARTESIAN_POINT ( 'NONE',  ( 4.944772684328679446, 98.38518628210145778, -11.48171059495397373 ) ) ;
#8687 = CARTESIAN_POINT ( 'NONE',  ( 15.02283181144952628, 7.347880794884122694E-16, 50.52293445648592751 ) ) ;
#8688 = CARTESIAN_POINT ( 'NONE',  ( -7.234628195640263826, 195.0700961906613600, -27.00000000000003553 ) ) ;
#8689 = ORIENTED_EDGE ( 'NONE', *, *, #32176, .F. ) ;
#8690 = CARTESIAN_POINT ( 'NONE',  ( 37.10082094864278446, 3.604726614523238837, 162.3962978386346663 ) ) ;
#8691 = CARTESIAN_POINT ( 'NONE',  ( 21.00000000000000000, -6.646953231504538984, -7.678124999385482319 ) ) ;
#8692 = CARTESIAN_POINT ( 'NONE',  ( -27.24356964375000345, 195.7718750006145569, -15.72908226750537786 ) ) ;
#8693 = CARTESIAN_POINT ( 'NONE',  ( 25.10405911393864642, 0.000000000000000000, 168.5465380477087933 ) ) ;
#8694 = CARTESIAN_POINT ( 'NONE',  ( 31.23317364535864371, -6.928203230275514990, 166.9657099896971602 ) ) ;
#8695 = CARTESIAN_POINT ( 'NONE',  ( -7.234628195640302017, 198.2924038105676630, 27.00000000000000711 ) ) ;
#8696 = CARTESIAN_POINT ( 'NONE',  ( 18.00000000000000355, 247.3750000000000000, 5.196152422706632912 ) ) ;
#8697 = CARTESIAN_POINT ( 'NONE',  ( -27.24356964375000345, 199.7656250006145342, -15.72908226750537786 ) ) ;
#8698 = CARTESIAN_POINT ( 'NONE',  ( 7.228626920338837358, 122.9273137178985422, 10.49813415416005036 ) ) ;
#8699 = AXIS2_PLACEMENT_3D ( 'NONE', #25646, #11611, #23369 ) ;
#8700 = CARTESIAN_POINT ( 'NONE',  ( 0.1745138560725515708, 125.4101862821014635, -12.50000000000000355 ) ) ;
#8702 = ORIENTED_EDGE ( 'NONE', *, *, #23541, .F. ) ;
#8701 = ORIENTED_EDGE ( 'NONE', *, *, #35342, .T. ) ;
#8703 = CARTESIAN_POINT ( 'NONE',  ( -13.62178482187500528, 197.9281250006145569, -23.59362340125807123 ) ) ;
#8704 = CARTESIAN_POINT ( 'NONE',  ( 18.12178482187500350, 242.1718750006145058, 4.985214923628407568 ) ) ;
#8705 = EDGE_CURVE ( 'NONE', #37366, #17495, #9944, .T. ) ;
#8706 = CARTESIAN_POINT ( 'NONE',  ( 16.56230152254411436, -6.928203230275514990, -3.037500000000043165 ) ) ;
#8707 = CARTESIAN_POINT ( 'NONE',  ( 2.908627838312458636, 91.87731371789854506, -15.53471296425188442 ) ) ;
#8708 = CARTESIAN_POINT ( 'NONE',  ( 23.87821517812499650, 4.985214923628404904, -4.903124999385472194 ) ) ;
#8709 = VECTOR ( 'NONE', #16765, 1000.000000000000000 ) ;
#8710 = COLOUR_RGB ( '',0.8941176470588234615, 0.8941176470588234615, 0.8941176470588234615 ) ;
#8711 = CARTESIAN_POINT ( 'NONE',  ( -26.99999999999998934, 195.6500000012290457, 15.58845726811991561 ) ) ;
#8712 = CARTESIAN_POINT ( 'NONE',  ( -9.465287035748106703, 79.80231371789852801, 2.064181346179061460 ) ) ;
#8713 = CARTESIAN_POINT ( 'NONE',  ( 19.68408634441910365, 5.407089921784857367, -2.990624999385543603 ) ) ;
#8714 = AXIS2_PLACEMENT_3D ( 'NONE', #16259, #30660, #4865 ) ;
#8715 = CARTESIAN_POINT ( 'NONE',  ( 26.75643035624999655, 241.4593750006145001, -3.323476615752271268 ) ) ;
#8716 = CARTESIAN_POINT ( 'NONE',  ( 2.311890736173452865, 55.07731371789855501, -12.53471296425189152 ) ) ;
#8717 = CARTESIAN_POINT ( 'NONE',  ( 21.00000000000016342, 4.000000000000002665, 50.00000000000000000 ) ) ;
#8718 = CARTESIAN_POINT ( 'NONE',  ( -12.50000000000000355, 95.51018628210144357, -0.1745138560725492671 ) ) ;
#8719 = CARTESIAN_POINT ( 'NONE',  ( 16.56230152254410015, -6.928203230275506996, -3.374999998770986664 ) ) ;
#8720 = CARTESIAN_POINT ( 'NONE',  ( -65.04538769728823411, 211.3212981617418222, -4.469044688360751749 ) ) ;
#8721 = DIRECTION ( 'NONE',  ( 0.000000000000000000, 0.000000000000000000, 1.000000000000000000 ) ) ;
#8722 = CARTESIAN_POINT ( 'NONE',  ( 36.94887460566563675, 3.464101615138066137, 163.4541914389360784 ) ) ;
#8723 = CARTESIAN_POINT ( 'NONE',  ( 10.83675517735155225, 110.4601862821014606, 11.08355503943142573 ) ) ;
#8724 = CARTESIAN_POINT ( 'NONE',  ( 2.660918448318279950, 15.29768628210143078, -12.46528703574805874 ) ) ;
#8725 = CARTESIAN_POINT ( 'NONE',  ( 22.56230152254412147, 7.347880794884125653E-16, -8.325000000000027711 ) ) ;
#8726 = CARTESIAN_POINT ( 'NONE',  ( 15.00000000000000000, 241.5062500012290627, 0.000000000000000000 ) ) ;
#8727 = CARTESIAN_POINT ( 'NONE',  ( -8.843639120294326972, 131.7351862821014663, 3.474262827703335166 ) ) ;
#8728 = CARTESIAN_POINT ( 'NONE',  ( 10.56230152254410726, 0.000000000000000000, -5.400000000000043876 ) ) ;
#8729 = CARTESIAN_POINT ( 'NONE',  ( 18.12178482187499640, 242.9218750006145058, -4.985214923628404904 ) ) ;
#8730 = VERTEX_POINT ( 'NONE', #4253 ) ;
#8731 = CARTESIAN_POINT ( 'NONE',  ( 13.56230152254411614, -5.196152422706632912, -4.762499998771041021 ) ) ;
#8732 = VECTOR ( 'NONE', #31338, 1000.000000000000000 ) ;
#8733 = CARTESIAN_POINT ( 'NONE',  ( 8.152565276336714462, 62.44768628210144357, -5.233372021372432847 ) ) ;
#8734 = PRODUCT_DEFINITION_FORMATION_WITH_SPECIFIED_SOURCE ( 'ANY', '', #37371, .NOT_KNOWN. ) ;
#8735 = CARTESIAN_POINT ( 'NONE',  ( 15.24356964374999990, 3.323476615752268604, -0.6281249993854746139 ) ) ;
#8736 = CARTESIAN_POINT ( 'NONE',  ( 26.99999999999999645, 241.1875000000000000, 3.464101615137751278 ) ) ;
#8737 = AXIS2_PLACEMENT_3D ( 'NONE', #24286, #35831, #32616 ) ;
#8738 = CARTESIAN_POINT ( 'NONE',  ( 15.00000000000000178, 242.4437500012290343, 3.464101615137757051 ) ) ;
#8739 = CARTESIAN_POINT ( 'NONE',  ( -28.99999999999999645, 201.9999999999999716, -1.007612034238798379E-23 ) ) ;
#8740 = FACE_OUTER_BOUND ( 'NONE', #3742, .T. ) ;
#8741 = CARTESIAN_POINT ( 'NONE',  ( 22.56230152254410370, 7.347880794884117764E-16, -5.512499998771014376 ) ) ;
#8742 = CARTESIAN_POINT ( 'NONE',  ( -6.840914352311947333, 44.43981371789855928, -6.594114490232462877 ) ) ;
#8743 = DIRECTION ( 'NONE',  ( 1.659705900203722642E-32, -2.710505431213758127E-16, -1.000000000000000000 ) ) ;
#8744 = VERTEX_POINT ( 'NONE', #1032 ) ;
#8745 = ORIENTED_EDGE ( 'NONE', *, *, #33601, .T. ) ;
#8746 = CARTESIAN_POINT ( 'NONE',  ( 26.99999999999999645, 239.9312500012290457, -7.347880794884117764E-16 ) ) ;
#8747 = CARTESIAN_POINT ( 'NONE',  ( 4.622313124798831829, 36.96481371789854364, -11.61527771782809282 ) ) ;
#8748 = CARTESIAN_POINT ( 'NONE',  ( 22.80587116629412137, 7.646167579472024665E-16, -8.521874999385502747 ) ) ;
#8749 = CARTESIAN_POINT ( 'NONE',  ( 15.24356964374999990, 0.000000000000000000, -9.703124999385471128 ) ) ;
#8750 = CARTESIAN_POINT ( 'NONE',  ( 11.61527771782809637, 11.66481371789854293, 4.622313124798827388 ) ) ;
#8751 = ORIENTED_EDGE ( 'NONE', *, *, #26547, .T. ) ;
#8752 = CARTESIAN_POINT ( 'NONE',  ( 22.80587116629412492, -3.604726614523238837, -4.059374999385534366 ) ) ;
#8753 = CARTESIAN_POINT ( 'NONE',  ( 27.24356964375000700, 199.5406250006145683, 15.72908226750537075 ) ) ;
#8754 = CARTESIAN_POINT ( 'NONE',  ( 34.36840877128340566, -5.407089921784861808, 166.9831475995933943 ) ) ;
#8755 = CARTESIAN_POINT ( 'NONE',  ( -64.84002896937849414, 202.6965474657332038, 4.350049139982197666 ) ) ;
#8756 = CARTESIAN_POINT ( 'NONE',  ( 20.99999999999999645, 248.0593750006144944, 6.646953231504538984 ) ) ;
#8757 =( LENGTH_UNIT ( ) NAMED_UNIT ( * ) SI_UNIT ( .MILLI., .METRE. ) );
#8758 = CARTESIAN_POINT ( 'NONE',  ( -22.24010127653566471, 195.0000000000001421, -15.49061856779472279 ) ) ;
#8759 = CARTESIAN_POINT ( 'NONE',  ( -54.74627896937850835, 205.4690446883607535, -1.090244570138286351 ) ) ;
#8760 = CARTESIAN_POINT ( 'NONE',  ( -46.44122103062156270, 208.3738570449993404, -6.530955311639226935 ) ) ;
#8761 = CARTESIAN_POINT ( 'NONE',  ( 28.21233043189729273, 5.407089921784856479, 168.2557779222707097 ) ) ;
#8762 = ORIENTED_EDGE ( 'NONE', *, *, #10856, .F. ) ;
#8763 = DIRECTION ( 'NONE',  ( -1.000000000000000000, 0.000000000000000000, 0.000000000000000000 ) ) ;
#8764 = CARTESIAN_POINT ( 'NONE',  ( 10.56230152254366672, 3.464101615137503920, -1.387500000000010170 ) ) ;
#8765 = CARTESIAN_POINT ( 'NONE',  ( -15.46528703574811736, 24.60231371789854649, 3.257655550456946436 ) ) ;
#8766 = CARTESIAN_POINT ( 'NONE',  ( -63.85788769728821990, 218.4690446883607535, 2.393094931466250408 ) ) ;
#8767 = CARTESIAN_POINT ( 'NONE',  ( -8.843639120294326972, 140.9351862821014549, 3.474262827703335166 ) ) ;
#8768 = EDGE_CURVE ( 'NONE', #22812, #22517, #8128, .T. ) ;
#8769 = CARTESIAN_POINT ( 'NONE',  ( -6.932735513423968321, 50.94768628210144357, -10.69584247140445221 ) ) ;
#8770 = EDGE_CURVE ( 'NONE', #18510, #19175, #24829, .T. ) ;
#8771 = CARTESIAN_POINT ( 'NONE',  ( 19.56230152254411792, 5.196152422706637353, -4.200000000000036593 ) ) ;
#8772 = ORIENTED_EDGE ( 'NONE', *, *, #7462, .F. ) ;
#8773 = CARTESIAN_POINT ( 'NONE',  ( -46.63913769728824121, 206.8500491399821044, -5.686928522499717253 ) ) ;
#8774 = DIRECTION ( 'NONE',  ( -0.000000000000000000, -0.000000000000000000, -1.000000000000000000 ) ) ;
#8775 = CARTESIAN_POINT ( 'NONE',  ( 13.62178482187499640, 195.6593750006145456, -23.59362340125807123 ) ) ;
#8776 = CARTESIAN_POINT ( 'NONE',  ( -70.80918835584510873, 215.2843023367891249, 7.500000000000000000 ) ) ;
#8777 = LINE ( 'NONE', #15027, #1692 ) ;
#8778 = CARTESIAN_POINT ( 'NONE',  ( 2.999999999999997335, 244.5000000000000000, 5.000000000000000000 ) ) ;
#8779 = CARTESIAN_POINT ( 'NONE',  ( 24.00000000000000000, 246.1562500012290400, 5.196152422706629359 ) ) ;
#8780 = EDGE_CURVE ( 'NONE', #21530, #21538, #11677, .T. ) ;
#8781 = CARTESIAN_POINT ( 'NONE',  ( 26.75643035624999655, 246.5218750006145285, -3.323476615752271712 ) ) ;
#8782 = CARTESIAN_POINT ( 'NONE',  ( -9.534712964251895073, 98.77731371789855075, -1.715153634034446428 ) ) ;
#8783 = CARTESIAN_POINT ( 'NONE',  ( 15.24356964374999990, 240.3718750006145228, -3.323476615752268604 ) ) ;
#8784 = ORIENTED_EDGE ( 'NONE', *, *, #5504, .T. ) ;
#8785 = CARTESIAN_POINT ( 'NONE',  ( -54.95163769728823411, 215.6869285224996986, -3.149950860017881382 ) ) ;
#8786 = CARTESIAN_POINT ( 'NONE',  ( 2.999999999999997335, 244.5000000000000000, 5.000000000000000000 ) ) ;
#8787 = CARTESIAN_POINT ( 'NONE',  ( 18.00000000000000000, 245.9312500012290457, -5.196152422706630247 ) ) ;
#8788 = ORIENTED_EDGE ( 'NONE', *, *, #11802, .F. ) ;
#8789 = CARTESIAN_POINT ( 'NONE',  ( -12.53471296425189152, 98.77731371789855075, -2.311890736173453309 ) ) ;
#8790 = CARTESIAN_POINT ( 'NONE',  ( 10.31873187879410736, 3.604726614523240613, -2.034374999385505145 ) ) ;
#8791 = CARTESIAN_POINT ( 'NONE',  ( 36.82301201863464968, 7.646167579472015790E-16, 159.2209272384671976 ) ) ;
#8792 = CARTESIAN_POINT ( 'NONE',  ( 18.12178482187500350, -4.985214923628407568, -3.328124999385479121 ) ) ;
#8793 = CARTESIAN_POINT ( 'NONE',  ( 2.660918448318002838, 68.30231371789854222, 12.46528703574811558 ) ) ;
#8794 = CARTESIAN_POINT ( 'NONE',  ( 13.62178482187499640, 199.7093750006145285, -23.59362340125807123 ) ) ;
#8795 = ORIENTED_EDGE ( 'NONE', *, *, #32424, .F. ) ;
#8796 = VECTOR ( 'NONE', #7210, 1000.000000000000000 ) ;
#8797 = ORIENTED_EDGE ( 'NONE', *, *, #9372, .F. ) ;
#8798 = ORIENTED_EDGE ( 'NONE', *, *, #17995, .F. ) ;
#8799 = CARTESIAN_POINT ( 'NONE',  ( 26.75643035624999655, 7.049594010296217766E-16, -4.865624999385476102 ) ) ;
#8800 = FACE_OUTER_BOUND ( 'NONE', #5199, .T. ) ;
#8801 = CARTESIAN_POINT ( 'NONE',  ( 21.00000000000000000, 246.0343750006144887, -6.646953231504538984 ) ) ;
#8802 = CARTESIAN_POINT ( 'NONE',  ( 12.46528703574805874, 45.19768628210143646, 2.660918448318279950 ) ) ;
#8803 = CARTESIAN_POINT ( 'NONE',  ( -53.95461230271182984, 208.1428034533958851, -6.469044688360754414 ) ) ;
#8804 = CARTESIAN_POINT ( 'NONE',  ( 11.24016333012526836, 213.6599387512111434, -4.770645753568232728 ) ) ;
#8805 = CARTESIAN_POINT ( 'NONE',  ( -44.85044563604516554, 206.6211998817775566, -3.209657149897419348 ) ) ;
#8806 =( LENGTH_UNIT ( ) NAMED_UNIT ( * ) SI_UNIT ( .MILLI., .METRE. ) );
#8807 = CARTESIAN_POINT ( 'NONE',  ( 33.72497000607938844, -5.196152422706629359, 161.0259329835556059 ) ) ;
#8808 = CARTESIAN_POINT ( 'NONE',  ( 2.660918448318002838, 95.90231371789856496, 12.46528703574811558 ) ) ;
#8809 = CARTESIAN_POINT ( 'NONE',  ( -60.88913769728824121, 207.8500491399821613, -3.954877714930864485 ) ) ;
#8810 = CARTESIAN_POINT ( 'NONE',  ( -50.99330436395489841, 210.1155267958016850, -8.500000000000003553 ) ) ;
#8811 = CARTESIAN_POINT ( 'NONE',  ( 18.12178482187500350, -4.985214923628407568, -3.778124999385484628 ) ) ;
#8812 = CARTESIAN_POINT ( 'NONE',  ( 15.50000000000000533, 84.68981371789855928, -0.1745138560722452326 ) ) ;
#8813 = CARTESIAN_POINT ( 'NONE',  ( -53.95461230271185116, 207.6069050685336492, -8.469044688360751749 ) ) ;
#8814 = VECTOR ( 'NONE', #19858, 1000.000000000000000 ) ;
#8815 = ORIENTED_EDGE ( 'NONE', *, *, #32108, .T. ) ;
#8816 = CARTESIAN_POINT ( 'NONE',  ( -10.69584247140444866, 113.0476862821014663, 6.932735513423972762 ) ) ;
#8817 = CARTESIAN_POINT ( 'NONE',  ( 2.908627838312118019, 37.72268628210143504, 15.53471296425195369 ) ) ;
#8818 = CIRCLE ( 'NONE', #26365, 2.499999999999996891 ) ;
#8819 = CYLINDRICAL_SURFACE ( 'NONE', #21099, 5.999999999999994671 ) ;
#8820 = CARTESIAN_POINT ( 'NONE',  ( 33.89776776044609363, -5.407089921784861808, 161.6036962298979915 ) ) ;
#8821 = CARTESIAN_POINT ( 'NONE',  ( -15.46528703574804986, 68.19768628210142936, -3.257655550457287497 ) ) ;
#8822 = CARTESIAN_POINT ( 'NONE',  ( -27.00000000000000355, 194.6888594429640875, -9.827195528215911580 ) ) ;
#8823 = CARTESIAN_POINT ( 'NONE',  ( 13.44051670066910908, 5.407089921784856479, -10.11562499938553650 ) ) ;
#8824 =( BOUNDED_CURVE ( )  B_SPLINE_CURVE ( 2, ( #1871, #33715, #25186, #36739, #10778, #2801, #5831 ),
 .UNSPECIFIED., .F., .F. ) 
 B_SPLINE_CURVE_WITH_KNOTS ( ( 3, 2, 2, 3 ),
 ( 0.9347826086956505520, 0.9420289855072447871, 0.9492753623188391332, 0.9565217391304334793 ),
 .UNSPECIFIED. ) 
 CURVE ( )  GEOMETRIC_REPRESENTATION_ITEM ( )  RATIONAL_B_SPLINE_CURVE ( ( 1.000000000000030864, 0.8660254037844079544, 1.000000000000000000, 0.8660254037844387076, 1.000000000000000000, 0.8660254037844633546, 0.9999999999999753530 ) ) 
 REPRESENTATION_ITEM ( '' )  );
#8825 = CARTESIAN_POINT ( 'NONE',  ( 10.56230152254410726, 0.000000000000000000, -8.550000000000029132 ) ) ;
#8826 = CARTESIAN_POINT ( 'NONE',  ( -45.84747103062156981, 213.3500491399821328, -5.571401726697985168 ) ) ;
#8827 = CARTESIAN_POINT ( 'NONE',  ( 10.82125134821038337, -2.451055655723595184, -9.999999999999994671 ) ) ;
#8828 = CARTESIAN_POINT ( 'NONE',  ( -2.660918448318275509, 38.29768628210145920, 12.46528703574805874 ) ) ;
#8829 = CARTESIAN_POINT ( 'NONE',  ( -27.24356964374999635, 199.4468750006145399, 15.72908226750539384 ) ) ;
#8830 = CARTESIAN_POINT ( 'NONE',  ( -7.234628195640302017, 197.9549038117966973, 27.00000000000000711 ) ) ;
#8831 = CARTESIAN_POINT ( 'NONE',  ( -6.594114490232312775, 13.86018628210145032, -6.840914352312096547 ) ) ;
#8832 = CARTESIAN_POINT ( 'NONE',  ( 26.75643035624999655, 247.7968750006145342, 3.323476615752267271 ) ) ;
#8833 = ORIENTED_EDGE ( 'NONE', *, *, #36051, .T. ) ;
#8834 = CARTESIAN_POINT ( 'NONE',  ( 26.99999999999999645, 3.464101615137755275, -5.587499999999997691 ) ) ;
#8835 = CARTESIAN_POINT ( 'NONE',  ( 25.20698035151260896, 0.000000000000000000, 166.9282849285064856 ) ) ;
#8836 = CARTESIAN_POINT ( 'NONE',  ( 22.56230152254410726, 7.347880794884117764E-16, -3.262499998771012599 ) ) ;
#8837 = CARTESIAN_POINT ( 'NONE',  ( 13.44051670066911264, 5.407089921784856479, -5.615624999385532057 ) ) ;
#8838 = CARTESIAN_POINT ( 'NONE',  ( 31.29935753756119965, -7.209453229046475009, 167.7221953391727709 ) ) ;
#8839 = CARTESIAN_POINT ( 'NONE',  ( 26.99999999999999645, 240.8125000000000000, -3.464101615137755275 ) ) ;
#8840 = CARTESIAN_POINT ( 'NONE',  ( 20.99999999999999645, 6.928203230275506996, -0.9562499987709413007 ) ) ;
#8841 = CARTESIAN_POINT ( 'NONE',  ( -4.944772684328673229, 66.18518628210144072, 11.48171059495397728 ) ) ;
#8842 = ORIENTED_EDGE ( 'NONE', *, *, #25857, .F. ) ;
#8843 = ORIENTED_EDGE ( 'NONE', *, *, #32287, .F. ) ;
#8844 = CYLINDRICAL_SURFACE ( 'NONE', #6085, 5.999999999999994671 ) ;
#8845 = CARTESIAN_POINT ( 'NONE',  ( -26.99999999999998934, 196.1000000012290627, 15.58845726811991561 ) ) ;
#8846 = CARTESIAN_POINT ( 'NONE',  ( -27.00000000000000355, 196.4750000012289775, -15.58845726811989429 ) ) ;
#8847 = CARTESIAN_POINT ( 'NONE',  ( 15.24356964374999990, 3.323476615752268604, -7.378124999385474503 ) ) ;
#8848 = CARTESIAN_POINT ( 'NONE',  ( -6.092822981423666739, 45.01481371789854791, -14.25334919248795096 ) ) ;
#8849 = CARTESIAN_POINT ( 'NONE',  ( 18.12178482187499640, 240.3343750006145285, -4.985214923628404904 ) ) ;
#8850 =( BOUNDED_CURVE ( )  B_SPLINE_CURVE ( 3, ( #8038, #19426, #16204, #10685 ),
 .UNSPECIFIED., .F., .F. ) 
 B_SPLINE_CURVE_WITH_KNOTS ( ( 4, 4 ),
 ( 1.570796326794900555, 4.712388980384686121 ),
 .UNSPECIFIED. ) 
 CURVE ( )  GEOMETRIC_REPRESENTATION_ITEM ( )  RATIONAL_B_SPLINE_CURVE ( ( 1.000000000000000000, 0.3333333333333359239, 0.3333333333333359239, 1.000000000000000000 ) ) 
 REPRESENTATION_ITEM ( '' )  );
#8851 = CARTESIAN_POINT ( 'NONE',  ( -39.51413769728823411, 212.1499508600178387, 3.954877714930865817 ) ) ;
#8852 = CARTESIAN_POINT ( 'NONE',  ( 16.56230152254410726, 0.000000000000000000, -10.00000000000000000 ) ) ;
#8853 = CARTESIAN_POINT ( 'NONE',  ( 34.32634463103817524, 5.196152422706631135, 167.8996764003886994 ) ) ;
#8854 = CARTESIAN_POINT ( 'NONE',  ( 2.064181346179061460, 22.30231371789854933, 9.465287035748106703 ) ) ;
#8855 = CARTESIAN_POINT ( 'NONE',  ( -54.35788769728821279, 216.4690446883607535, 1.857196546604031662 ) ) ;
#8856 = CARTESIAN_POINT ( 'NONE',  ( -41.28794563604517265, 203.8621396198271043, 6.307003348498029460 ) ) ;
#8857 = DIRECTION ( 'NONE',  ( 0.08715574274765150453, 0.000000000000000000, 0.9961946980917461003 ) ) ;
#8858 = CARTESIAN_POINT ( 'NONE',  ( 13.62178482187499640, 195.2093750006145569, -23.59362340125807123 ) ) ;
#8859 = CARTESIAN_POINT ( 'NONE',  ( 5.770363421894130873, 138.1648137178985678, -14.38691631536193860 ) ) ;
#8860 = ORIENTED_EDGE ( 'NONE', *, *, #7007, .T. ) ;
#8861 = CARTESIAN_POINT ( 'NONE',  ( -12.50000000000000355, 40.31018628210144783, -0.1745138560725492671 ) ) ;
#8862 = CARTESIAN_POINT ( 'NONE',  ( 19.56230152254411436, -5.196152422706629359, -8.287499998771014731 ) ) ;
#8863 = CARTESIAN_POINT ( 'NONE',  ( 13.49999999999999645, 198.9500000000000171, -23.38268590217984766 ) ) ;
#8864 = CARTESIAN_POINT ( 'NONE',  ( 24.40626844856526745, -3.604726614523240613, 160.5707542461117612 ) ) ;
#8865 = CARTESIAN_POINT ( 'NONE',  ( 15.00000000000000000, 0.000000000000000000, -1.293749998770965526 ) ) ;
#8866 = CARTESIAN_POINT ( 'NONE',  ( 16.56230152254411436, 7.209453229046482114, -9.309374999385527261 ) ) ;
#8867 = CARTESIAN_POINT ( 'NONE',  ( -68.40997103062156270, 215.5714017266979852, 3.350049139982118618 ) ) ;
#8868 = CARTESIAN_POINT ( 'NONE',  ( -9.500000000000005329, 58.71018628210145351, -0.1745138560725176813 ) ) ;
#8869 = CARTESIAN_POINT ( 'NONE',  ( 19.39230484541326760, 249.6424038105677141, 5.999999999999999112 ) ) ;
#8870 = DIRECTION ( 'NONE',  ( -0.000000000000000000, -1.000000000000000000, -0.000000000000000000 ) ) ;
#8871 = CARTESIAN_POINT ( 'NONE',  ( 2.311890736173175753, 102.1226862821014691, 12.53471296425194836 ) ) ;
#8872 = CARTESIAN_POINT ( 'NONE',  ( 33.64979817785242489, 5.196152422706637353, 160.1667150552271437 ) ) ;
#8873 = EDGE_LOOP ( 'NONE', ( #10245, #20263 ) ) ;
#8874 = CARTESIAN_POINT ( 'NONE',  ( 37.09428426793671463, -3.604726614523235284, 162.3215832362777746 ) ) ;
#8875 = CARTESIAN_POINT ( 'NONE',  ( 18.12178482187499640, 4.985214923628404904, -8.315624999385457627 ) ) ;
#8876 = FACE_OUTER_BOUND ( 'NONE', #35769, .T. ) ;
#8877 = CARTESIAN_POINT ( 'NONE',  ( 24.78703009969406779, 3.604726614523240613, 164.9228798334000601 ) ) ;
#8878 = CARTESIAN_POINT ( 'NONE',  ( 31.07629330841286830, -6.928203230275514990, 165.1725595331320449 ) ) ;
#8879 = CARTESIAN_POINT ( 'NONE',  ( 16.56230152254411436, 6.928203230275514990, -4.162500000000016520 ) ) ;
#8880 = CARTESIAN_POINT ( 'NONE',  ( 26.99999999999999645, 247.5250000000000057, -7.347880794884117764E-16 ) ) ;
#8881 = CARTESIAN_POINT ( 'NONE',  ( 5.778771075727756162E-15, 197.6656250006145399, 31.45816453501076637 ) ) ;
#8882 = CARTESIAN_POINT ( 'NONE',  ( -6.932735513424201912, 115.4523137178985621, 10.69584247140429412 ) ) ;
#8883 = CARTESIAN_POINT ( 'NONE',  ( 12.50000000000000355, 118.5101862821014578, 0.1745138560725507937 ) ) ;
#8885 = EDGE_LOOP ( 'NONE', ( #27251, #28943 ) ) ;
#8884 = ORIENTED_EDGE ( 'NONE', *, *, #36115, .T. ) ;
#8886 = CARTESIAN_POINT ( 'NONE',  ( 27.24356964375000700, 197.7406250006145285, 15.72908226750537075 ) ) ;
#8887 = CARTESIAN_POINT ( 'NONE',  ( 23.87821517812499650, 242.8468750006145171, -4.985214923628404904 ) ) ;
#8888 = AXIS2_PLACEMENT_3D ( 'NONE', #37356, #25258, #7644 ) ;
#8889 = CARTESIAN_POINT ( 'NONE',  ( -14.38691631536193860, 99.06481371789857349, -5.770363421894132649 ) ) ;
#8890 = ADVANCED_FACE ( 'NONE', ( #33071 ), #24169, .T. ) ;
#8891 = CARTESIAN_POINT ( 'NONE',  ( 26.75643035624999655, 3.323476615752271712, -4.940624999385510918 ) ) ;
#8892 = CARTESIAN_POINT ( 'NONE',  ( 26.75643035624999655, 247.7968750006145342, 3.323476615752267715 ) ) ;
#8893 = CARTESIAN_POINT ( 'NONE',  ( -13.49999999999998401, 197.4875000012290229, 23.38268590217985476 ) ) ;
#8894 = CARTESIAN_POINT ( 'NONE',  ( -3.474262827703527901, 69.16481371789853938, 8.843639120294245259 ) ) ;
#8895 = CARTESIAN_POINT ( 'NONE',  ( 10.31873187879410736, -3.604726614523240613, -5.953124999385525307 ) ) ;
#8896 = EDGE_CURVE ( 'NONE', #16958, #3817, #32572, .T. ) ;
#8897 = CARTESIAN_POINT ( 'NONE',  ( 15.24356964374999990, 241.1593750006145171, -3.323476615752268604 ) ) ;
#8898 = CARTESIAN_POINT ( 'NONE',  ( -2.311890736173448424, 41.27731371789855075, 12.53471296425189330 ) ) ;
#8899 = CARTESIAN_POINT ( 'NONE',  ( 27.89814547376861142, -5.196152422706632912, 163.2673032942497571 ) ) ;
#8900 = CARTESIAN_POINT ( 'NONE',  ( 10.69584247140445221, 108.4476862821014578, -6.932735513423970097 ) ) ;
#8901 = CARTESIAN_POINT ( 'NONE',  ( 16.56230152254410726, -6.928203230275506996, -4.274999998770977250 ) ) ;
#8902 = ADVANCED_FACE ( 'NONE', ( #1216 ), #12983, .T. ) ;
#8903 = CARTESIAN_POINT ( 'NONE',  ( -65.44122103062156270, 208.9097554298617752, -4.530955311639240257 ) ) ;
#8904 = CARTESIAN_POINT ( 'NONE',  ( 11.61527771782819940, 136.3351862821014606, -4.622313124798573369 ) ) ;
#8905 = CARTESIAN_POINT ( 'NONE',  ( 36.94560626531313829, 7.347880794884125653E-16, 163.4168341377576041 ) ) ;
#8906 = CARTESIAN_POINT ( 'NONE',  ( -14.25334919248782306, 96.08518628210146062, -6.092822981423979378 ) ) ;
#8907 = AXIS2_PLACEMENT_3D ( 'NONE', #21819, #22562, #28052 ) ;
#8908 = EDGE_CURVE ( 'NONE', #13274, #7860, #18310, .T. ) ;
#8909 = CARTESIAN_POINT ( 'NONE',  ( -12.53471296425194659, 12.42268628210144144, 2.311890736173176641 ) ) ;
#8910 = CARTESIAN_POINT ( 'NONE',  ( -20.76482629054277496, 195.0000000000000000, -17.25728419020853366 ) ) ;
#8911 = CARTESIAN_POINT ( 'NONE',  ( 1.069080835302379631E-14, 196.6250000012290400, 27.00000000000000000 ) ) ;
#8912 = CARTESIAN_POINT ( 'NONE',  ( 2.064181346179272847, 125.6976862821014578, -9.465287035748065847 ) ) ;
#8913 = CARTESIAN_POINT ( 'NONE',  ( 15.00000000000000178, 247.8437500012290400, 3.464101615137757051 ) ) ;
#8914 = CARTESIAN_POINT ( 'NONE',  ( -13.62178482187498396, 194.9843750006145626, 23.59362340125808188 ) ) ;
#8915 = CARTESIAN_POINT ( 'NONE',  ( 15.24356964374999990, 241.6468750006145285, 0.000000000000000000 ) ) ;
#8916 = VERTEX_POINT ( 'NONE', #19427 ) ;
#8917 = CARTESIAN_POINT ( 'NONE',  ( 18.06230152254410726, 1.836970198721029441E-16, 0.000000000000000000 ) ) ;
#8918 = CARTESIAN_POINT ( 'NONE',  ( 9.500000000000005329, 54.11018628210144499, 0.1745138560725188748 ) ) ;
#8919 = CARTESIAN_POINT ( 'NONE',  ( 24.00000000000000000, 243.9062500012290400, 5.196152422706629359 ) ) ;
#8920 = CYLINDRICAL_SURFACE ( 'NONE', #25333, 5.999999999999994671 ) ;
#8921 = CARTESIAN_POINT ( 'NONE',  ( 14.99999999999979039, -3.464101615137634038, -4.856249998770949539 ) ) ;
#8922 = CARTESIAN_POINT ( 'NONE',  ( -20.86978606573367045, 194.8588513912095550, -17.51182790300216752 ) ) ;
#8923 = PLANE ( 'NONE',  #22893 ) ;
#8924 = DIRECTION ( 'NONE',  ( 0.000000000000000000, 0.000000000000000000, 1.000000000000000000 ) ) ;
#8925 = CARTESIAN_POINT ( 'NONE',  ( 3.796722387233182339, 40.41481371789855359, 8.710071997420207879 ) ) ;
#8926 = CARTESIAN_POINT ( 'NONE',  ( 26.99999999999999645, 7.347880794884117764E-16, -5.118749998770960374 ) ) ;
#8927 = ORIENTED_EDGE ( 'NONE', *, *, #10754, .F. ) ;
#8928 = ORIENTED_EDGE ( 'NONE', *, *, #21219, .F. ) ;
#8929 = CARTESIAN_POINT ( 'NONE',  ( 18.12178482187499640, 249.6718750006145342, -4.985214923628404904 ) ) ;
#8930 = CARTESIAN_POINT ( 'NONE',  ( -8.715434833792127023, 42.13981371789854791, 8.962234695871568846 ) ) ;
#8931 = CARTESIAN_POINT ( 'NONE',  ( 13.44051670066911264, -5.407089921784865361, -8.671874999385515537 ) ) ;
#8932 = CARTESIAN_POINT ( 'NONE',  ( 23.87821517812500005, -4.985214923628404016, -9.103124999385482141 ) ) ;
#8933 = CARTESIAN_POINT ( 'NONE',  ( -11.61527771782809282, 16.26481371789853370, -4.622313124798832717 ) ) ;
#8934 = CARTESIAN_POINT ( 'NONE',  ( 22.56230152254473253, -3.464101615137399115, -1.162500000000026512 ) ) ;
#8935 = ORIENTED_EDGE ( 'NONE', *, *, #8505, .T. ) ;
#8936 = CARTESIAN_POINT ( 'NONE',  ( 22.80587116629412492, 3.604726614523243278, -4.884374999385530991 ) ) ;
#8937 = EDGE_LOOP ( 'NONE', ( #6883, #162, #19240, #14606 ) ) ;
#8938 = CARTESIAN_POINT ( 'NONE',  ( -27.24356964375000345, 199.3531250006145399, 0.000000000000000000 ) ) ;
#8939 = EDGE_CURVE ( 'NONE', #5013, #36517, #22190, .T. ) ;
#8940 = CARTESIAN_POINT ( 'NONE',  ( 37.48485094012463748, 7.646167579472024665E-16, 166.7857807271014394 ) ) ;
#8941 = ADVANCED_FACE ( 'NONE', ( #25281 ), #37201, .T. ) ;
#8942 = CARTESIAN_POINT ( 'NONE',  ( -30.79836230271183695, 204.3130714775002446, -3.149950860017828091 ) ) ;
#8943 = VECTOR ( 'NONE', #36979, 1000.000000000000000 ) ;
#8944 = CARTESIAN_POINT ( 'NONE',  ( 23.87821517812500005, 248.9968750006145228, 4.985214923628404016 ) ) ;
#8945 =( NAMED_UNIT ( * ) SI_UNIT ( $, .STERADIAN. ) SOLID_ANGLE_UNIT ( ) );
#8946 = CYLINDRICAL_SURFACE ( 'NONE', #26687, 6.000000000000001776 ) ;
#8947 = EDGE_CURVE ( 'NONE', #9483, #18816, #27936, .T. ) ;
#8948 = CARTESIAN_POINT ( 'NONE',  ( -55.34002896937850124, 206.1606490808709111, 2.350049139982143931 ) ) ;
#8949 = CARTESIAN_POINT ( 'NONE',  ( -32.58705436395489841, 205.3262412349647263, -4.842901733360204020 ) ) ;
#8950 = CARTESIAN_POINT ( 'NONE',  ( -20.80759054502876282, 194.9057263910046913, -17.45964060548497443 ) ) ;
#8951 = ORIENTED_EDGE ( 'NONE', *, *, #29804, .F. ) ;
#8952 = CARTESIAN_POINT ( 'NONE',  ( 10.56230152254410903, 0.000000000000000000, -7.987499998771019349 ) ) ;
#8953 = CARTESIAN_POINT ( 'NONE',  ( 8.927990412390371944, 21.72731371789853938, 13.04141134922778811 ) ) ;
#8954 = CARTESIAN_POINT ( 'NONE',  ( -57.32663769728824121, 202.5810206699313767, 4.149950860017909804 ) ) ;
#8955 = ADVANCED_FACE ( 'NONE', ( #22636, #7669 ), #5365, .F. ) ;
#8956 = CARTESIAN_POINT ( 'NONE',  ( 6.594114490232313663, 138.0601862821014549, 6.840914352312096547 ) ) ;
#8957 = CARTESIAN_POINT ( 'NONE',  ( 8.962234695871762469, 43.76018628210144357, -8.715434833791931624 ) ) ;
#8958 = CARTESIAN_POINT ( 'NONE',  ( 22.56230152254412147, 7.347880794884125653E-16, -3.825000000000050804 ) ) ;
#8959 = ORIENTED_EDGE ( 'NONE', *, *, #18561, .F. ) ;
#8960 = CARTESIAN_POINT ( 'NONE',  ( -36.94122103062156981, 208.3738570449994256, -6.530955311639227823 ) ) ;
#8961 = CARTESIAN_POINT ( 'NONE',  ( 5.233372021372432847, 27.94768628210144001, 8.152565276336710909 ) ) ;
#8962 = CARTESIAN_POINT ( 'NONE',  ( -1.926257025242585782E-15, 197.0468750006145626, -31.45816453501075927 ) ) ;
#8963 = CARTESIAN_POINT ( 'NONE',  ( 26.99999999999999645, 7.347880794884117764E-16, -1.574999999999993072 ) ) ;
#8964 = CARTESIAN_POINT ( 'NONE',  ( 1.069080835302379631E-14, 198.7624999999999886, 27.00000000000000000 ) ) ;
#8965 = CARTESIAN_POINT ( 'NONE',  ( 0.000000000000000000, 210.0000000000000284, -27.00000000000000000 ) ) ;
#8966 = CARTESIAN_POINT ( 'NONE',  ( 34.31327126962603558, -5.196152422706629359, 167.7502471956748877 ) ) ;
#8967 = CARTESIAN_POINT ( 'NONE',  ( 21.00000000000000000, 244.3468750006145171, -6.646953231504538984 ) ) ;
#8968 = CARTESIAN_POINT ( 'NONE',  ( -9.534712964251895073, 89.57731371789856212, -1.715153634034446428 ) ) ;
#8969 = CARTESIAN_POINT ( 'NONE',  ( 36.78872592836736288, 7.347880794884125653E-16, 161.6236836811924604 ) ) ;
#8970 = VECTOR ( 'NONE', #21963, 1000.000000000000000 ) ;
#8971 = VERTEX_POINT ( 'NONE', #36648 ) ;
#8972 = CARTESIAN_POINT ( 'NONE',  ( -56.73288769728823411, 203.5309553116391612, -1.857196546604028775 ) ) ;
#8973 = CARTESIAN_POINT ( 'NONE',  ( 21.00000000000000000, 245.8937500012290229, -6.928203230275506996 ) ) ;
#8974 = CARTESIAN_POINT ( 'NONE',  ( 0.1745138560722779009, 105.3898137178985621, 12.50000000000000355 ) ) ;
#8975 = CARTESIAN_POINT ( 'NONE',  ( 16.56230152254411436, 7.209453229046482114, -2.109374999385531080 ) ) ;
#8976 = CARTESIAN_POINT ( 'NONE',  ( 27.00000000000000355, 198.0875000012290457, -3.306546357697854128E-15 ) ) ;
#8977 = CARTESIAN_POINT ( 'NONE',  ( 15.24356964375000167, -3.323476615752272600, -2.465624999385486404 ) ) ;
#8978 = CARTESIAN_POINT ( 'NONE',  ( 6.932735513424201024, 74.05231371789855643, -10.69584247140429412 ) ) ;
#8979 = CARTESIAN_POINT ( 'NONE',  ( -27.24356964375000345, 197.1593750006145456, 0.000000000000000000 ) ) ;
#8980 = EDGE_LOOP ( 'NONE', ( #15418, #5660, #34133, #7428 ) ) ;
#8981 = ORIENTED_EDGE ( 'NONE', *, *, #2452, .T. ) ;
#8982 = CARTESIAN_POINT ( 'NONE',  ( 20.99999999999999645, -6.646953231504538984, -5.428124999385471661 ) ) ;
#8983 = CARTESIAN_POINT ( 'NONE',  ( 20.99999999999999645, 241.6187500012290457, 5.999999999999998224 ) ) ;
#8984 = CARTESIAN_POINT ( 'NONE',  ( 26.75643035624999655, 246.8593750006145342, -3.323476615752271712 ) ) ;
#8985 = CARTESIAN_POINT ( 'NONE',  ( -11.61527771782819940, 39.73518628210144499, 4.622313124798574258 ) ) ;
#8986 = ADVANCED_FACE ( 'NONE', ( #2344 ), #19979, .F. ) ;
#8987 = CARTESIAN_POINT ( 'NONE',  ( -47.81919563604517265, 216.5000000000000000, -0.1155267958017906493 ) ) ;
#8988 = DIRECTION ( 'NONE',  ( 0.08715574274765150453, 0.000000000000000000, 0.9961946980917461003 ) ) ;
#8989 = AXIS2_PLACEMENT_3D ( 'NONE', #29950, #18597, #33170 ) ;
#8990 = CARTESIAN_POINT ( 'NONE',  ( -66.02752896937849414, 213.3500491399821613, 5.571401726697954970 ) ) ;
#8991 =( NAMED_UNIT ( * ) PLANE_ANGLE_UNIT ( ) SI_UNIT ( $, .RADIAN. ) );
#8992 = CARTESIAN_POINT ( 'NONE',  ( 33.81648353596441581, 5.196152422706631135, 162.0719374165519469 ) ) ;
#8993 = CARTESIAN_POINT ( 'NONE',  ( 0.1745138560722779009, 105.3898137178985621, 12.50000000000000355 ) ) ;
#8994 = CARTESIAN_POINT ( 'NONE',  ( -60.69122103062156981, 208.9097554298617752, -4.530955311639240257 ) ) ;
#8995 = CARTESIAN_POINT ( 'NONE',  ( -65.63913769728823411, 206.8500491399821044, -5.686928522499717253 ) ) ;
#8996 = CARTESIAN_POINT ( 'NONE',  ( 26.75643035624999655, 7.049594010296217766E-16, -5.428124999385497418 ) ) ;
#8997 = CARTESIAN_POINT ( 'NONE',  ( -27.24356964375000345, 194.8531250006145115, 0.000000000000000000 ) ) ;
#8998 = CARTESIAN_POINT ( 'NONE',  ( -15.53471296425188442, 80.37731371789853085, -2.908627838312459080 ) ) ;
#8999 = CARTESIAN_POINT ( 'NONE',  ( -54.94419563604517265, 201.5000000000000000, 0.1155267958018195706 ) ) ;
#9000 = ORIENTED_EDGE ( 'NONE', *, *, #32582, .F. ) ;
#9001 = DIRECTION ( 'NONE',  ( 1.000000000000000000, 0.000000000000000000, 0.000000000000000000 ) ) ;
#9002 = CARTESIAN_POINT ( 'NONE',  ( 4.622313124798573369, 101.8351862821014464, 11.61527771782819940 ) ) ;
#9003 = CARTESIAN_POINT ( 'NONE',  ( -15.46528703574804986, 49.79768628210144499, -3.257655550457287497 ) ) ;
#9004 = FACE_OUTER_BOUND ( 'NONE', #5323, .T. ) ;
#9005 = DIRECTION ( 'NONE',  ( 0.000000000000000000, 0.000000000000000000, 1.000000000000000000 ) ) ;
#9006 = CARTESIAN_POINT ( 'NONE',  ( 2.908627838312118019, 65.32268628210144357, 15.53471296425195369 ) ) ;
#9007 = CARTESIAN_POINT ( 'NONE',  ( -1.926257025242585782E-15, 199.6906250006145456, -31.45816453501076637 ) ) ;
#9008 = CARTESIAN_POINT ( 'NONE',  ( 13.44051670066911441, -5.407089921784859143, -8.615624999385563143 ) ) ;
#9009 = CARTESIAN_POINT ( 'NONE',  ( 0.000000000000000000, 210.0000000000000284, -27.00000000000000000 ) ) ;
#9010 = CARTESIAN_POINT ( 'NONE',  ( -44.85788769728821990, 216.4690446883607535, 1.857196546604031662 ) ) ;
#9011 = CARTESIAN_POINT ( 'NONE',  ( 10.44739295067906681, -1.007476398167555631, -10.00000000000000000 ) ) ;
#9012 = CARTESIAN_POINT ( 'NONE',  ( -10.69584247140444866, 39.44768628210145067, 6.932735513423972762 ) ) ;
#9013 = CARTESIAN_POINT ( 'NONE',  ( -26.99999999999998934, 195.0875000000000341, 15.58845726811991561 ) ) ;
#9014 = CARTESIAN_POINT ( 'NONE',  ( 26.99999999999946354, 3.464101615138061696, -7.781249998770928933 ) ) ;
#9015 = CARTESIAN_POINT ( 'NONE',  ( 6.840914352312096547, 6.960186282101432198, -6.594114490232313663 ) ) ;
#9016 = CARTESIAN_POINT ( 'NONE',  ( 26.75643035624999655, 246.4843750006145342, -7.049594010296217766E-16 ) ) ;
#9017 = ORIENTED_EDGE ( 'NONE', *, *, #6091, .T. ) ;
#9018 = CARTESIAN_POINT ( 'NONE',  ( 23.99999999999999645, 5.196152422706631135, -7.800000000000001599 ) ) ;
#9019 = CYLINDRICAL_SURFACE ( 'NONE', #33031, 6.000000000000001776 ) ;
#9020 = CARTESIAN_POINT ( 'NONE',  ( 18.00000000000000000, 5.196152422706630247, -6.768749998770945631 ) ) ;
#9021 = CARTESIAN_POINT ( 'NONE',  ( 10.31873187879411091, 3.604726614523236616, -5.128124999385527794 ) ) ;
#9022 = CARTESIAN_POINT ( 'NONE',  ( 37.40804494182826545, -3.604726614523235284, 165.9078841494080336 ) ) ;
#9023 = CARTESIAN_POINT ( 'NONE',  ( 15.00000000000000000, 240.0625000000000000, -3.464101615137752166 ) ) ;
#9024 = EDGE_CURVE ( 'NONE', #8744, #3817, #30977, .T. ) ;
#9025 = CARTESIAN_POINT ( 'NONE',  ( 13.49999999999999645, 198.9500000000000171, -23.38268590217984766 ) ) ;
#9026 = CARTESIAN_POINT ( 'NONE',  ( -7.228626920339070061, 66.47268628210144925, 10.49813415415989404 ) ) ;
#9027 = ORIENTED_EDGE ( 'NONE', *, *, #33003, .T. ) ;
#9028 = ORIENTED_EDGE ( 'NONE', *, *, #20849, .T. ) ;
#9029 = DIRECTION ( 'NONE',  ( -1.000000000000000000, -0.000000000000000000, -0.000000000000000000 ) ) ;
#9030 = EDGE_CURVE ( 'NONE', #16114, #29947, #29132, .T. ) ;
#9031 = CARTESIAN_POINT ( 'NONE',  ( 20.99999999999999645, 185.0294372515228645, 0.000000000000000000 ) ) ;
#9032 = CARTESIAN_POINT ( 'NONE',  ( 26.99999999999999645, 242.9874999999999829, 3.464101615137751278 ) ) ;
#9033 = CARTESIAN_POINT ( 'NONE',  ( 23.87821517812500005, -4.985214923628404016, -5.390624999385473792 ) ) ;
#9034 = CARTESIAN_POINT ( 'NONE',  ( -15.46528703574811736, 24.60231371789854649, 3.257655550456946436 ) ) ;
#9035 = ADVANCED_FACE ( 'NONE', ( #25647 ), #16944, .F. ) ;
#9036 = CARTESIAN_POINT ( 'NONE',  ( 26.99999999999999645, 249.3249999999999886, -7.347880794884117764E-16 ) ) ;
#9037 = CARTESIAN_POINT ( 'NONE',  ( 23.87821517812500005, 240.5593750006145228, 4.985214923628404016 ) ) ;
#9038 = CARTESIAN_POINT ( 'NONE',  ( -64.44419563604517975, 205.4999999999999716, 0.1155267958017633378 ) ) ;
#9039 = FACE_OUTER_BOUND ( 'NONE', #33452, .T. ) ;
#9040 = CARTESIAN_POINT ( 'NONE',  ( 30.60810355289388696, 7.209453229046482114, 159.8211261399325736 ) ) ;
#9041 = CARTESIAN_POINT ( 'NONE',  ( 3.474262827703532341, 27.76481371789854791, -8.843639120294245259 ) ) ;
#9042 = CARTESIAN_POINT ( 'NONE',  ( -60.49330436395489841, 210.1155267958017134, -6.500000000000000888 ) ) ;
#9043 = CARTESIAN_POINT ( 'NONE',  ( -43.86086230271183695, 214.1499508600178387, -7.418979330068641964 ) ) ;
#9044 = APPLICATION_PROTOCOL_DEFINITION ( 'draft international standard', 'automotive_design', 1998, #35935 ) ;
#9045 = CARTESIAN_POINT ( 'NONE',  ( 22.97035613655870989, 195.0000000000000568, 14.56992986484456587 ) ) ;
#9046 = CARTESIAN_POINT ( 'NONE',  ( 27.24356964374999635, 196.9718750006145456, -15.72908226750539029 ) ) ;
#9047 = CARTESIAN_POINT ( 'NONE',  ( 13.23911966647199812, 131.5523137178985564, 8.632099005475788900 ) ) ;
#9048 = CARTESIAN_POINT ( 'NONE',  ( -58.11086230271183695, 213.1499508600178387, -5.686928522499747451 ) ) ;
#9049 = VERTEX_POINT ( 'NONE', #1966 ) ;
#9050 =( BOUNDED_CURVE ( )  B_SPLINE_CURVE ( 2, ( #34992, #15097, #26091, #23072, #12058, #8662, #29109 ),
 .UNSPECIFIED., .F., .F. ) 
 B_SPLINE_CURVE_WITH_KNOTS ( ( 3, 2, 2, 3 ),
 ( 0.4565217391304355332, 0.4637681159420298238, 0.4710144927536241144, 0.4782608695652184050 ),
 .UNSPECIFIED. ) 
 CURVE ( )  GEOMETRIC_REPRESENTATION_ITEM ( )  RATIONAL_B_SPLINE_CURVE ( ( 0.9999999999999856781, 0.8660254037844530295, 1.000000000000000000, 0.8660254037844387076, 1.000000000000000000, 0.8660254037844202779, 1.000000000000018430 ) ) 
 REPRESENTATION_ITEM ( '' )  );
#9051 = CARTESIAN_POINT ( 'NONE',  ( -12.50000000000000355, 49.51018628210145067, -0.1745138560725492671 ) ) ;
#9052 = CARTESIAN_POINT ( 'NONE',  ( 15.00000000000000178, -3.464101615137757051, -6.262500000000007283 ) ) ;
#9053 = CARTESIAN_POINT ( 'NONE',  ( 27.00000000000001421, 198.8374999999999773, 15.58845726811988897 ) ) ;
#9054 = CARTESIAN_POINT ( 'NONE',  ( 34.52528910822917396, -5.407089921784861808, 168.7762980561585380 ) ) ;
#9055 = CARTESIAN_POINT ( 'NONE',  ( 18.00000000000000355, -5.196152422706632912, -3.018749998770942078 ) ) ;
#9056 = CARTESIAN_POINT ( 'NONE',  ( 13.44051670066910908, 5.407089921784862696, -9.271874999385531169 ) ) ;
#9057 = CARTESIAN_POINT ( 'NONE',  ( -65.44122103062156270, 208.3738570449994256, -6.530955311639227823 ) ) ;
#9058 = CARTESIAN_POINT ( 'NONE',  ( 22.80587116629411071, -3.604726614523235284, -2.653124999385503724 ) ) ;
#9059 = CARTESIAN_POINT ( 'NONE',  ( -0.1745138560725182642, 65.61018628210146630, 9.500000000000005329 ) ) ;
#9060 = CARTESIAN_POINT ( 'NONE',  ( 18.00000000000000355, 249.6250000000000000, 5.196152422706632912 ) ) ;
#9061 = CARTESIAN_POINT ( 'NONE',  ( 26.99999999999999645, 245.7624999999999886, -3.464101615137755275 ) ) ;
#9062 = CARTESIAN_POINT ( 'NONE',  ( 0.1745138560725515708, 88.61018628210146630, -12.50000000000000355 ) ) ;
#9063 = CARTESIAN_POINT ( 'NONE',  ( 28.00273236506578201, 5.196152422706630247, 164.4627369319599097 ) ) ;
#9064 = CARTESIAN_POINT ( 'NONE',  ( 27.00000000000000355, 198.5375000012290627, -3.306546357697854128E-15 ) ) ;
#9065 = VERTEX_POINT ( 'NONE', #16576 ) ;
#9066 = CARTESIAN_POINT ( 'NONE',  ( 33.78501001826630556, -5.407089921784855591, 160.3148693392417670 ) ) ;
#9067 = CARTESIAN_POINT ( 'NONE',  ( 18.12178482187500350, -4.985214923628407568, -8.615624999385479654 ) ) ;
#9068 = DIRECTION ( 'NONE',  ( -0.000000000000000000, 1.000000000000000000, -0.000000000000000000 ) ) ;
#9069 = CARTESIAN_POINT ( 'NONE',  ( 24.82625018393051164, 3.604726614523240613, 165.3711674475414100 ) ) ;
#9070 = CARTESIAN_POINT ( 'NONE',  ( 34.04199902021685631, 5.196152422706637353, 164.6495911966399888 ) ) ;
#9071 = CARTESIAN_POINT ( 'NONE',  ( 7.234628195640363302, 196.7174038105676459, -26.99999999999996803 ) ) ;
#9072 = CARTESIAN_POINT ( 'NONE',  ( 26.99999999999999645, 247.9749999999999943, -7.347880794884117764E-16 ) ) ;
#9073 = CARTESIAN_POINT ( 'NONE',  ( 13.62178482187499640, 199.6531250006145228, -23.59362340125807123 ) ) ;
#9074 =( BOUNDED_CURVE ( )  B_SPLINE_CURVE ( 2, ( #2694, #14270, #37002, #31692, #31880, #8213, #8398 ),
 .UNSPECIFIED., .F., .F. ) 
 B_SPLINE_CURVE_WITH_KNOTS ( ( 3, 2, 2, 3 ),
 ( 0.1739130434782606427, 0.1811594202898546835, 0.1884057971014487243, 0.1956521739130427651 ),
 .UNSPECIFIED. ) 
 CURVE ( )  GEOMETRIC_REPRESENTATION_ITEM ( )  RATIONAL_B_SPLINE_CURVE ( ( 1.000000000000003997, 0.8660254037844345998, 1.000000000000000000, 0.8660254037844387076, 1.000000000000000000, 0.8660254037844520303, 0.9999999999999866773 ) ) 
 REPRESENTATION_ITEM ( '' )  );
#9075 = CARTESIAN_POINT ( 'NONE',  ( -12.53471296425189152, 107.9773137178985536, -2.311890736173453753 ) ) ;
#9076 = CARTESIAN_POINT ( 'NONE',  ( 11.61527771782819940, 127.1351862821014578, -4.622313124798573369 ) ) ;
#9078 = EDGE_LOOP ( 'NONE', ( #29235, #5460, #30093, #8701 ) ) ;
#9077 = ORIENTED_EDGE ( 'NONE', *, *, #11409, .F. ) ;
#9079 = CARTESIAN_POINT ( 'NONE',  ( 13.62178482187499640, 196.5031250006145456, -23.59362340125807123 ) ) ;
#9080 = CARTESIAN_POINT ( 'NONE',  ( 23.87821517812500005, 241.7968750006145342, 4.985214923628404016 ) ) ;
#9081 = CARTESIAN_POINT ( 'NONE',  ( 13.23911966647199812, 85.55231371789855643, 8.632099005475788900 ) ) ;
#9082 = CARTESIAN_POINT ( 'NONE',  ( 23.87821517812500005, -4.985214923628404016, -4.153124999385471305 ) ) ;
#9083 = CARTESIAN_POINT ( 'NONE',  ( 26.75643035624999655, 248.6968750006145115, 3.323476615752267715 ) ) ;
#9084 = VECTOR ( 'NONE', #26243, 1000.000000000000000 ) ;
#9085 = CARTESIAN_POINT ( 'NONE',  ( 3.474262827703335166, 101.8351862821014606, 8.843639120294326972 ) ) ;
#9086 = CARTESIAN_POINT ( 'NONE',  ( 13.50000000000001421, 195.7625000012290570, 23.38268590217984055 ) ) ;
#9087 = CARTESIAN_POINT ( 'NONE',  ( -8.710071997420207879, 70.31481371789853085, 3.796722387233182339 ) ) ;
#9088 = CARTESIAN_POINT ( 'NONE',  ( 10.31873187879411269, -3.604726614523240613, -6.403124999385521043 ) ) ;
#9089 = CARTESIAN_POINT ( 'NONE',  ( 26.75643035624999655, 241.3843750006145115, 3.323476615752267271 ) ) ;
#9090 = CARTESIAN_POINT ( 'NONE',  ( 12.50000000000000355, 57.08981371789855075, -0.1745138560722771515 ) ) ;
#9091 = CARTESIAN_POINT ( 'NONE',  ( 26.99999999999999645, 246.6437500012290513, 3.464101615137751278 ) ) ;
#9092 = AXIS2_PLACEMENT_3D ( 'NONE', #23152, #37167, #8190 ) ;
#9093 = CARTESIAN_POINT ( 'NONE',  ( 4.622313124798573369, 101.8351862821014464, 11.61527771782819940 ) ) ;
#9094 = CARTESIAN_POINT ( 'NONE',  ( 19.56230152254411081, -5.196152422706629359, -5.137499998771027698 ) ) ;
#9095 = CARTESIAN_POINT ( 'NONE',  ( -35.55580436395490551, 216.5000000000000000, 0.1155267958017343610 ) ) ;
#9096 = CARTESIAN_POINT ( 'NONE',  ( -0.1745138560725500443, 139.2101862821014606, 12.50000000000000355 ) ) ;
#9097 = CARTESIAN_POINT ( 'NONE',  ( 33.68901826208886519, 5.196152422706637353, 160.6150026693684367 ) ) ;
#9098 = CARTESIAN_POINT ( 'NONE',  ( -14.25334919248782306, 86.88518628210145778, -6.092822981423979378 ) ) ;
#9099 = DIRECTION ( 'NONE',  ( -0.8660254037844613562, -0.4999999999999605871, 0.000000000000000000 ) ) ;
#9100 = CARTESIAN_POINT ( 'NONE',  ( 26.99999999999999645, 244.4687500012290684, -3.464101615137755275 ) ) ;
#9101 = CARTESIAN_POINT ( 'NONE',  ( -3.474262827703337830, 115.6351862821014436, -8.843639120294326972 ) ) ;
#9102 = CARTESIAN_POINT ( 'NONE',  ( 7.234628195640363302, 195.0299038117966575, -26.99999999999996803 ) ) ;
#9103 = EDGE_CURVE ( 'NONE', #36001, #33455, #8228, .T. ) ;
#9104 = CARTESIAN_POINT ( 'NONE',  ( -8.927990412390661490, 20.47268628210143859, 13.04141134922759804 ) ) ;
#9105 = CARTESIAN_POINT ( 'NONE',  ( 16.56230152254410726, 0.000000000000000000, -10.00000000000000000 ) ) ;
#9106 = CARTESIAN_POINT ( 'NONE',  ( 26.75643035624999655, 242.3593750006145342, -3.323476615752271712 ) ) ;
#9108 = ORIENTED_EDGE ( 'NONE', *, *, #19180, .T. ) ;
#9107 =( GEOMETRIC_REPRESENTATION_CONTEXT ( 3 ) GLOBAL_UNCERTAINTY_ASSIGNED_CONTEXT ( ( #30949 ) ) GLOBAL_UNIT_ASSIGNED_CONTEXT ( ( #7623, #16529, #1921 ) ) REPRESENTATION_CONTEXT ( 'NONE', 'WORKASPACE' ) );
#9109 = CARTESIAN_POINT ( 'NONE',  ( 25.02725311564228150, 3.604726614523236616, 167.6686414700154444 ) ) ;
#9110 = CARTESIAN_POINT ( 'NONE',  ( -6.840914352312096547, 48.36018628210145209, 6.594114490232313663 ) ) ;
#9111 =( BOUNDED_CURVE ( )  B_SPLINE_CURVE ( 2, ( #28484, #11430, #26198, #22816, #19977, #14279, #5544 ),
 .UNSPECIFIED., .F., .F. ) 
 B_SPLINE_CURVE_WITH_KNOTS ( ( 3, 2, 2, 3 ),
 ( 0.6086956521739131931, 0.6159420289855074282, 0.6231884057971016633, 0.6304347826086960094 ),
 .UNSPECIFIED. ) 
 CURVE ( )  GEOMETRIC_REPRESENTATION_ITEM ( )  RATIONAL_B_SPLINE_CURVE ( ( 0.9999999999999980016, 0.8660254037844407060, 1.000000000000000000, 0.8660254037844387076, 1.000000000000000000, 0.8660254037844326014, 1.000000000000006217 ) ) 
 REPRESENTATION_ITEM ( '' )  );
#9112 = CARTESIAN_POINT ( 'NONE',  ( 15.24356964374999990, 0.000000000000000000, -1.490624999385459226 ) ) ;
#9113 = CARTESIAN_POINT ( 'NONE',  ( 20.99999999999995381, 241.5625000000000000, 5.999999999999998224 ) ) ;
#9114 = DIRECTION ( 'NONE',  ( 1.047113545471812582E-14, 0.1163425707149433608, -0.9932091452657082487 ) ) ;
#9115 = DIRECTION ( 'NONE',  ( 0.000000000000000000, 0.000000000000000000, 1.000000000000000000 ) ) ;
#9116 = CARTESIAN_POINT ( 'NONE',  ( 20.99999999999997868, 246.0625000000000284, 5.999999999999999112 ) ) ;
#9117 = CARTESIAN_POINT ( 'NONE',  ( 10.31873187879411091, 3.604726614523236616, -0.6281249993855065883 ) ) ;
#9118 = CARTESIAN_POINT ( 'NONE',  ( 5.529263428287300108, 40.12731371789853796, 7.954856959092309943 ) ) ;
#9119 = DIRECTION ( 'NONE',  ( 0.000000000000000000, 0.000000000000000000, 1.000000000000000000 ) ) ;
#9120 = ORIENTED_EDGE ( 'NONE', *, *, #20907, .F. ) ;
#9121 = CARTESIAN_POINT ( 'NONE',  ( 21.00000000000000000, 240.2687500012290513, 6.928203230275506996 ) ) ;
#9122 = CARTESIAN_POINT ( 'NONE',  ( 11.61527771782809637, 48.46481371789855785, 4.622313124798827388 ) ) ;
#9123 = CARTESIAN_POINT ( 'NONE',  ( 26.75643035624999655, -3.323476615752267715, -9.065624999385498484 ) ) ;
#9124 = CARTESIAN_POINT ( 'NONE',  ( -4.622313124798826500, 13.96481371789853831, 11.61527771782809637 ) ) ;
#9125 = ADVANCED_FACE ( 'NONE', ( #22078 ), #8039, .T. ) ;
#9126 = CARTESIAN_POINT ( 'NONE',  ( 23.99999999999999645, 248.0499999999999829, -5.196152422706631135 ) ) ;
#9127 = ORIENTED_EDGE ( 'NONE', *, *, #34611, .T. ) ;
#9128 = CARTESIAN_POINT ( 'NONE',  ( 16.56230152254411436, 7.209453229046482114, -3.009374999385522553 ) ) ;
#9129 = ORIENTED_EDGE ( 'NONE', *, *, #1321, .F. ) ;
#9130 = CARTESIAN_POINT ( 'NONE',  ( 5.778771075727756162E-15, 198.1156250006145285, 31.45816453501075927 ) ) ;
#9131 = CARTESIAN_POINT ( 'NONE',  ( 37.36392234706227811, -3.604726614523238837, 165.4035605834991145 ) ) ;
#9132 = EDGE_CURVE ( 'NONE', #8730, #18034, #29922, .T. ) ;
#9133 = VECTOR ( 'NONE', #17110, 1000.000000000000000 ) ;
#9134 = CARTESIAN_POINT ( 'NONE',  ( -33.96502896937850124, 215.5714017266979567, -3.350049139982168800 ) ) ;
#9135 = CARTESIAN_POINT ( 'NONE',  ( 18.00000000000000000, 245.4812500012290570, -5.196152422706630247 ) ) ;
#9136 = CARTESIAN_POINT ( 'NONE',  ( -26.30981681325194899, 195.0000000000000853, -6.417592593584456218 ) ) ;
#9137 = CARTESIAN_POINT ( 'NONE',  ( -58.11086230271183695, 212.1499508600178387, -3.954877714930852495 ) ) ;
#9138 = CARTESIAN_POINT ( 'NONE',  ( -34.17038769728823411, 208.1428034533959703, 6.469044688360770401 ) ) ;
#9139 = CARTESIAN_POINT ( 'NONE',  ( 28.26462387754589045, -5.407089921784859143, 168.8534947411257576 ) ) ;
#9140 = EDGE_LOOP ( 'NONE', ( #29627, #25716, #26194, #20810 ) ) ;
#9141 = CARTESIAN_POINT ( 'NONE',  ( 26.99999999999999645, 241.6937500012290343, 3.464101615137751278 ) ) ;
#9142 = CARTESIAN_POINT ( 'NONE',  ( -2.908627838312453306, 22.87731371789854151, 15.53471296425188797 ) ) ;
#9143 = CARTESIAN_POINT ( 'NONE',  ( -54.55580436395489841, 218.5000000000000000, 0.1155267958017064944 ) ) ;
#9144 = CARTESIAN_POINT ( 'NONE',  ( -7.954856959092191815, 123.9726862821014493, -5.529263428287477744 ) ) ;
#9145 = CARTESIAN_POINT ( 'NONE',  ( 2.311890736173175753, 37.72268628210144215, 12.53471296425194836 ) ) ;
#9146 = CARTESIAN_POINT ( 'NONE',  ( 13.56230152254410903, 5.196152422706636465, -5.475000000000035172 ) ) ;
#9147 = EDGE_LOOP ( 'NONE', ( #2489, #6792, #34926, #17521 ) ) ;
#9148 = CARTESIAN_POINT ( 'NONE',  ( -41.49330436395490551, 210.1155267958017134, -6.500000000000000888 ) ) ;
#9149 = CARTESIAN_POINT ( 'NONE',  ( 22.56230152254467924, 3.464101615137418211, -5.474999998770981868 ) ) ;
#9150 = CARTESIAN_POINT ( 'NONE',  ( -3.796722387233375073, 29.38518628210144712, 8.710071997420127943 ) ) ;
#9151 = CARTESIAN_POINT ( 'NONE',  ( -13.62178482187500528, 196.6343750006145399, -23.59362340125807123 ) ) ;
#9152 = DIRECTION ( 'NONE',  ( 0.000000000000000000, 0.000000000000000000, 1.000000000000000000 ) ) ;
#9153 = DIRECTION ( 'NONE',  ( 0.08715574274765150453, 0.000000000000000000, 0.9961946980917461003 ) ) ;
#9154 = CARTESIAN_POINT ( 'NONE',  ( 10.56230152254410726, 0.000000000000000000, -5.850000000000049383 ) ) ;
#9155 = CARTESIAN_POINT ( 'NONE',  ( 37.39010055343310768, 3.464101615137841872, 168.4974270992498475 ) ) ;
#9156 = CARTESIAN_POINT ( 'NONE',  ( 26.75643035624999655, 245.5468750006145342, 3.323476615752267715 ) ) ;
#9157 = CARTESIAN_POINT ( 'NONE',  ( 6.840914352311949109, 85.83981371789856496, 6.594114490232462877 ) ) ;
#9158 = CARTESIAN_POINT ( 'NONE',  ( 23.87821517812500005, 240.1093750006145342, 4.985214923628404016 ) ) ;
#9159 = ORIENTED_EDGE ( 'NONE', *, *, #37039, .F. ) ;
#9160 = CARTESIAN_POINT ( 'NONE',  ( -54.35788769728821279, 216.4690446883607535, 1.857196546604031662 ) ) ;
#9161 = CARTESIAN_POINT ( 'NONE',  ( 18.00000000000000355, 247.4312500012290457, 5.196152422706632912 ) ) ;
#9162 = CARTESIAN_POINT ( 'NONE',  ( -6.932735513424201912, 97.05231371789855643, 10.69584247140429412 ) ) ;
#9163 = EDGE_CURVE ( 'NONE', #16244, #17027, #5735, .T. ) ;
#9164 = CARTESIAN_POINT ( 'NONE',  ( 22.80587116629411781, -3.604726614523238837, -2.709374999385515181 ) ) ;
#9165 = CARTESIAN_POINT ( 'NONE',  ( 27.50636891564131759, 5.407089921784856479, 160.1866008677275772 ) ) ;
#9166 = CARTESIAN_POINT ( 'NONE',  ( 23.87821517812499650, 4.985214923628404904, -2.203124999385491556 ) ) ;
#9167 = CARTESIAN_POINT ( 'NONE',  ( -11.61527771782809282, 62.26481371789854791, -4.622313124798832717 ) ) ;
#9168 = CARTESIAN_POINT ( 'NONE',  ( 27.24356964375000700, 198.2468750006145513, 15.72908226750537075 ) ) ;
#9169 = EDGE_LOOP ( 'NONE', ( #35167, #13770, #16487, #25746 ) ) ;
#9170 = ORIENTED_EDGE ( 'NONE', *, *, #4266, .T. ) ;
#9171 = CARTESIAN_POINT ( 'NONE',  ( 20.99999999999999645, -6.646953231504538984, -4.078124999385484450 ) ) ;
#9172 = CARTESIAN_POINT ( 'NONE',  ( 36.59262550718515428, 7.347880794884125653E-16, 159.3822456104860237 ) ) ;
#9173 = CARTESIAN_POINT ( 'NONE',  ( 15.24356964375000167, 246.6343750006145115, 3.323476615752272600 ) ) ;
#9174 = ADVANCED_FACE ( 'NONE', ( #14650 ), #11989, .F. ) ;
#9175 = CARTESIAN_POINT ( 'NONE',  ( -10.69584247140444866, 39.44768628210145067, 6.932735513423972762 ) ) ;
#9176 = CARTESIAN_POINT ( 'NONE',  ( -45.44419563604516554, 203.5000000000000000, 0.1155267958017914542 ) ) ;
#9177 = CARTESIAN_POINT ( 'NONE',  ( -63.85044563604516554, 205.1570982666397072, -4.673758765035155527 ) ) ;
#9178 = APPLICATION_PROTOCOL_DEFINITION ( 'draft international standard', 'automotive_design', 1998, #21674 ) ;
#9179 = CARTESIAN_POINT ( 'NONE',  ( 36.72009078106068358, 7.347880794884117764E-16, 160.8391803576695622 ) ) ;
#9180 = CARTESIAN_POINT ( 'NONE',  ( 12.46528703574811558, 93.60231371789855359, -2.660918448318005503 ) ) ;
#9181 = CARTESIAN_POINT ( 'NONE',  ( -60.09747103062157692, 212.3500491399821613, -3.839350919129076445 ) ) ;
#9182 = CARTESIAN_POINT ( 'NONE',  ( -33.37872103062156981, 201.4690446883607819, 2.162041339862843525 ) ) ;
#9183 = EDGE_CURVE ( 'NONE', #28874, #15760, #17880, .T. ) ;
#9184 = CARTESIAN_POINT ( 'NONE',  ( 18.12178482187500350, -4.985214923628407568, -7.378124999385477167 ) ) ;
#9185 = DIRECTION ( 'NONE',  ( -1.000000000000000000, 0.000000000000000000, 0.000000000000000000 ) ) ;
#9186 = CARTESIAN_POINT ( 'NONE',  ( -14.25334919248795096, 70.31481371789853085, 6.092822981423662299 ) ) ;
#9187 = CARTESIAN_POINT ( 'NONE',  ( -59.10044563604517265, 203.6929966515019430, -6.137860380172892150 ) ) ;
#9188 = AXIS2_PLACEMENT_3D ( 'NONE', #9942, #9199, #26621 ) ;
#9189 = VERTEX_POINT ( 'NONE', #26390 ) ;
#9190 = CYLINDRICAL_SURFACE ( 'NONE', #13197, 5.999999999999998224 ) ;
#9191 = CARTESIAN_POINT ( 'NONE',  ( -4.944772684328673229, 102.9851862821014663, 11.48171059495397728 ) ) ;
#9192 = CARTESIAN_POINT ( 'NONE',  ( 13.04141134922759804, 45.77268628210144641, 8.927990412390657937 ) ) ;
#9193 = DIRECTION ( 'NONE',  ( 1.000000000000000000, 0.000000000000000000, 0.000000000000000000 ) ) ;
#9194 = DIRECTION ( 'NONE',  ( -0.000000000000000000, 1.000000000000000000, -0.000000000000000000 ) ) ;
#9195 = CARTESIAN_POINT ( 'NONE',  ( 15.46528703574804986, 54.39768628210144641, 3.257655550457285720 ) ) ;
#9196 = CARTESIAN_POINT ( 'NONE',  ( 26.99999999999999645, 247.0937500012290400, 3.464101615137751278 ) ) ;
#9197 = EDGE_CURVE ( 'NONE', #8211, #13498, #33794, .T. ) ;
#9198 = CARTESIAN_POINT ( 'NONE',  ( 22.80587116629410716, 3.604726614523238837, -8.878124999385544669 ) ) ;
#9199 = DIRECTION ( 'NONE',  ( -0.000000000000000000, -1.000000000000000000, -0.000000000000000000 ) ) ;
#9200 = CARTESIAN_POINT ( 'NONE',  ( -49.60788769728823411, 216.4690446883607535, 1.857196546604031662 ) ) ;
#9201 = CARTESIAN_POINT ( 'NONE',  ( 10.41621459261286198, -0.7567938363388677647, -9.999999999999998224 ) ) ;
#9202 = CARTESIAN_POINT ( 'NONE',  ( 2.311890736173175753, 46.92268628210145209, 12.53471296425194836 ) ) ;
#9203 = CARTESIAN_POINT ( 'NONE',  ( -9.500000000000005329, 3.510186282101451560, -0.1745138560725176813 ) ) ;
#9204 = CARTESIAN_POINT ( 'NONE',  ( 15.24356964375000167, 246.7468750006145797, 3.323476615752272600 ) ) ;
#9205 = EDGE_LOOP ( 'NONE', ( #23577, #31014, #20897, #8795 ) ) ;
#9206 = CARTESIAN_POINT ( 'NONE',  ( 21.00000000000000000, 6.928203230275506996, -6.412499999999995204 ) ) ;
#9207 = CARTESIAN_POINT ( 'NONE',  ( 19.39230484541326760, 245.1986538117967029, 5.999999999999999112 ) ) ;
#9208 = CARTESIAN_POINT ( 'NONE',  ( 7.234628195640295800, 197.4325961894323882, 27.00000000000001066 ) ) ;
#9209 = CARTESIAN_POINT ( 'NONE',  ( 22.80587116629411426, 3.604726614523238837, -3.928124999385561367 ) ) ;
#9210 = CARTESIAN_POINT ( 'NONE',  ( 34.42560472746153977, 5.407089921784857367, 167.6369003702161251 ) ) ;
#9211 = CARTESIAN_POINT ( 'NONE',  ( 26.99999999999999645, 241.2624999999999886, -3.464101615137755275 ) ) ;
#9212 = CARTESIAN_POINT ( 'NONE',  ( 27.00000000000001066, 198.8374999999999773, 15.58845726811988897 ) ) ;
#9213 = CARTESIAN_POINT ( 'NONE',  ( 7.228626920339069173, 52.67268628210145209, -10.49813415415989404 ) ) ;
#9214 = ORIENTED_EDGE ( 'NONE', *, *, #728, .T. ) ;
#9215 = ORIENTED_EDGE ( 'NONE', *, *, #12423, .T. ) ;
#9216 = CARTESIAN_POINT ( 'NONE',  ( 24.62848410913218800, 0.000000000000000000, 160.3160426211468348 ) ) ;
#9217 = CARTESIAN_POINT ( 'NONE',  ( 30.57623723450533504, -6.928203230275506996, 159.4568924540549517 ) ) ;
#9218 = CARTESIAN_POINT ( 'NONE',  ( 24.56230152254410726, 0.000000000000000000, -10.00000000000000000 ) ) ;
#9219 = CARTESIAN_POINT ( 'NONE',  ( 26.75643035624999655, -3.323476615752267715, -5.353124999385477700 ) ) ;
#9220 = CARTESIAN_POINT ( 'NONE',  ( 12.50000000000000355, 90.91018628210146346, 0.1745138560725507937 ) ) ;
#9221 = CARTESIAN_POINT ( 'NONE',  ( 5.770363421894130873, 27.76481371789854791, -14.38691631536193860 ) ) ;
#9222 = CARTESIAN_POINT ( 'NONE',  ( 21.00000000000000000, 240.2968750006145342, -6.646953231504538984 ) ) ;
#9223 = CARTESIAN_POINT ( 'NONE',  ( -34.36830436395490551, 209.8844732041982297, 4.499999999999996447 ) ) ;
#9224 = LINE ( 'NONE', #20990, #13139 ) ;
#9225 = CARTESIAN_POINT ( 'NONE',  ( 30.62771359501211066, -7.209453229046482114, 160.0452699470032485 ) ) ;
#9226 = CARTESIAN_POINT ( 'NONE',  ( -6.840914352311947333, 26.03981371789855714, -6.594114490232462877 ) ) ;
#9227 = CARTESIAN_POINT ( 'NONE',  ( -62.86830436395490551, 209.8844732041982581, 6.500000000000000888 ) ) ;
#9228 = CARTESIAN_POINT ( 'NONE',  ( -66.43080436395490551, 201.5000000000000000, -0.1155267958017054536 ) ) ;
#9229 = DIRECTION ( 'NONE',  ( 0.000000000000000000, 0.000000000000000000, 1.000000000000000000 ) ) ;
#9230 = DIRECTION ( 'NONE',  ( 0.000000000000000000, 0.000000000000000000, 1.000000000000000000 ) ) ;
#9231 = CARTESIAN_POINT ( 'NONE',  ( -13.62178482187498396, 196.7843750006145456, 23.59362340125808188 ) ) ;
#9232 = CARTESIAN_POINT ( 'NONE',  ( -8.632099005475794229, 124.6523137178985650, 13.23911966647199812 ) ) ;
#9233 = CARTESIAN_POINT ( 'NONE',  ( -61.67336230271183695, 215.6869285224997270, 3.149950860017831200 ) ) ;
#9234 = EDGE_CURVE ( 'NONE', #13579, #6071, #18891, .T. ) ;
#9235 = ORIENTED_EDGE ( 'NONE', *, *, #33533, .F. ) ;
#9236 = EDGE_CURVE ( 'NONE', #25827, #1351, #25523, .T. ) ;
#9237 = CARTESIAN_POINT ( 'NONE',  ( 12.50000000000000355, 54.11018628210144499, 0.1745138560725507937 ) ) ;
#9238 = CARTESIAN_POINT ( 'NONE',  ( 23.99999999999999645, 245.4062500012290400, -5.196152422706631135 ) ) ;
#9239 = CIRCLE ( 'NONE', #36471, 5.999999999999999112 ) ;
#9240 = CARTESIAN_POINT ( 'NONE',  ( 20.16825598028117028, 5.708404836608378830, -8.000000000000001776 ) ) ;
#9241 = CARTESIAN_POINT ( 'NONE',  ( 28.08976766865841057, 5.407089921784862696, 166.8548791280792045 ) ) ;
#9242 = CARTESIAN_POINT ( 'NONE',  ( 26.99999999999999645, 7.347880794884117764E-16, -2.868749998770958598 ) ) ;
#9243 = EDGE_CURVE ( 'NONE', #10376, #17383, #22569, .T. ) ;
#9244 = CARTESIAN_POINT ( 'NONE',  ( 10.31873187879410914, 0.000000000000000000, -1.490624999385542493 ) ) ;
#9245 = CARTESIAN_POINT ( 'NONE',  ( -3.474262827703337830, 60.43518628210146204, -8.843639120294326972 ) ) ;
#9246 = CARTESIAN_POINT ( 'NONE',  ( 26.99999999999999289, 0.000000000000000000, -8.000000000000000000 ) ) ;
#9247 = CARTESIAN_POINT ( 'NONE',  ( 20.99999999999999289, 245.8374999999999773, -5.999999999999997335 ) ) ;
#9248 = ADVANCED_FACE ( 'NONE', ( #32079 ), #3081, .F. ) ;
#9249 = CARTESIAN_POINT ( 'NONE',  ( -4.944772684328673229, 102.9851862821014663, 11.48171059495397728 ) ) ;
#9250 = CARTESIAN_POINT ( 'NONE',  ( 7.234628195640322446, 199.3450961906613657, 26.99999999999999645 ) ) ;
#9251 = CARTESIAN_POINT ( 'NONE',  ( 0.000000000000000000, 200.0000000000000000, -27.00000000000000355 ) ) ;
#9252 = CARTESIAN_POINT ( 'NONE',  ( -79.65000000000001990, 210.0000000000000000, -5.000000000000001776 ) ) ;
#9253 = CARTESIAN_POINT ( 'NONE',  ( 28.41593846164884241, 5.957544813848093312, 159.6438083957854133 ) ) ;
#9254 = CARTESIAN_POINT ( 'NONE',  ( 15.24356964375000167, -3.323476615752272600, -9.553124999385460114 ) ) ;
#9255 = CARTESIAN_POINT ( 'NONE',  ( 37.34761212884377812, 7.347880794884117764E-16, 168.0117821839301087 ) ) ;
#9256 = CARTESIAN_POINT ( 'NONE',  ( 27.97210741594907901, 5.407089921784862696, 165.5100162856553538 ) ) ;
#9257 = PRODUCT_DEFINITION_CONTEXT ( 'detailed design', #23111, 'design' ) ;
#9258 = CARTESIAN_POINT ( 'NONE',  ( 24.97165984609394940, 0.000000000000000000, 164.2385592436587558 ) ) ;
#9259 = CARTESIAN_POINT ( 'NONE',  ( 25.16776026727616511, 0.000000000000000000, 166.4799973143651926 ) ) ;
#9260 = CARTESIAN_POINT ( 'NONE',  ( 15.00000000000000000, 249.5125000000000171, -3.464101615137752166 ) ) ;
#9261 = CARTESIAN_POINT ( 'NONE',  ( 27.24356964375000700, 196.3906250006145342, 15.72908226750537075 ) ) ;
#9262 = CARTESIAN_POINT ( 'NONE',  ( -12.53471296425189152, 98.77731371789855075, -2.311890736173453753 ) ) ;
#9263 = CARTESIAN_POINT ( 'NONE',  ( -2.660918448318275509, 102.6976862821014578, 12.46528703574805874 ) ) ;
#9265 = ORIENTED_EDGE ( 'NONE', *, *, #1898, .F. ) ;
#9264 = VERTEX_POINT ( 'NONE', #9154 ) ;
#9266 = CARTESIAN_POINT ( 'NONE',  ( 5.778771075727756162E-15, 196.3156250006145171, 31.45816453501075927 ) ) ;
#9267 = CARTESIAN_POINT ( 'NONE',  ( 36.91619120224290640, 7.347880794884117764E-16, 163.0806184283759706 ) ) ;
#9268 = CARTESIAN_POINT ( 'NONE',  ( -6.092822981423666739, 81.81481371789855928, -14.25334919248795096 ) ) ;
#9269 = CIRCLE ( 'NONE', #7434, 2.649999999999990585 ) ;
#9270 = CARTESIAN_POINT ( 'NONE',  ( 21.00000000000000000, 6.646953231504538984, -3.065624999385470062 ) ) ;
#9271 = CARTESIAN_POINT ( 'NONE',  ( 21.00000000000000000, 246.8218750006145399, 6.646953231504538984 ) ) ;
#9272 = CARTESIAN_POINT ( 'NONE',  ( -9.465287035748065847, 104.9976862821014549, -2.064181346179273735 ) ) ;
#9273 = PRODUCT_DEFINITION_SHAPE ( 'NONE', 'NONE',  #18775 ) ;
#9274 = CARTESIAN_POINT ( 'NONE',  ( 27.00000000000000355, 197.6375000012290286, -3.306546357697854128E-15 ) ) ;
#9275 = CARTESIAN_POINT ( 'NONE',  ( 9.500000000000005329, 75.48981371789854222, -0.1745138560723090149 ) ) ;
#9276 = CARTESIAN_POINT ( 'NONE',  ( 16.56230152254411081, -7.209453229046475009, -5.878124999385531346 ) ) ;
#9277 =( BOUNDED_CURVE ( )  B_SPLINE_CURVE ( 2, ( #14789, #25782, #31841, #2081, #23139, #22955, #34870, #17451, #8911 ),
 .UNSPECIFIED., .F., .F. ) 
 B_SPLINE_CURVE_WITH_KNOTS ( ( 3, 2, 2, 2, 3 ),
 ( 0.5208333333333333703, 0.5277777777777777901, 0.5416666666666666297, 0.5555555555555555802, 0.5625000000000000000 ),
 .UNSPECIFIED. ) 
 CURVE ( )  GEOMETRIC_REPRESENTATION_ITEM ( )  RATIONAL_B_SPLINE_CURVE ( ( 0.9330127018922192983, 0.9330127018922198534, 1.000000000000000000, 0.8660254037844387076, 1.000000000000000000, 0.8660254037844387076, 1.000000000000000000, 0.9330127018922194093, 0.9330127018922194093 ) ) 
 REPRESENTATION_ITEM ( '' )  );
#9278 = CARTESIAN_POINT ( 'NONE',  ( 15.24356964374999990, 241.6468750006145285, 0.000000000000000000 ) ) ;
#9279 = CARTESIAN_POINT ( 'NONE',  ( 10.49813415416005213, 56.22731371789854649, -7.228626920338837358 ) ) ;
#9280 = CARTESIAN_POINT ( 'NONE',  ( 24.00000000000000000, -5.196152422706629359, -3.000000000000002665 ) ) ;
#9281 = CARTESIAN_POINT ( 'NONE',  ( -12.50000000000000355, 104.7101862821014606, -0.1745138560725492671 ) ) ;
#9282 = CARTESIAN_POINT ( 'NONE',  ( 10.56230152254410726, 0.000000000000000000, -7.087499998771007448 ) ) ;
#9283 = CARTESIAN_POINT ( 'NONE',  ( -36.74330436395489841, 210.1155267958017134, -6.500000000000000888 ) ) ;
#9284 = CARTESIAN_POINT ( 'NONE',  ( -12.53471296425194836, 141.2226862821014493, 2.311890736173176641 ) ) ;
#9285 = CARTESIAN_POINT ( 'NONE',  ( 37.25443294523552851, 7.646167579472015790E-16, 164.1520909940213642 ) ) ;
#9286 = CARTESIAN_POINT ( 'NONE',  ( 8.632099005475504683, 83.14768628210143220, 13.23911966647218996 ) ) ;
#9287 = CARTESIAN_POINT ( 'NONE',  ( 10.31873187879410736, -3.604726614523244610, -3.309374999385498395 ) ) ;
#9288 = CARTESIAN_POINT ( 'NONE',  ( -11.48171059495397373, 4.085186282101443744, -4.944772684328680334 ) ) ;
#9289 = DIRECTION ( 'NONE',  ( 0.9925324990730152175, -0.1219804832088933616, 0.000000000000000000 ) ) ;
#9290 = CARTESIAN_POINT ( 'NONE',  ( 26.99999999999999645, 7.347880794884117764E-16, -5.568749998770966769 ) ) ;
#9291 = CARTESIAN_POINT ( 'NONE',  ( -6.594114490232312775, 105.8601862821014379, -6.840914352312096547 ) ) ;
#9292 = LINE ( 'NONE', #2521, #2831 ) ;
#9293 =( BOUNDED_CURVE ( )  B_SPLINE_CURVE ( 2, ( #13680, #21648, #7801, #21835, #30555, #24487, #36217, #30170, #7613 ),
 .UNSPECIFIED., .F., .F. ) 
 B_SPLINE_CURVE_WITH_KNOTS ( ( 3, 2, 2, 2, 3 ),
 ( 0.8125000000000000000, 0.8194444444444444198, 0.8333333333333333703, 0.8472222222222222099, 0.8541666666666667407 ),
 .UNSPECIFIED. ) 
 CURVE ( )  GEOMETRIC_REPRESENTATION_ITEM ( )  RATIONAL_B_SPLINE_CURVE ( ( 0.9330127018922194093, 0.9330127018922194093, 1.000000000000000000, 0.8660254037844387076, 1.000000000000000000, 0.8660254037844387076, 1.000000000000000000, 0.9330127018922187432, 0.9330127018922192983 ) ) 
 REPRESENTATION_ITEM ( '' )  );
#9294 = CARTESIAN_POINT ( 'NONE',  ( 14.38691631536207538, 16.73518628210143788, -5.770363421893813793 ) ) ;
#9295 = CIRCLE ( 'NONE', #36436, 5.999999999999994671 ) ;
#9296 = CARTESIAN_POINT ( 'NONE',  ( 13.62178482187501416, 196.8593750006145342, 23.59362340125806767 ) ) ;
#9297 = CARTESIAN_POINT ( 'NONE',  ( 15.24356964374999990, 241.1968750006145115, 0.000000000000000000 ) ) ;
#9298 = VERTEX_POINT ( 'NONE', #15028 ) ;
#9299 = CARTESIAN_POINT ( 'NONE',  ( 31.14247720061542068, -7.209453229046475009, 165.9290448826076272 ) ) ;
#9300 = CARTESIAN_POINT ( 'NONE',  ( 15.24356964374999990, 3.323476615752268604, -1.978124999385461935 ) ) ;
#9301 = CARTESIAN_POINT ( 'NONE',  ( 27.24356964374999279, 199.6718750006145058, -15.72908226750539207 ) ) ;
#9302 = DIRECTION ( 'NONE',  ( 0.000000000000000000, 0.000000000000000000, 1.000000000000000000 ) ) ;
#9303 = CARTESIAN_POINT ( 'NONE',  ( 20.99999999999999645, 185.0294372515228645, -5.999999999999999112 ) ) ;
#9304 = LINE ( 'NONE', #26917, #2896 ) ;
#9305 = CARTESIAN_POINT ( 'NONE',  ( -20.86978604919638869, 194.8026013911397456, -17.51182792271053046 ) ) ;
#9306 = CARTESIAN_POINT ( 'NONE',  ( 6.840914352311949109, 12.23981371789853512, 6.594114490232462877 ) ) ;
#9307 = CARTESIAN_POINT ( 'NONE',  ( 13.62178482187499640, 198.8093750006145513, -23.59362340125807123 ) ) ;
#9308 = EDGE_LOOP ( 'NONE', ( #29771, #19654, #22675, #36227 ) ) ;
#9309 = STYLED_ITEM ( 'NONE', ( #11413 ), #19224 ) ;
#9310 = CARTESIAN_POINT ( 'NONE',  ( 21.00000000000000000, 246.7093750006145285, 6.646953231504538984 ) ) ;
#9311 = CARTESIAN_POINT ( 'NONE',  ( -12.50000000000000355, 43.28981371789855359, 0.1745138560722786503 ) ) ;
#9312 = CARTESIAN_POINT ( 'NONE',  ( 21.00000000000000000, -6.646953231504538984, -0.4781249993854547187 ) ) ;
#9313 = CARTESIAN_POINT ( 'NONE',  ( 14.38691631536194393, 122.0648137178985877, 5.770363421894124656 ) ) ;
#9314 = CARTESIAN_POINT ( 'NONE',  ( 18.00000000000000355, -5.196152422706632912, -6.168749998770955756 ) ) ;
#9315 = CARTESIAN_POINT ( 'NONE',  ( 22.60769515458672885, 247.8825961894323484, 5.999999999999997335 ) ) ;
#9316 = EDGE_LOOP ( 'NONE', ( #2845, #1422, #28655, #10247 ) ) ;
#9317 = CARTESIAN_POINT ( 'NONE',  ( 10.31873187879410381, 3.604726614523240613, -3.384374999385492799 ) ) ;
#9318 = CARTESIAN_POINT ( 'NONE',  ( 27.24356964375000345, 197.7781250006145228, -3.336375036156643733E-15 ) ) ;
#9319 = CARTESIAN_POINT ( 'NONE',  ( 24.67263818733777470, 0.000000000000000000, 163.6153742921546836 ) ) ;
#9320 = APPLICATION_CONTEXT ( 'automotive_design' ) ;
#9321 = CARTESIAN_POINT ( 'NONE',  ( -65.03794563604515133, 203.8621396198271043, 6.307003348498029460 ) ) ;
#9322 = CARTESIAN_POINT ( 'NONE',  ( 19.39230484541324984, 245.6486538117966916, 5.999999999999991118 ) ) ;
#9323 = CARTESIAN_POINT ( 'NONE',  ( -13.50000000000000533, 199.1375000012290286, -23.38268590217984411 ) ) ;
#9324 = CARTESIAN_POINT ( 'NONE',  ( -62.06919563604516554, 214.5000000000000284, -0.1155267958017627827 ) ) ;
#9325 = CARTESIAN_POINT ( 'NONE',  ( -32.19122103062156981, 208.3738570449993404, -6.530955311639226935 ) ) ;
#9326 = CARTESIAN_POINT ( 'NONE',  ( 24.87037277869651319, 3.604726614523236616, 165.8754910134502722 ) ) ;
#9327 = ORIENTED_EDGE ( 'NONE', *, *, #31021, .F. ) ;
#9328 = CARTESIAN_POINT ( 'NONE',  ( 19.39230484541326405, 248.7424038105677084, 5.999999999999995559 ) ) ;
#9329 = CARTESIAN_POINT ( 'NONE',  ( 14.38691631536207538, 136.3351862821014606, -5.770363421893813793 ) ) ;
#9330 = CARTESIAN_POINT ( 'NONE',  ( -62.86830436395490551, 209.8844732041983150, 8.500000000000003553 ) ) ;
#9331 =( BOUNDED_CURVE ( )  B_SPLINE_CURVE ( 2, ( #36839, #21712, #33262, #22085, #19254 ),
 .UNSPECIFIED., .F., .F. ) 
 B_SPLINE_CURVE_WITH_KNOTS ( ( 3, 2, 3 ),
 ( 0.000000000000000000, 0.007246376811594202987, 0.01086956521739129364 ),
 .UNSPECIFIED. ) 
 CURVE ( )  GEOMETRIC_REPRESENTATION_ITEM ( )  RATIONAL_B_SPLINE_CURVE ( ( 1.000000000000000000, 0.8660254037844387076, 1.000000000000000000, 0.9330127018922196314, 0.9330127018922194093 ) ) 
 REPRESENTATION_ITEM ( '' )  );
#9332 = MECHANICAL_DESIGN_GEOMETRIC_PRESENTATION_REPRESENTATION (  '', ( #3886 ), #34137 ) ;
#9333 = CARTESIAN_POINT ( 'NONE',  ( 8.152565276336714462, 136.0476862821014379, -5.233372021372432847 ) ) ;
#9334 = VECTOR ( 'NONE', #701, 1000.000000000000114 ) ;
#9335 = CARTESIAN_POINT ( 'NONE',  ( 0.000000000000000000, -30.00000000000000000, 0.000000000000000000 ) ) ;
#9336 = CARTESIAN_POINT ( 'NONE',  ( 4.622313124798573369, 28.23518628210144854, 11.61527771782819940 ) ) ;
#9337 = COLOUR_RGB ( '',0.8941176470588234615, 0.8941176470588234615, 0.8941176470588234615 ) ;
#9338 = CARTESIAN_POINT ( 'NONE',  ( 22.56230152254411792, 3.464101615137759271, -6.487500000000020250 ) ) ;
#9339 = EDGE_LOOP ( 'NONE', ( #33249, #23101, #22001, #21854 ) ) ;
#9340 = CARTESIAN_POINT ( 'NONE',  ( -8.927990412390661490, 121.6726862821014521, 13.04141134922759804 ) ) ;
#9341 = CARTESIAN_POINT ( 'NONE',  ( 15.00000000000000000, 242.3125000000000000, -3.464101615137752610 ) ) ;
#9342 = CARTESIAN_POINT ( 'NONE',  ( -0.1745138560725182642, 10.41018628210144037, 9.500000000000005329 ) ) ;
#9343 = CARTESIAN_POINT ( 'NONE',  ( 5.778771075727756162E-15, 198.1156250006145285, 31.45816453501075927 ) ) ;
#9344 = LINE ( 'NONE', #15412, #18395 ) ;
#9345 = CARTESIAN_POINT ( 'NONE',  ( 22.45414455245212793, -1.393728951354829659, -10.00000000000000533 ) ) ;
#9346 = CARTESIAN_POINT ( 'NONE',  ( 33.64652983760650073, -5.196152422706629359, 160.1293577552730483 ) ) ;
#9347 = CARTESIAN_POINT ( 'NONE',  ( 23.87821517812499650, 242.5093750006145399, -4.985214923628404904 ) ) ;
#9348 = CARTESIAN_POINT ( 'NONE',  ( 7.954856959092311719, 83.82731371789856212, -5.529263428287300108 ) ) ;
#9349 = CARTESIAN_POINT ( 'NONE',  ( 26.75643035624999655, 240.1468750006145569, 3.323476615752267271 ) ) ;
#9350 = ORIENTED_EDGE ( 'NONE', *, *, #12350, .F. ) ;
#9351 = CARTESIAN_POINT ( 'NONE',  ( 23.99999999999999645, 245.4062500012290400, -5.196152422706631135 ) ) ;
#9352 = CARTESIAN_POINT ( 'NONE',  ( -7.228626920338836470, 90.72731371789855359, -10.49813415416005213 ) ) ;
#9353 = CARTESIAN_POINT ( 'NONE',  ( 22.80587116629412137, 7.646167579472024665E-16, -4.021874999385527616 ) ) ;
#9354 = LINE ( 'NONE', #6507, #22153 ) ;
#9355 = CARTESIAN_POINT ( 'NONE',  ( 23.87821517812500005, -4.985214923628404016, -5.503124999385489602 ) ) ;
#9356 = CARTESIAN_POINT ( 'NONE',  ( 8.962234695871567070, 67.43981371789855928, 8.715434833792127023 ) ) ;
#9357 = CARTESIAN_POINT ( 'NONE',  ( 13.62178482187501416, 198.6593750006145456, 23.59362340125806767 ) ) ;
#9358 = ORIENTED_EDGE ( 'NONE', *, *, #19362, .F. ) ;
#9359 = ORIENTED_EDGE ( 'NONE', *, *, #23079, .F. ) ;
#9360 = CARTESIAN_POINT ( 'NONE',  ( 20.99999999999999645, -6.646953231504538984, -4.978124999385475036 ) ) ;
#9361 = CARTESIAN_POINT ( 'NONE',  ( 10.56230152254410903, 0.000000000000000000, -6.187499998771023080 ) ) ;
#9362 = CARTESIAN_POINT ( 'NONE',  ( 21.00000000000000000, 245.5843750006145569, -6.646953231504538984 ) ) ;
#9363 = CARTESIAN_POINT ( 'NONE',  ( 0.1745138560725515708, 33.41018628210144925, -12.50000000000000355 ) ) ;
#9364 = EDGE_CURVE ( 'NONE', #1475, #3147, #20916, .T. ) ;
#9365 = CARTESIAN_POINT ( 'NONE',  ( -34.16294563604515844, 214.6737587650350747, -4.842901733360248429 ) ) ;
#9366 = CARTESIAN_POINT ( 'NONE',  ( 20.21461154673354699, 212.0943692086927399, -5.961323472698028425 ) ) ;
#9367 = CARTESIAN_POINT ( 'NONE',  ( -68.00669563604516554, 209.8844732041982013, -6.500000000000000888 ) ) ;
#9368 = CARTESIAN_POINT ( 'NONE',  ( 36.80179928988660976, 3.464101615137755275, 161.7731128871305657 ) ) ;
#9369 = CARTESIAN_POINT ( 'NONE',  ( 8.715434833792128799, 83.53981371789856780, -8.962234695871567070 ) ) ;
#9370 = CARTESIAN_POINT ( 'NONE',  ( -55.34747103062157692, 212.3500491399821613, -3.839350919129076445 ) ) ;
#9371 = CARTESIAN_POINT ( 'NONE',  ( -67.81622103062156270, 211.6261429550005744, 6.530955311639227823 ) ) ;
#9372 = EDGE_CURVE ( 'NONE', #8155, #25296, #607, .T. ) ;
#9373 = CARTESIAN_POINT ( 'NONE',  ( 15.24356964375000167, -3.323476615752272600, -7.865624999385466332 ) ) ;
#9374 = CYLINDRICAL_SURFACE ( 'NONE', #27078, 5.999999999999998224 ) ;
#9375 = CARTESIAN_POINT ( 'NONE',  ( 8.632099005475788900, 64.85231371789855359, -13.23911966647199812 ) ) ;
#9376 = CARTESIAN_POINT ( 'NONE',  ( -52.56919563604517265, 218.5000000000000000, -0.1155267958018185298 ) ) ;
#9377 = LINE ( 'NONE', #3683, #25906 ) ;
#9378 = CARTESIAN_POINT ( 'NONE',  ( -6.932735513423968321, 78.54768628210146630, -10.69584247140445221 ) ) ;
#9379 = CARTESIAN_POINT ( 'NONE',  ( -15.46528703574804986, 40.59768628210144215, -3.257655550457287497 ) ) ;
#9380 = DIRECTION ( 'NONE',  ( 1.000000000000000000, 0.000000000000000000, 0.000000000000000000 ) ) ;
#9381 = CARTESIAN_POINT ( 'NONE',  ( 27.50146640511176344, 5.407089921784862696, 160.1305649159599227 ) ) ;
#9382 = CARTESIAN_POINT ( 'NONE',  ( -13.23911966647218463, 48.64768628210144641, 8.632099005475506459 ) ) ;
#9383 = CARTESIAN_POINT ( 'NONE',  ( 37.03385145495223441, 7.347880794884117764E-16, 164.4254812707998497 ) ) ;
#9384 = ADVANCED_FACE ( 'NONE', ( #32455 ), #34735, .T. ) ;
#9385 = CARTESIAN_POINT ( 'NONE',  ( 16.56230152254411436, -7.209453229046475009, -9.928124999385525840 ) ) ;
#9386 = VECTOR ( 'NONE', #3463, 1000.000000000000000 ) ;
#9387 = CARTESIAN_POINT ( 'NONE',  ( 13.56230152254411436, -5.196152422706638241, -2.625000000000043965 ) ) ;
#9388 = CARTESIAN_POINT ( 'NONE',  ( -56.13913769728823411, 206.8500491399821044, -5.686928522499717253 ) ) ;
#9389 = CARTESIAN_POINT ( 'NONE',  ( 31.37044394018620252, 6.928203230275514990, 168.5347166391916574 ) ) ;
#9390 = CARTESIAN_POINT ( 'NONE',  ( 7.228626920339068285, 15.87268628210144961, -10.49813415415989581 ) ) ;
#9391 = CARTESIAN_POINT ( 'NONE',  ( 9.000000000000003553, 242.0000000000000000, 6.000000000000000888 ) ) ;
#9392 = CARTESIAN_POINT ( 'NONE',  ( 3.796722387233182339, 141.6148137178985849, 8.710071997420207879 ) ) ;
#9393 = CARTESIAN_POINT ( 'NONE',  ( 20.99999999999999645, 247.4968750006145513, -6.646953231504538984 ) ) ;
#9394 = ORIENTED_EDGE ( 'NONE', *, *, #412, .F. ) ;
#9395 = CARTESIAN_POINT ( 'NONE',  ( 21.00000000000000000, 6.928203230275506996, -5.962499999999998579 ) ) ;
#9396 = DIRECTION ( 'NONE',  ( 1.000000000000000000, 0.000000000000000000, 0.000000000000000000 ) ) ;
#9397 = CARTESIAN_POINT ( 'NONE',  ( 0.000000000000000000, 195.0000000000000000, 0.000000000000000000 ) ) ;
#9398 = CARTESIAN_POINT ( 'NONE',  ( 16.56230152254410015, -7.209453229046475009, -4.078124999385484450 ) ) ;
#9399 = CARTESIAN_POINT ( 'NONE',  ( 24.90959286293295349, 3.604726614523236616, 166.3237786275915937 ) ) ;
#9400 = CARTESIAN_POINT ( 'NONE',  ( 15.00000000000000000, 240.9624999999999773, -3.464101615137752166 ) ) ;
#9401 = CARTESIAN_POINT ( 'NONE',  ( -8.871188430189180352, 219.1704066634408434, 3.236079657462661796 ) ) ;
#9402 = CARTESIAN_POINT ( 'NONE',  ( -11.48171059495397373, 40.88518628210144357, -4.944772684328680334 ) ) ;
#9403 = VERTEX_POINT ( 'NONE', #11432 ) ;
#9404 = ORIENTED_EDGE ( 'NONE', *, *, #36505, .F. ) ;
#9405 = CARTESIAN_POINT ( 'NONE',  ( 22.56230152254411792, 7.347880794884125653E-16, -5.175000000000040679 ) ) ;
#9406 = DIRECTION ( 'NONE',  ( 0.08715574274765150453, 0.000000000000000000, 0.9961946980917461003 ) ) ;
#9407 = CARTESIAN_POINT ( 'NONE',  ( 13.49999999999999645, 195.3500000000000227, -23.38268590217984766 ) ) ;
#9408 = CARTESIAN_POINT ( 'NONE',  ( 26.75643035624999655, 3.323476615752271712, -6.628124999385471838 ) ) ;
#9409 = CARTESIAN_POINT ( 'NONE',  ( 11.61527771782819940, 90.33518628210144641, -4.622313124798573369 ) ) ;
#9410 = CARTESIAN_POINT ( 'NONE',  ( -3.257655550456946880, 17.70231371789854435, -15.46528703574811736 ) ) ;
#9411 = CARTESIAN_POINT ( 'NONE',  ( 21.00000000000000355, 0.000000000000000000, 50.00000000000001421 ) ) ;
#9412 = CARTESIAN_POINT ( 'NONE',  ( 18.12178482187499640, 241.2343750006145342, -4.985214923628404904 ) ) ;
#9413 = CARTESIAN_POINT ( 'NONE',  ( -35.35788769728823411, 214.4690446883608104, 1.321298161741840893 ) ) ;
#9414 = CARTESIAN_POINT ( 'NONE',  ( -5.352125845617103472, 223.7130433768494129, 2.500000000000000000 ) ) ;
#9415 = CARTESIAN_POINT ( 'NONE',  ( 36.85406125198851157, -3.604726614523238837, 159.5758215996624187 ) ) ;
#9416 = CARTESIAN_POINT ( 'NONE',  ( 4.944772684328420986, 141.6148137178985849, 11.48171059495408208 ) ) ;
#9417 = EDGE_CURVE ( 'NONE', #6556, #19909, #1301, .T. ) ;
#9418 = CARTESIAN_POINT ( 'NONE',  ( -61.08705436395488420, 205.3262412349647263, -4.842901733360204020 ) ) ;
#9419 = CARTESIAN_POINT ( 'NONE',  ( -31.98586230271182984, 205.8500491399821613, 7.418979330068642852 ) ) ;
#9420 = APPLICATION_PROTOCOL_DEFINITION ( 'draft international standard', 'automotive_design', 1998, #6891 ) ;
#9421 = CARTESIAN_POINT ( 'NONE',  ( 20.99999999999999289, 240.8874999999999886, -5.999999999999997335 ) ) ;
#9422 = CARTESIAN_POINT ( 'NONE',  ( -27.24356964374999635, 198.4906250006145569, 15.72908226750539384 ) ) ;
#9423 = CARTESIAN_POINT ( 'NONE',  ( 15.50000000000000533, 139.8898137178985621, -0.1745138560722452326 ) ) ;
#9424 = CARTESIAN_POINT ( 'NONE',  ( -56.52752896937850124, 213.3500491399821613, 5.571401726697954970 ) ) ;
#9425 = ORIENTED_EDGE ( 'NONE', *, *, #1060, .T. ) ;
#9426 = CARTESIAN_POINT ( 'NONE',  ( -11.61527771782819940, 39.73518628210144499, 4.622313124798574258 ) ) ;
#9427 = LINE ( 'NONE', #32539, #11419 ) ;
#9428 = CARTESIAN_POINT ( 'NONE',  ( 37.40314243129871841, -3.604726614523238837, 165.8518481976404360 ) ) ;
#9429 = CARTESIAN_POINT ( 'NONE',  ( 0.1745138560725837118, 97.81018628210145494, -15.50000000000000533 ) ) ;
#9430 = CARTESIAN_POINT ( 'NONE',  ( -63.65997103062156981, 215.5714017266979852, 3.350049139982118618 ) ) ;
#9431 = CARTESIAN_POINT ( 'NONE',  ( 22.80587116629410716, -3.604726614523235284, -0.8531249993855525293 ) ) ;
#9432 = CARTESIAN_POINT ( 'NONE',  ( 8.710071997420127943, 54.68518628210145494, 3.796722387233375073 ) ) ;
#9433 = CARTESIAN_POINT ( 'NONE',  ( 19.39230484541326049, 240.5138461906613827, -5.999999999999997335 ) ) ;
#9434 = LINE ( 'NONE', #29327, #32953 ) ;
#9435 = CARTESIAN_POINT ( 'NONE',  ( -7.228626920339069173, 94.07268628210145778, 10.49813415415989581 ) ) ;
#9436 = CARTESIAN_POINT ( 'NONE',  ( 27.67916667000801212, 5.196152422706636465, 160.7643641140699344 ) ) ;
#9437 = CARTESIAN_POINT ( 'NONE',  ( 13.50000000000001421, 198.4625000012290172, 23.38268590217984055 ) ) ;
#9438 = DIRECTION ( 'NONE',  ( 1.000000000000000000, 0.000000000000000000, 0.000000000000000000 ) ) ;
#9439 = CARTESIAN_POINT ( 'NONE',  ( 27.51944227705346790, -5.407089921784859143, 160.3360300724413321 ) ) ;
#9440 = CARTESIAN_POINT ( 'NONE',  ( 18.12178482187499640, 4.985214923628404904, -9.665624999385475036 ) ) ;
#9441 = CARTESIAN_POINT ( 'NONE',  ( 37.35088046919665317, 3.464101615137854751, 168.0491394851085829 ) ) ;
#9442 = CARTESIAN_POINT ( 'NONE',  ( 31.09835460584942624, -7.209453229046482114, 165.4247213166986796 ) ) ;
#9443 = CARTESIAN_POINT ( 'NONE',  ( 30.95863305570354385, -6.928203230275514990, 163.8276966907081658 ) ) ;
#9444 = DIRECTION ( 'NONE',  ( -0.1219804832088935975, -0.9925324990730152175, 0.000000000000000000 ) ) ;
#9445 = CARTESIAN_POINT ( 'NONE',  ( 15.00000000000000000, 247.7125000000000057, -3.464101615137752166 ) ) ;
#9446 = CARTESIAN_POINT ( 'NONE',  ( 13.62178482187499640, 196.0531250006145285, -23.59362340125807123 ) ) ;
#9447 = VECTOR ( 'NONE', #1919, 1000.000000000000000 ) ;
#9448 = EDGE_CURVE ( 'NONE', #25471, #6369, #31707, .T. ) ;
#9449 = CARTESIAN_POINT ( 'NONE',  ( -2.660918448318004614, 109.7023137178985621, -12.46528703574811558 ) ) ;
#9450 = CARTESIAN_POINT ( 'NONE',  ( 8.962234695871762469, 98.96018628210146062, -8.715434833791931624 ) ) ;
#9451 = EDGE_LOOP ( 'NONE', ( #30221, #2316, #13727, #34332 ) ) ;
#9452 = CARTESIAN_POINT ( 'NONE',  ( -1.926257025242585782E-15, 196.5406250006145399, -31.45816453501075927 ) ) ;
#9453 = FACE_OUTER_BOUND ( 'NONE', #12945, .T. ) ;
#9454 = CARTESIAN_POINT ( 'NONE',  ( -2.908627838312453306, 68.87731371789855928, 15.53471296425188797 ) ) ;
#9455 = CARTESIAN_POINT ( 'NONE',  ( 23.87821517812500005, -4.985214923628404016, -5.053124999385483207 ) ) ;
#9456 = CARTESIAN_POINT ( 'NONE',  ( 21.00000000000000000, 247.9468750006145399, -6.646953231504538984 ) ) ;
#9457 = CARTESIAN_POINT ( 'NONE',  ( -8.843639120294326972, 94.93518628210146915, 3.474262827703335166 ) ) ;
#9458 = CIRCLE ( 'NONE', #29444, 5.000000000000000888 ) ;
#9459 = DIRECTION ( 'NONE',  ( -0.000000000000000000, -1.000000000000000000, -0.000000000000000000 ) ) ;
#9460 = EDGE_CURVE ( 'NONE', #23156, #22401, #12899, .T. ) ;
#9461 = CARTESIAN_POINT ( 'NONE',  ( 3.796722387233182339, 58.81481371789855217, 8.710071997420207879 ) ) ;
#9462 = CARTESIAN_POINT ( 'NONE',  ( 22.80587116629410360, -3.604726614523235284, -6.253124999385533123 ) ) ;
#9463 = EDGE_CURVE ( 'NONE', #27676, #12668, #1883, .T. ) ;
#9464 = CARTESIAN_POINT ( 'NONE',  ( -3.796722387233185003, 118.6148137178985706, -8.710071997420207879 ) ) ;
#9465 = CARTESIAN_POINT ( 'NONE',  ( 13.49999999999999645, 198.0500000000000114, -23.38268590217984766 ) ) ;
#9466 = CARTESIAN_POINT ( 'NONE',  ( 4.622313124798831829, 46.16481371789854649, -11.61527771782809282 ) ) ;
#9467 = LINE ( 'NONE', #17753, #8537 ) ;
#9468 = CARTESIAN_POINT ( 'NONE',  ( 4.944772684328679446, 98.38518628210145778, -11.48171059495397373 ) ) ;
#9469 = CARTESIAN_POINT ( 'NONE',  ( 10.56230152254411259, -3.464101615137757051, -5.249999998770995546 ) ) ;
#9470 = CARTESIAN_POINT ( 'NONE',  ( -64.05580436395490551, 214.5000000000000284, 0.1155267958017899832 ) ) ;
#9471 = CARTESIAN_POINT ( 'NONE',  ( -4.944772684328673229, 139.7851862821014493, 11.48171059495397728 ) ) ;
#9472 = CARTESIAN_POINT ( 'NONE',  ( 31.06403703214253653, -7.209453229046475009, 165.0324696543250411 ) ) ;
#9473 = CARTESIAN_POINT ( 'NONE',  ( -13.04141134922759804, 87.17268628210142367, -8.927990412390657937 ) ) ;
#9474 = CARTESIAN_POINT ( 'NONE',  ( 22.80587116629412137, 7.646167579472024665E-16, -4.021874999385527616 ) ) ;
#9475 = CARTESIAN_POINT ( 'NONE',  ( -10.49813415415989404, 4.372686282101439836, -7.228626920339069173 ) ) ;
#9476 = CARTESIAN_POINT ( 'NONE',  ( 10.56230152254410726, 0.000000000000000000, -7.087499998771007448 ) ) ;
#9477 = CARTESIAN_POINT ( 'NONE',  ( 15.00000000000000000, 244.1124999999999829, -3.464101615137752610 ) ) ;
#9478 = CARTESIAN_POINT ( 'NONE',  ( -6.840914352312096547, 121.9601862821014606, 6.594114490232313663 ) ) ;
#9479 = DIRECTION ( 'NONE',  ( 0.000000000000000000, 1.000000000000000000, 0.000000000000000000 ) ) ;
#9480 = CARTESIAN_POINT ( 'NONE',  ( -5.770363421893818234, 5.235186282101429001, -14.38691631536207005 ) ) ;
#9481 = CARTESIAN_POINT ( 'NONE',  ( 13.62178482187501416, 195.5093750006145399, 23.59362340125806767 ) ) ;
#9482 = CARTESIAN_POINT ( 'NONE',  ( 15.24356964374999990, 242.0968750006145171, 0.000000000000000000 ) ) ;
#9483 = VERTEX_POINT ( 'NONE', #32647 ) ;
#9484 = CARTESIAN_POINT ( 'NONE',  ( 31.31896757967941980, 7.209453229046475009, 167.9463391462434174 ) ) ;
#9485 = CARTESIAN_POINT ( 'NONE',  ( 18.12178482187499640, 4.985214923628404904, -3.815624999385480720 ) ) ;
#9486 = AXIS2_PLACEMENT_3D ( 'NONE', #18142, #32340, #23635 ) ;
#9487 = CARTESIAN_POINT ( 'NONE',  ( 22.60769515458672885, 242.6674038105676345, -5.999999999999998224 ) ) ;
#9488 = DIRECTION ( 'NONE',  ( -1.000000000000000000, 0.000000000000000000, 0.000000000000000000 ) ) ;
#9489 = DIRECTION ( 'NONE',  ( 0.08715574274765150453, 0.000000000000000000, 0.9961946980917461003 ) ) ;
#9490 = CARTESIAN_POINT ( 'NONE',  ( 15.00000000000000000, 0.000000000000000000, -7.593749998770965348 ) ) ;
#9491 = DIRECTION ( 'NONE',  ( -0.000000000000000000, -1.000000000000000000, -0.000000000000000000 ) ) ;
#9492 = CARTESIAN_POINT ( 'NONE',  ( 9.500000000000005329, 20.28981371789855004, -0.1745138560723090149 ) ) ;
#9493 = CARTESIAN_POINT ( 'NONE',  ( 13.62178482187501416, 198.2093750006145285, 23.59362340125806767 ) ) ;
#9495 = ORIENTED_EDGE ( 'NONE', *, *, #20078, .F. ) ;
#9494 = ORIENTED_EDGE ( 'NONE', *, *, #34367, .F. ) ;
#9496 = CARTESIAN_POINT ( 'NONE',  ( 15.24356964374999990, 246.1468750006145285, 0.000000000000000000 ) ) ;
#9497 = CARTESIAN_POINT ( 'NONE',  ( 10.49813415416005213, 19.42731371789854933, -7.228626920338837358 ) ) ;
#9498 = CARTESIAN_POINT ( 'NONE',  ( 23.87821517812500005, -4.985214923628404016, -1.340624999385475746 ) ) ;
#9499 = CARTESIAN_POINT ( 'NONE',  ( -13.04141134922778456, 134.4273137178984996, 8.927990412390377273 ) ) ;
#9500 =( BOUNDED_CURVE ( )  B_SPLINE_CURVE ( 2, ( #15693, #24588, #21573, #1834, #10554, #13403, #24952 ),
 .UNSPECIFIED., .F., .F. ) 
 B_SPLINE_CURVE_WITH_KNOTS ( ( 3, 2, 2, 3 ),
 ( 0.8043478260869548757, 0.8115942028985493328, 0.8188405797101435679, 0.8260869565217380250 ),
 .UNSPECIFIED. ) 
 CURVE ( )  GEOMETRIC_REPRESENTATION_ITEM ( )  RATIONAL_B_SPLINE_CURVE ( ( 1.000000000000030864, 0.8660254037844079544, 1.000000000000000000, 0.8660254037844387076, 1.000000000000000000, 0.8660254037844592467, 0.9999999999999794609 ) ) 
 REPRESENTATION_ITEM ( '' )  );
#9501 = ADVANCED_FACE ( 'NONE', ( #13454, #19348 ), #12752, .T. ) ;
#9502 = CARTESIAN_POINT ( 'NONE',  ( 15.00000000000000178, -3.464101615137757051, -8.006249998770949006 ) ) ;
#9503 = DIRECTION ( 'NONE',  ( 0.000000000000000000, -1.000000000000000000, 0.000000000000000000 ) ) ;
#9504 = ORIENTED_EDGE ( 'NONE', *, *, #20322, .T. ) ;
#9505 = CARTESIAN_POINT ( 'NONE',  ( 19.68408634441911431, 5.407089921784862696, -7.096874999385549998 ) ) ;
#9506 = EDGE_LOOP ( 'NONE', ( #27941, #21028, #28460, #9670 ) ) ;
#9507 = CARTESIAN_POINT ( 'NONE',  ( -13.62178482187500528, 197.0281250006145228, -23.59362340125807123 ) ) ;
#9508 = CARTESIAN_POINT ( 'NONE',  ( 24.82951852428355011, 0.000000000000000000, 165.4085247487197989 ) ) ;
#9509 = ADVANCED_FACE ( 'NONE', ( #24320 ), #12565, .F. ) ;
#9510 = CARTESIAN_POINT ( 'NONE',  ( -31.19419563604516910, 203.5000000000000000, 0.1155267958017914542 ) ) ;
#9511 = CARTESIAN_POINT ( 'NONE',  ( 20.99999999999999645, 249.1843750006145513, -6.646953231504538984 ) ) ;
#9512 = VECTOR ( 'NONE', #3435, 1000.000000000000000 ) ;
#9513 = CARTESIAN_POINT ( 'NONE',  ( 22.56230152254225274, -3.464101615138824197, -9.599999998771053811 ) ) ;
#9514 = CARTESIAN_POINT ( 'NONE',  ( -48.01711230271184405, 214.4690446883608104, -1.321298161741814914 ) ) ;
#9515 = FACE_OUTER_BOUND ( 'NONE', #24779, .T. ) ;
#9516 = CARTESIAN_POINT ( 'NONE',  ( 34.30794447475221176, 5.407089921784857367, 166.2920375277922460 ) ) ;
#9517 = ORIENTED_EDGE ( 'NONE', *, *, #7760, .F. ) ;
#9518 =( BOUNDED_CURVE ( )  B_SPLINE_CURVE ( 2, ( #34156, #8201, #19778, #28462, #31314, #20326, #34527, #23345, #5899 ),
 .UNSPECIFIED., .F., .F. ) 
 B_SPLINE_CURVE_WITH_KNOTS ( ( 3, 2, 2, 2, 3 ),
 ( 0.3369565217391304324, 0.3405797101449275499, 0.3478260869565217295, 0.3550724637681159646, 0.3586956521739130266 ),
 .UNSPECIFIED. ) 
 CURVE ( )  GEOMETRIC_REPRESENTATION_ITEM ( )  RATIONAL_B_SPLINE_CURVE ( ( 0.9330127018922194093, 0.9330127018922194093, 1.000000000000000000, 0.8660254037844387076, 1.000000000000000000, 0.8660254037844387076, 1.000000000000000000, 0.9330127018922198534, 0.9330127018922191873 ) ) 
 REPRESENTATION_ITEM ( '' )  );
#9519 = CARTESIAN_POINT ( 'NONE',  ( -27.87471972953270338, 210.0000000000000284, 8.000000000000000000 ) ) ;
#9520 = CARTESIAN_POINT ( 'NONE',  ( -15.53471296425188442, 6.777313717898553413, -2.908627838312459080 ) ) ;
#9521 = CARTESIAN_POINT ( 'NONE',  ( -46.44122103062156981, 207.8379586601371329, -8.530955311639223382 ) ) ;
#9522 = CARTESIAN_POINT ( 'NONE',  ( 8.152565276336714462, 126.8476862821014635, -5.233372021372432847 ) ) ;
#9523 = CARTESIAN_POINT ( 'NONE',  ( 20.99999999999997868, 246.5687500012290343, 5.999999999999999112 ) ) ;
#9524 = CARTESIAN_POINT ( 'NONE',  ( -11.48171059495397373, 31.68518628210144428, -4.944772684328680334 ) ) ;
#9525 = CARTESIAN_POINT ( 'NONE',  ( 22.56230152254412147, 3.464101615137759271, -6.937500000000048850 ) ) ;
#9526 = ORIENTED_EDGE ( 'NONE', *, *, #26140, .T. ) ;
#9527 = CARTESIAN_POINT ( 'NONE',  ( 14.25334919248782661, 119.0851862821014606, 6.092822981423971385 ) ) ;
#9528 = DIRECTION ( 'NONE',  ( 0.000000000000000000, 0.000000000000000000, -1.000000000000000000 ) ) ;
#9529 = CARTESIAN_POINT ( 'NONE',  ( -3.474262827703527901, 142.7648137178985621, 8.843639120294245259 ) ) ;
#9530 = CARTESIAN_POINT ( 'NONE',  ( -27.24356964374999635, 197.5906250006145228, 15.72908226750539384 ) ) ;
#9531 = CARTESIAN_POINT ( 'NONE',  ( 14.99999999999954348, 3.464101615137491930, -1.387499999999978417 ) ) ;
#9532 = CARTESIAN_POINT ( 'NONE',  ( 18.71316448956201839, -5.789678881962990076, -10.00000000000000355 ) ) ;
#9533 = CARTESIAN_POINT ( 'NONE',  ( 37.64499961742345135, 3.604726614523243278, 168.6162884848450005 ) ) ;
#9534 = CARTESIAN_POINT ( 'NONE',  ( -44.35000000000001563, 244.5000000000000000, -2.499999999999997335 ) ) ;
#9535 = CARTESIAN_POINT ( 'NONE',  ( 2.064181346179061460, 68.30231371789852801, 9.465287035748106703 ) ) ;
#9536 = CARTESIAN_POINT ( 'NONE',  ( 16.07192114941521766, -3.422577806627481234, -8.000000000000001776 ) ) ;
#9537 = VERTEX_POINT ( 'NONE', #18259 ) ;
#9538 = VECTOR ( 'NONE', #10970, 1000.000000000000000 ) ;
#9539 = CARTESIAN_POINT ( 'NONE',  ( 23.99999999999999645, 243.6062500012290286, -5.196152422706631135 ) ) ;
#9540 = CARTESIAN_POINT ( 'NONE',  ( -2.660918448318005058, 72.90231371789855075, -12.46528703574811558 ) ) ;
#9541 = CARTESIAN_POINT ( 'NONE',  ( 10.31873187879411269, 3.604726614523240613, -4.284374999385515359 ) ) ;
#9542 = CARTESIAN_POINT ( 'NONE',  ( -12.65935014772596823, 143.0000000000000284, 5.795439718954652264 ) ) ;
#9543 = CARTESIAN_POINT ( 'NONE',  ( 15.24356964374999990, 3.323476615752268604, -4.340624999385463312 ) ) ;
#9544 = CARTESIAN_POINT ( 'NONE',  ( -7.228626920338836470, 53.92731371789854933, -10.49813415416005213 ) ) ;
#9545 = CARTESIAN_POINT ( 'NONE',  ( 27.24356964374999635, 196.9718750006145456, -15.72908226750539029 ) ) ;
#9546 = VERTEX_POINT ( 'NONE', #36751 ) ;
#9547 = VERTEX_POINT ( 'NONE', #35862 ) ;
#9548 = CARTESIAN_POINT ( 'NONE',  ( 20.99999999999999645, -6.646953231504538984, -5.878124999385467397 ) ) ;
#9549 = CARTESIAN_POINT ( 'NONE',  ( 26.75643035624999655, 245.0593750006144944, -3.323476615752271712 ) ) ;
#9550 = CARTESIAN_POINT ( 'NONE',  ( -12.53471296425194836, 49.22268628210144215, 2.311890736173176641 ) ) ;
#9551 = CARTESIAN_POINT ( 'NONE',  ( -32.57961230271183695, 211.8571965466040581, 6.469044688360755302 ) ) ;
#9552 = CARTESIAN_POINT ( 'NONE',  ( 22.80587116629410360, -3.604726614523235284, -1.753124999385512028 ) ) ;
#9553 = CARTESIAN_POINT ( 'NONE',  ( -62.66294563604517975, 214.6737587650350747, -4.842901733360249317 ) ) ;
#9554 = CARTESIAN_POINT ( 'NONE',  ( 8.562301522544109034, 9.797174393178823685E-16, -10.00000000000000000 ) ) ;
#9555 = CARTESIAN_POINT ( 'NONE',  ( -8.962234695871565293, 81.23981371789855643, -8.715434833792128799 ) ) ;
#9556 = CARTESIAN_POINT ( 'NONE',  ( -50.99330436395489841, 210.1155267958017703, -4.499999999999996447 ) ) ;
#9557 = CARTESIAN_POINT ( 'NONE',  ( -35.55580436395489130, 218.5000000000000000, 0.1155267958017064944 ) ) ;
#9558 = CARTESIAN_POINT ( 'NONE',  ( 26.75643035624999655, 7.049594010296217766E-16, -6.328124999385481786 ) ) ;
#9559 = CARTESIAN_POINT ( 'NONE',  ( 13.56230152254410903, 5.196152422706636465, -0.5250000000000532019 ) ) ;
#9560 = CARTESIAN_POINT ( 'NONE',  ( -6.092822981423666739, 54.21481371789855785, -14.25334919248795096 ) ) ;
#9561 = CARTESIAN_POINT ( 'NONE',  ( -61.87127896937851546, 218.5309553116392465, 2.162041339862725842 ) ) ;
#9562 = VECTOR ( 'NONE', #2747, 1000.000000000000000 ) ;
#9563 = CARTESIAN_POINT ( 'NONE',  ( 33.84263025878871645, -5.196152422706629359, 162.3707958259794566 ) ) ;
#9564 = CARTESIAN_POINT ( 'NONE',  ( 6.932735513423970097, 92.34768628210144925, 10.69584247140445044 ) ) ;
#9565 = CARTESIAN_POINT ( 'NONE',  ( 14.38691631536207538, 25.93518628210144072, -5.770363421893813793 ) ) ;
#9566 = CARTESIAN_POINT ( 'NONE',  ( 13.56230152254410903, 5.196152422706636465, -0.07500000000004725109 ) ) ;
#9567 = CARTESIAN_POINT ( 'NONE',  ( 36.86059793269458140, 3.604726614523243278, 159.6505362020193104 ) ) ;
#9568 = AXIS2_PLACEMENT_3D ( 'NONE', #33173, #16493, #25006 ) ;
#9569 = CARTESIAN_POINT ( 'NONE',  ( 3.257655550457285720, 52.09768628210144925, -15.46528703574804986 ) ) ;
#9570 = CARTESIAN_POINT ( 'NONE',  ( 27.24356964375000345, 196.4281250006145569, -3.336375036156643733E-15 ) ) ;
#9571 = CARTESIAN_POINT ( 'NONE',  ( 13.56230152254411259, -5.196152422706632912, -0.7124999987710434191 ) ) ;
#9572 = LINE ( 'NONE', #35331, #2524 ) ;
#9573 = CARTESIAN_POINT ( 'NONE',  ( -33.77455436395490551, 205.1570982666397356, 4.673758765035198159 ) ) ;
#9574 = ADVANCED_FACE ( 'NONE', ( #9726 ), #9904, .F. ) ;
#9575 = CARTESIAN_POINT ( 'NONE',  ( 37.30185536379384814, 3.464101615137935575, 167.4887799662076304 ) ) ;
#9576 = CARTESIAN_POINT ( 'NONE',  ( -12.53471296425194836, 21.62268628210144072, 2.311890736173176641 ) ) ;
#9577 = CARTESIAN_POINT ( 'NONE',  ( 20.99999999999997868, 210.0000000000000000, 5.999999999999999112 ) ) ;
#9578 = CARTESIAN_POINT ( 'NONE',  ( -6.840914352311947333, 136.4398137178985735, -6.594114490232462877 ) ) ;
#9579 = CARTESIAN_POINT ( 'NONE',  ( 23.87821517812500005, 245.9593750006145569, 4.985214923628404016 ) ) ;
#9580 = EDGE_LOOP ( 'NONE', ( #4310, #6892, #14299, #1890 ) ) ;
#9581 = CARTESIAN_POINT ( 'NONE',  ( 21.00000000000000000, -6.928203230275506996, -6.637499999999977085 ) ) ;
#9582 = DIRECTION ( 'NONE',  ( 0.000000000000000000, 0.000000000000000000, -1.000000000000000000 ) ) ;
#9583 = CARTESIAN_POINT ( 'NONE',  ( 20.99999999999999645, 6.928203230275506996, -6.806249998770949716 ) ) ;
#9584 = CARTESIAN_POINT ( 'NONE',  ( 19.68408634441910721, 5.407089921784857367, -5.690624999385579308 ) ) ;
#9585 = CARTESIAN_POINT ( 'NONE',  ( 34.25565102910361759, -5.407089921784855591, 165.6943207089371981 ) ) ;
#9586 = CARTESIAN_POINT ( 'NONE',  ( 29.51960950058489175, 6.028781714493277377, 159.5765249394674470 ) ) ;
#9587 = FACE_OUTER_BOUND ( 'NONE', #33645, .T. ) ;
#9588 = CARTESIAN_POINT ( 'NONE',  ( 2.311890736173175753, 46.92268628210144499, 12.53471296425194659 ) ) ;
#9589 = ORIENTED_EDGE ( 'NONE', *, *, #6674, .T. ) ;
#9590 = AXIS2_PLACEMENT_3D ( 'NONE', #15254, #27183, #6534 ) ;
#9591 = ORIENTED_EDGE ( 'NONE', *, *, #5304, .F. ) ;
#9592 = PLANE ( 'NONE',  #1284 ) ;
#9593 = CARTESIAN_POINT ( 'NONE',  ( 10.56230152254416765, -3.464101615137792134, -4.012500000000060574 ) ) ;
#9594 = DIRECTION ( 'NONE',  ( 1.000000000000000000, -0.000000000000000000, 1.052579609121344151E-14 ) ) ;
#9595 = CARTESIAN_POINT ( 'NONE',  ( 37.14170668649535401, 7.347880794884125653E-16, 165.6582722084640125 ) ) ;
#9596 = CARTESIAN_POINT ( 'NONE',  ( 23.87821517812500005, -4.985214923628404016, -8.990624999385465443 ) ) ;
#9597 = CARTESIAN_POINT ( 'NONE',  ( 2.311890736173175753, 92.92268628210145209, 12.53471296425194836 ) ) ;
#9598 = CARTESIAN_POINT ( 'NONE',  ( 3.257655550456945548, 22.30231371789854933, 15.46528703574811736 ) ) ;
#9599 = CARTESIAN_POINT ( 'NONE',  ( 26.99999999999999645, 243.5312500012290400, -7.347880794884117764E-16 ) ) ;
#9600 = EDGE_CURVE ( 'NONE', #15757, #18882, #14587, .T. ) ;
#9601 = CARTESIAN_POINT ( 'NONE',  ( -64.64211230271182274, 205.5309553116392465, 1.321298161741817356 ) ) ;
#9602 = LINE ( 'NONE', #3535, #25814 ) ;
#9603 = CARTESIAN_POINT ( 'NONE',  ( 25.25927379726832100, -3.464101615137757051, 167.5260017485858555 ) ) ;
#9604 = CARTESIAN_POINT ( 'NONE',  ( 12.46528703574811558, 139.6023137178985394, -2.660918448318005503 ) ) ;
#9605 = CARTESIAN_POINT ( 'NONE',  ( -60.29538769728823411, 211.8571965466039444, -6.469044688360768625 ) ) ;
#9606 = CARTESIAN_POINT ( 'NONE',  ( -68.60788769728823411, 218.4690446883607535, 2.393094931466250408 ) ) ;
#9607 = EDGE_CURVE ( 'NONE', #25759, #26216, #5607, .T. ) ;
#9608 = APPLICATION_PROTOCOL_DEFINITION ( 'draft international standard', 'automotive_design', 1998, #29401 ) ;
#9609 = DIRECTION ( 'NONE',  ( 1.000000000000000000, 0.000000000000000000, 0.000000000000000000 ) ) ;
#9610 = CARTESIAN_POINT ( 'NONE',  ( 13.62178482187499640, 199.2031250006145342, -23.59362340125807123 ) ) ;
#9611 = CARTESIAN_POINT ( 'NONE',  ( -8.927990412390371944, 109.1273137178985451, -13.04141134922778988 ) ) ;
#9612 = CARTESIAN_POINT ( 'NONE',  ( -59.69419563604516554, 203.5000000000000000, 0.1155267958017914542 ) ) ;
#9613 = ORIENTED_EDGE ( 'NONE', *, *, #33334, .T. ) ;
#9614 = CARTESIAN_POINT ( 'NONE',  ( 2.660918448318279950, 24.49768628210144783, -12.46528703574805697 ) ) ;
#9615 = CARTESIAN_POINT ( 'NONE',  ( 20.99999999999999645, 6.928203230275506996, -7.762500000000014388 ) ) ;
#9616 = CARTESIAN_POINT ( 'NONE',  ( 24.98477879236699195, 0.000000000000000000, 49.65137702900941008 ) ) ;
#9617 = CARTESIAN_POINT ( 'NONE',  ( 24.98639886122932197, 0.000000000000000000, 167.2016752052849426 ) ) ;
#9618 = CARTESIAN_POINT ( 'NONE',  ( 8.632099005475504683, 110.7476862821014691, 13.23911966647218996 ) ) ;
#9619 = CARTESIAN_POINT ( 'NONE',  ( 10.31873187879411091, 3.604726614523236616, -5.128124999385527794 ) ) ;
#9620 = CARTESIAN_POINT ( 'NONE',  ( 1.715153634034233487, 56.12268628210142651, 9.534712964251941258 ) ) ;
#9621 = CARTESIAN_POINT ( 'NONE',  ( 20.99999999999999289, 240.4937500012290457, -5.999999999999997335 ) ) ;
#9622 = CARTESIAN_POINT ( 'NONE',  ( -32.98288769728823411, 201.5309553116392181, -2.393094931466246855 ) ) ;
#9623 =( BOUNDED_CURVE ( )  B_SPLINE_CURVE ( 2, ( #21066, #30143, #3611, #757, #23900, #35442, #9490 ),
 .UNSPECIFIED., .F., .F. ) 
 B_SPLINE_CURVE_WITH_KNOTS ( ( 3, 2, 2, 3 ),
 ( 0.6739130434782618639, 0.6811594202898562100, 0.6884057971014503341, 0.6956521739130446802 ),
 .UNSPECIFIED. ) 
 CURVE ( )  GEOMETRIC_REPRESENTATION_ITEM ( )  RATIONAL_B_SPLINE_CURVE ( ( 0.9999999999999815703, 0.8660254037844571373, 1.000000000000000000, 0.8660254037844387076, 1.000000000000000000, 0.8660254037844161701, 1.000000000000022649 ) ) 
 REPRESENTATION_ITEM ( '' )  );
#9624 = CARTESIAN_POINT ( 'NONE',  ( 12.46528703574805874, 81.99768628210146915, 2.660918448318279950 ) ) ;
#9625 = FACE_OUTER_BOUND ( 'NONE', #20074, .T. ) ;
#9626 = FACE_OUTER_BOUND ( 'NONE', #24236, .T. ) ;
#9627 = CARTESIAN_POINT ( 'NONE',  ( 14.99999999999946709, 3.464101615137446188, -5.437500000000002665 ) ) ;
#9628 = CARTESIAN_POINT ( 'NONE',  ( 26.99999999999999645, 244.9187500012290286, -3.464101615137755275 ) ) ;
#9629 = CARTESIAN_POINT ( 'NONE',  ( 15.00000000000000178, -3.464101615137757051, -0.8624999999999944933 ) ) ;
#9631 = EDGE_CURVE ( 'NONE', #13240, #19996, #21157, .T. ) ;
#9630 = CARTESIAN_POINT ( 'NONE',  ( 37.18092677073180141, 7.347880794884125653E-16, 166.1065598226053055 ) ) ;
#9632 = CARTESIAN_POINT ( 'NONE',  ( 37.36392234706227811, -3.604726614523238837, 165.4035605834991145 ) ) ;
#9633 = CARTESIAN_POINT ( 'NONE',  ( 28.03214742813599969, 5.196152422706636465, 164.7989526413415149 ) ) ;
#9634 = CARTESIAN_POINT ( 'NONE',  ( 24.00000000000000000, 247.0000000000000000, 5.196152422706629359 ) ) ;
#9635 = CARTESIAN_POINT ( 'NONE',  ( -1.926257025242585782E-15, 196.0906250006145228, -31.45816453501076637 ) ) ;
#9636 = CARTESIAN_POINT ( 'NONE',  ( 6.932735513424201024, 101.6523137178985650, -10.69584247140429412 ) ) ;
#9637 = CARTESIAN_POINT ( 'NONE',  ( -4.944772684328673229, 112.1851862821014549, 11.48171059495397728 ) ) ;
#9638 = ORIENTED_EDGE ( 'NONE', *, *, #19300, .F. ) ;
#9639 = ORIENTED_EDGE ( 'NONE', *, *, #17982, .T. ) ;
#9640 = CARTESIAN_POINT ( 'NONE',  ( -27.24356964374999635, 195.7906250006145115, 15.72908226750539384 ) ) ;
#9641 = LINE ( 'NONE', #9826, #6566 ) ;
#9642 = EDGE_CURVE ( 'NONE', #36568, #2166, #21911, .T. ) ;
#9643 = CARTESIAN_POINT ( 'NONE',  ( -8.927990412390371944, 81.52731371789856496, -13.04141134922778988 ) ) ;
#9644 = CARTESIAN_POINT ( 'NONE',  ( 26.75643035624999655, -3.323476615752267715, -7.715624999385478411 ) ) ;
#9645 = CARTESIAN_POINT ( 'NONE',  ( 15.24356964374999990, 245.7718750006145001, -3.323476615752268604 ) ) ;
#9646 = CARTESIAN_POINT ( 'NONE',  ( 3.796722387233379514, 107.5851862821014748, -8.710071997420127943 ) ) ;
#9647 = EDGE_CURVE ( 'NONE', #6483, #31946, #5535, .T. ) ;
#9648 = CARTESIAN_POINT ( 'NONE',  ( 26.99999999999999645, 243.0812500012290513, -7.347880794884117764E-16 ) ) ;
#9649 = CARTESIAN_POINT ( 'NONE',  ( -0.1745138560723084320, 54.78981371789855359, -9.500000000000005329 ) ) ;
#9650 = CARTESIAN_POINT ( 'NONE',  ( 13.44051670066911086, 5.407089921784856479, -5.165624999385554084 ) ) ;
#9651 = CARTESIAN_POINT ( 'NONE',  ( 8.152565276336593669, 103.9523137178985763, 5.233372021372610483 ) ) ;
#9652 = CARTESIAN_POINT ( 'NONE',  ( 20.99999999999999645, 239.9593750006145001, 6.646953231504538984 ) ) ;
#9653 = CARTESIAN_POINT ( 'NONE',  ( 12.46528703574811558, 38.40231371789855075, -2.660918448318005503 ) ) ;
#9654 = CARTESIAN_POINT ( 'NONE',  ( 31.45868912971818432, 0.000000000000000000, 169.5433637710095809 ) ) ;
#9655 = CARTESIAN_POINT ( 'NONE',  ( 8.715434833791931624, 82.86018628210145209, 8.962234695871760692 ) ) ;
#9656 = CARTESIAN_POINT ( 'NONE',  ( 19.56230152254411081, 5.196152422706631135, -4.987499998771016685 ) ) ;
#9657 = EDGE_CURVE ( 'NONE', #17309, #23915, #107, .T. ) ;
#9658 = CARTESIAN_POINT ( 'NONE',  ( 18.00000000000000000, 5.196152422706630247, -1.818749998770963217 ) ) ;
#9659 = CARTESIAN_POINT ( 'NONE',  ( 37.29038468911893034, -3.604726614523235284, 164.5630213069841830 ) ) ;
#9660 = CARTESIAN_POINT ( 'NONE',  ( -10.83675517735155047, 78.26018628210144357, -11.08355503943142750 ) ) ;
#9661 = CARTESIAN_POINT ( 'NONE',  ( 10.31873187879411091, -3.604726614523244610, -5.109374999385544847 ) ) ;
#9662 =( NAMED_UNIT ( * ) PLANE_ANGLE_UNIT ( ) SI_UNIT ( $, .RADIAN. ) );
#9663 = DIRECTION ( 'NONE',  ( 0.000000000000000000, -0.000000000000000000, 1.000000000000000000 ) ) ;
#9664 = CARTESIAN_POINT ( 'NONE',  ( 25.36712902881149745, -3.464101615137806345, 168.7587926862500183 ) ) ;
#9665 = CARTESIAN_POINT ( 'NONE',  ( 6.594114490232313663, 119.6601862821014635, 6.840914352312096547 ) ) ;
#9666 = CARTESIAN_POINT ( 'NONE',  ( 1.069080835302379631E-14, 198.8750000012290400, 27.00000000000000000 ) ) ;
#9667 = CARTESIAN_POINT ( 'NONE',  ( 12.46528703574805874, 127.9976862821014407, 2.660918448318279950 ) ) ;
#9668 = CARTESIAN_POINT ( 'NONE',  ( 27.24356964375000345, 196.0343750006145456, -3.336375036156643733E-15 ) ) ;
#9669 = CARTESIAN_POINT ( 'NONE',  ( 18.12178482187499640, 240.2218750006145171, -4.985214923628404904 ) ) ;
#9670 = ORIENTED_EDGE ( 'NONE', *, *, #25721, .F. ) ;
#9671 = CARTESIAN_POINT ( 'NONE',  ( 25.06647319987872535, 3.604726614523236616, 168.1169290841567090 ) ) ;
#9672 = CARTESIAN_POINT ( 'NONE',  ( 15.24356964375000167, -3.323476615752272600, -2.803124999385491645 ) ) ;
#9673 = EDGE_CURVE ( 'NONE', #13899, #12159, #477, .T. ) ;
#9674 = CARTESIAN_POINT ( 'NONE',  ( 10.56230152254363652, -3.464101615137481716, -5.249999998771001763 ) ) ;
#9675 = CARTESIAN_POINT ( 'NONE',  ( 10.56230152254410903, 0.000000000000000000, 10.00000000000000000 ) ) ;
#9676 = CYLINDRICAL_SURFACE ( 'NONE', #31811, 5.999999999999998224 ) ;
#9677 = CARTESIAN_POINT ( 'NONE',  ( 28.13346597918727099, -5.196152422706632912, 165.9570289790974869 ) ) ;
#9678 = DIRECTION ( 'NONE',  ( 0.000000000000000000, 0.000000000000000000, 1.000000000000000000 ) ) ;
#9679 = CARTESIAN_POINT ( 'NONE',  ( 5.529263428287300108, 21.72731371789853938, 7.954856959092309943 ) ) ;
#9680 = CARTESIAN_POINT ( 'NONE',  ( -27.24356964375000345, 196.2593750006145399, 0.000000000000000000 ) ) ;
#9682 = ORIENTED_EDGE ( 'NONE', *, *, #36803, .T. ) ;
#9681 = VERTEX_POINT ( 'NONE', #12044 ) ;
#9683 = CARTESIAN_POINT ( 'NONE',  ( 26.75643035624999655, 248.1343750006145115, 3.323476615752267715 ) ) ;
#9684 = CARTESIAN_POINT ( 'NONE',  ( 12.50000000000000355, 20.28981371789855004, -0.1745138560722771515 ) ) ;
#9685 = CARTESIAN_POINT ( 'NONE',  ( 15.24356964374999990, 3.323476615752268604, -2.428124999385457894 ) ) ;
#9686 = CARTESIAN_POINT ( 'NONE',  ( -15.50000000000000533, 135.2898137178985394, 0.1745138560722471477 ) ) ;
#9687 = CARTESIAN_POINT ( 'NONE',  ( 24.00000000000000000, -5.196152422706629359, -8.343749998770967125 ) ) ;
#9688 = CARTESIAN_POINT ( 'NONE',  ( -13.50000000000000533, 199.5875000012290457, -23.38268590217984411 ) ) ;
#9689 = ORIENTED_EDGE ( 'NONE', *, *, #22347, .T. ) ;
#9690 = CARTESIAN_POINT ( 'NONE',  ( 10.31873187879411091, 3.604726614523240613, -6.534374999385494043 ) ) ;
#9691 = EDGE_CURVE ( 'NONE', #717, #9547, #12232, .T. ) ;
#9692 = EDGE_LOOP ( 'NONE', ( #35454, #20087 ) ) ;
#9693 = CARTESIAN_POINT ( 'NONE',  ( -13.62178482187500528, 195.6781250006145569, -23.59362340125807123 ) ) ;
#9694 = CARTESIAN_POINT ( 'NONE',  ( -7.228626920339069173, 130.8726862821014834, 10.49813415415989581 ) ) ;
#9695 = CARTESIAN_POINT ( 'NONE',  ( 24.83278686463658502, -3.604726614523244610, 165.4458820498982163 ) ) ;
#9696 = CARTESIAN_POINT ( 'NONE',  ( -58.11086230271183695, 214.1499508600178387, -7.418979330068641964 ) ) ;
#9697 = CARTESIAN_POINT ( 'NONE',  ( 20.99999999999999645, 246.7093750006145285, 6.646953231504538984 ) ) ;
#9698 =( LENGTH_UNIT ( ) NAMED_UNIT ( * ) SI_UNIT ( .MILLI., .METRE. ) );
#9699 = DIRECTION ( 'NONE',  ( 0.08715574274765150453, 0.000000000000000000, 0.9961946980917461003 ) ) ;
#9700 = CARTESIAN_POINT ( 'NONE',  ( -40.89211230271183695, 205.5309553116392465, 1.321298161741817356 ) ) ;
#9701 = CARTESIAN_POINT ( 'NONE',  ( -33.57663769728823411, 204.3130714775002730, 3.149950860017883603 ) ) ;
#9702 = CARTESIAN_POINT ( 'NONE',  ( 31.18169728485186454, -7.209453229046475009, 166.3773324967488918 ) ) ;
#9703 = ORIENTED_EDGE ( 'NONE', *, *, #21799, .F. ) ;
#9704 = CARTESIAN_POINT ( 'NONE',  ( -28.62304584722514988, 203.4962709778747580, 4.665718542665365121 ) ) ;
#9705 = VECTOR ( 'NONE', #31157, 1000.000000000000000 ) ;
#9706 = CARTESIAN_POINT ( 'NONE',  ( -3.257655550457281723, 130.2976862821014379, 15.46528703574804986 ) ) ;
#9707 = CARTESIAN_POINT ( 'NONE',  ( -49.60788769728823411, 218.4690446883607535, 2.393094931466250408 ) ) ;
#9708 = CARTESIAN_POINT ( 'NONE',  ( -2.064181346179269738, 121.0976862821014635, 9.465287035748067623 ) ) ;
#9709 = EDGE_CURVE ( 'NONE', #32329, #25286, #27872, .T. ) ;
#9710 = CARTESIAN_POINT ( 'NONE',  ( 26.99999999999999289, 0.000000000000000000, -8.000000000000000000 ) ) ;
#9711 = ADVANCED_FACE ( 'NONE', ( #23426 ), #20592, .F. ) ;
#9712 = CARTESIAN_POINT ( 'NONE',  ( -8.962234695871760692, 39.16018628210144215, 8.715434833791933400 ) ) ;
#9713 = CARTESIAN_POINT ( 'NONE',  ( 19.56230152254412147, 5.196152422706637353, -7.350000000000022737 ) ) ;
#9714 = UNCERTAINTY_MEASURE_WITH_UNIT (LENGTH_MEASURE( 1.000000000000000082E-05 ), #28, 'distance_accuracy_value', 'NONE');
#9715 = ORIENTED_EDGE ( 'NONE', *, *, #34029, .F. ) ;
#9716 = CARTESIAN_POINT ( 'NONE',  ( -0.1745138560725817967, 130.0101862821014436, 15.50000000000000533 ) ) ;
#9717 = DIRECTION ( 'NONE',  ( 0.000000000000000000, 0.000000000000000000, 1.000000000000000000 ) ) ;
#9718 = CARTESIAN_POINT ( 'NONE',  ( 3.474262827703532341, 138.1648137178985678, -8.843639120294245259 ) ) ;
#9719 = AXIS2_PLACEMENT_3D ( 'NONE', #25908, #37454, #35926 ) ;
#9720 = CARTESIAN_POINT ( 'NONE',  ( -13.62178482187498396, 198.5281250006145228, 23.59362340125808188 ) ) ;
#9722 = CARTESIAN_POINT ( 'NONE',  ( 13.49999999999999645, 198.1625000012290343, -23.38268590217984766 ) ) ;
#9721 =( BOUNDED_CURVE ( )  B_SPLINE_CURVE ( 2, ( #31950, #28918, #14708, #5982, #2952, #14522, #29097 ),
 .UNSPECIFIED., .F., .F. ) 
 B_SPLINE_CURVE_WITH_KNOTS ( ( 3, 2, 2, 3 ),
 ( 0.5652173913043470055, 0.5724637681159411295, 0.5797101449275352536, 0.5869565217391293777 ),
 .UNSPECIFIED. ) 
 CURVE ( )  GEOMETRIC_REPRESENTATION_ITEM ( )  RATIONAL_B_SPLINE_CURVE ( ( 1.000000000000014433, 0.8660254037844243857, 1.000000000000000000, 0.8660254037844387076, 1.000000000000000000, 0.8660254037844592467, 0.9999999999999794609 ) ) 
 REPRESENTATION_ITEM ( '' )  );
#9723 = CARTESIAN_POINT ( 'NONE',  ( 13.50000000000001421, 195.6500000000000057, 23.38268590217984055 ) ) ;
#9724 = CARTESIAN_POINT ( 'NONE',  ( 19.39205759080449809, -5.473655403650819373, -10.00000000000000000 ) ) ;
#9725 = EDGE_CURVE ( 'NONE', #12708, #4247, #31512, .T. ) ;
#9726 = FACE_OUTER_BOUND ( 'NONE', #2820, .T. ) ;
#9727 = CARTESIAN_POINT ( 'NONE',  ( 36.71028575989448228, 7.347880794884125653E-16, 160.7271084529098744 ) ) ;
#9728 = CARTESIAN_POINT ( 'NONE',  ( 9.465287035748106703, 84.40231371789855075, -2.064181346179063237 ) ) ;
#9729 = DIRECTION ( 'NONE',  ( 0.9925324990730152175, -0.1219804832088933616, 0.000000000000000000 ) ) ;
#9730 = ORIENTED_EDGE ( 'NONE', *, *, #19911, .F. ) ;
#9731 = CARTESIAN_POINT ( 'NONE',  ( 23.99999999999999645, 243.1562500012290400, -5.196152422706631135 ) ) ;
#9732 = CARTESIAN_POINT ( 'NONE',  ( 8.962234695871567070, 76.63981371789856212, 8.715434833792127023 ) ) ;
#9733 = CARTESIAN_POINT ( 'NONE',  ( 16.56230152254411436, -7.209453229046482114, -3.234374999385536853 ) ) ;
#9734 = CARTESIAN_POINT ( 'NONE',  ( -81.72704584564829133, 216.6260876520869658, -5.000000000000000888 ) ) ;
#9735 = CARTESIAN_POINT ( 'NONE',  ( 15.24356964374999990, 3.323476615752268604, -3.890624999385467575 ) ) ;
#9736 = CARTESIAN_POINT ( 'NONE',  ( 10.69584247140429589, 39.55231371789855643, 6.932735513424201024 ) ) ;
#9737 = COLOUR_RGB ( '',0.8941176470588234615, 0.8941176470588234615, 0.8941176470588234615 ) ;
#9738 = ORIENTED_EDGE ( 'NONE', *, *, #17124, .F. ) ;
#9739 = CARTESIAN_POINT ( 'NONE',  ( 23.87821517812500005, -4.985214923628404016, -7.640624999385475569 ) ) ;
#9740 = CARTESIAN_POINT ( 'NONE',  ( 15.24356964374999990, 244.3093750006145228, -3.323476615752268604 ) ) ;
#9741 = CARTESIAN_POINT ( 'NONE',  ( -10.69584247140444866, 30.24768628210144783, 6.932735513423972762 ) ) ;
#9742 = CARTESIAN_POINT ( 'NONE',  ( -35.15252896937850124, 206.6499508600178387, -5.571401726697954970 ) ) ;
#9743 = CARTESIAN_POINT ( 'NONE',  ( -60.09002896937850124, 204.4285982733020433, 3.350049139982171020 ) ) ;
#9744 = CARTESIAN_POINT ( 'NONE',  ( 30.65467740297821919, -6.928203230275506996, 160.3534676823375378 ) ) ;
#9745 = CARTESIAN_POINT ( 'NONE',  ( 0.1745138560722779009, 86.98981371789855643, 12.50000000000000355 ) ) ;
#9746 = CARTESIAN_POINT ( 'NONE',  ( -43.47247103062156981, 207.6499508600178387, 3.839350919129076445 ) ) ;
#9747 = CARTESIAN_POINT ( 'NONE',  ( -36.94122103062156981, 207.8379586601371329, -8.530955311639223382 ) ) ;
#9748 = CARTESIAN_POINT ( 'NONE',  ( 18.12178482187499640, 4.985214923628404904, -7.078124999385481786 ) ) ;
#9749 = CARTESIAN_POINT ( 'NONE',  ( 16.56230152254410726, 0.000000000000000000, -10.00000000000000000 ) ) ;
#9750 = CARTESIAN_POINT ( 'NONE',  ( 10.83675517735179206, 55.93981371789855217, -11.08355503943118769 ) ) ;
#9751 = CARTESIAN_POINT ( 'NONE',  ( -39.70461230271183695, 207.6069050685336492, -8.469044688360751749 ) ) ;
#9752 = CARTESIAN_POINT ( 'NONE',  ( -0.1745138560725500443, 84.01018628210145778, 12.50000000000000355 ) ) ;
#9753 = CARTESIAN_POINT ( 'NONE',  ( 15.50000000000000533, 35.71018628210144641, 0.1745138560725827404 ) ) ;
#9754 = CARTESIAN_POINT ( 'NONE',  ( 16.56230152254411436, -6.928203230275514990, -0.7875000000000326184 ) ) ;
#9755 = CARTESIAN_POINT ( 'NONE',  ( 10.56230152254411081, 0.000000000000000000, -5.287499998771011178 ) ) ;
#9756 = CIRCLE ( 'NONE', #4287, 3.500000000000002220 ) ;
#9757 = ORIENTED_EDGE ( 'NONE', *, *, #9243, .F. ) ;
#9758 = CARTESIAN_POINT ( 'NONE',  ( 8.927990412390657937, 43.47268628210144215, -13.04141134922759804 ) ) ;
#9759 = CARTESIAN_POINT ( 'NONE',  ( -13.62178482187500528, 197.4781250006145399, -23.59362340125807123 ) ) ;
#9760 = CARTESIAN_POINT ( 'NONE',  ( 18.00000000000000355, -5.196152422706632912, -1.218749998770946030 ) ) ;
#9761 = CARTESIAN_POINT ( 'NONE',  ( -35.35788769728823411, 216.4690446883607535, 1.857196546604031662 ) ) ;
#9762 = CARTESIAN_POINT ( 'NONE',  ( 25.01079625726091749, 203.5081962293401148, 5.000000000000000000 ) ) ;
#9763 = CARTESIAN_POINT ( 'NONE',  ( -4.944772684328673229, 20.18518628210144783, 11.48171059495397728 ) ) ;
#9764 = CARTESIAN_POINT ( 'NONE',  ( 8.152565276336593669, 122.3523137178985394, 5.233372021372610483 ) ) ;
#9765 = CARTESIAN_POINT ( 'NONE',  ( 23.87821517812499650, 244.7593750006145399, -4.985214923628404904 ) ) ;
#9766 = ORIENTED_EDGE ( 'NONE', *, *, #18960, .F. ) ;
#9767 = CARTESIAN_POINT ( 'NONE',  ( 18.00000000000000355, -5.196152422706632912, -7.574999999999998401 ) ) ;
#9768 = CARTESIAN_POINT ( 'NONE',  ( -12.46528703574811558, 135.0023137178985451, 2.660918448318004170 ) ) ;
#9769 = CARTESIAN_POINT ( 'NONE',  ( 13.44051670066911797, -5.407089921784859143, -6.365624999385560479 ) ) ;
#9770 = CARTESIAN_POINT ( 'NONE',  ( 27.97700992647863316, 5.407089921784856479, 165.5660522374229799 ) ) ;
#9771 = CARTESIAN_POINT ( 'NONE',  ( -6.213262668644736308, 222.0587753200859424, 2.499999999999998668 ) ) ;
#9772 = EDGE_CURVE ( 'NONE', #30148, #5563, #9721, .T. ) ;
#9773 = CARTESIAN_POINT ( 'NONE',  ( 2.311890736173175753, 56.12268628210144783, 12.53471296425194659 ) ) ;
#9774 = VERTEX_POINT ( 'NONE', #3140 ) ;
#9775 = ORIENTED_EDGE ( 'NONE', *, *, #9460, .T. ) ;
#9776 = CARTESIAN_POINT ( 'NONE',  ( 13.49999999999999645, 196.8125000012290400, -23.38268590217984766 ) ) ;
#9777 = CARTESIAN_POINT ( 'NONE',  ( -55.52725981217221118, 242.6196170348268879, 0.4999999999999997780 ) ) ;
#9778 = CYLINDRICAL_SURFACE ( 'NONE', #21556, 5.999999999999998224 ) ;
#9779 =( BOUNDED_CURVE ( )  B_SPLINE_CURVE ( 2, ( #29943, #23890, #27102, #1126, #35807, #10032, #36178, #21612, #9850 ),
 .UNSPECIFIED., .F., .F. ) 
 B_SPLINE_CURVE_WITH_KNOTS ( ( 3, 2, 2, 2, 3 ),
 ( 0.1195652173913043653, 0.1231884057971014551, 0.1304347826086956486, 0.1376811594202898559, 0.1413043478260869457 ),
 .UNSPECIFIED. ) 
 CURVE ( )  GEOMETRIC_REPRESENTATION_ITEM ( )  RATIONAL_B_SPLINE_CURVE ( ( 0.9330127018922194093, 0.9330127018922196314, 1.000000000000000000, 0.8660254037844387076, 1.000000000000000000, 0.8660254037844387076, 1.000000000000000000, 0.9330127018922196314, 0.9330127018922194093 ) ) 
 REPRESENTATION_ITEM ( '' )  );
#9780 = DIRECTION ( 'NONE',  ( 2.057406622567553763E-16, -0.000000000000000000, -1.000000000000000000 ) ) ;
#9781 = CARTESIAN_POINT ( 'NONE',  ( 15.24356964375000167, -3.323476615752272600, -8.203124999385472904 ) ) ;
#9782 = CARTESIAN_POINT ( 'NONE',  ( -12.46528703574805697, 77.39768628210144641, -2.660918448318280838 ) ) ;
#9783 = CARTESIAN_POINT ( 'NONE',  ( -2.908627838312453306, 22.87731371789854151, 15.53471296425188797 ) ) ;
#9784 = DIRECTION ( 'NONE',  ( 1.000000000000000000, 0.000000000000000000, 0.000000000000000000 ) ) ;
#9785 = CARTESIAN_POINT ( 'NONE',  ( 14.62176384544827101, 216.3782361545538606, 2.408991313804690115 ) ) ;
#9786 = CARTESIAN_POINT ( 'NONE',  ( -62.06919563604516554, 214.5000000000000284, -0.1155267958017627827 ) ) ;
#9787 = LINE ( 'NONE', #32903, #4063 ) ;
#9788 = CARTESIAN_POINT ( 'NONE',  ( 25.29195720079868792, 3.464101615137752166, 167.8995747603702853 ) ) ;
#9789 = CARTESIAN_POINT ( 'NONE',  ( 6.932735513424201024, 138.4523137178985621, -10.69584247140429412 ) ) ;
#9790 = CARTESIAN_POINT ( 'NONE',  ( -47.43080436395489841, 203.5000000000000000, -0.1155267958017335561 ) ) ;
#9791 = CARTESIAN_POINT ( 'NONE',  ( -65.44122103062156270, 207.8379586601371329, -8.530955311639223382 ) ) ;
#9792 = APPLICATION_PROTOCOL_DEFINITION ( 'draft international standard', 'automotive_design', 1998, #12693 ) ;
#9793 = CARTESIAN_POINT ( 'NONE',  ( 5.778771075727756162E-15, 198.1156250006145285, 31.45816453501075927 ) ) ;
#9794 = CARTESIAN_POINT ( 'NONE',  ( -14.38691631536193860, 117.4648137178985650, -5.770363421894132649 ) ) ;
#9795 = CARTESIAN_POINT ( 'NONE',  ( -39.70461230271183695, 208.1428034533959135, -6.469044688360754414 ) ) ;
#9796 = ORIENTED_EDGE ( 'NONE', *, *, #14549, .T. ) ;
#9797 = CARTESIAN_POINT ( 'NONE',  ( 10.49813415415989581, 36.57268628210145067, 7.228626920339068285 ) ) ;
#9798 = CARTESIAN_POINT ( 'NONE',  ( 14.99999999999962874, 3.464101615137538115, -7.687499999999983125 ) ) ;
#9799 = DIRECTION ( 'NONE',  ( -1.000000000000000000, 0.000000000000000000, -0.000000000000000000 ) ) ;
#9800 = CARTESIAN_POINT ( 'NONE',  ( 37.36392234706227811, -3.604726614523238837, 165.4035605834991145 ) ) ;
#9801 = CARTESIAN_POINT ( 'NONE',  ( -11.08355503943142573, 103.5601862821014407, 10.83675517735155402 ) ) ;
#9802 = CIRCLE ( 'NONE', #18915, 2.649999999999994582 ) ;
#9803 = CARTESIAN_POINT ( 'NONE',  ( -50.59747103062156270, 213.3500491399821328, -5.571401726697985168 ) ) ;
#9804 = CARTESIAN_POINT ( 'NONE',  ( 22.80587116629410716, 3.604726614523238837, -5.278124999385515714 ) ) ;
#9805 = CARTESIAN_POINT ( 'NONE',  ( 3.796722387233379514, 33.98518628210143788, -8.710071997420127943 ) ) ;
#9806 = FACE_OUTER_BOUND ( 'NONE', #24174, .T. ) ;
#9807 = CARTESIAN_POINT ( 'NONE',  ( -37.93080436395490551, 201.5000000000000000, -0.1155267958017054536 ) ) ;
#9808 = DIRECTION ( 'NONE',  ( -0.000000000000000000, -1.000000000000000000, -0.000000000000000000 ) ) ;
#9809 = CARTESIAN_POINT ( 'NONE',  ( 2.311890736173175753, 83.72268628210143504, 12.53471296425194836 ) ) ;
#9810 = CARTESIAN_POINT ( 'NONE',  ( 22.56230152254534715, -3.464101615137050505, -8.362500000000045119 ) ) ;
#9811 = CARTESIAN_POINT ( 'NONE',  ( 27.00000000000000355, 199.3249999999999886, -3.306546357697854128E-15 ) ) ;
#9813 = CARTESIAN_POINT ( 'NONE',  ( 26.99999999999962341, 3.464101615137969770, -5.587499999999994138 ) ) ;
#9812 = CARTESIAN_POINT ( 'NONE',  ( 0.1745138560725194299, 42.61018628210144499, -9.500000000000005329 ) ) ;
#9814 = CARTESIAN_POINT ( 'NONE',  ( -49.64999999999999858, 244.5000000000000000, 2.500000000000001332 ) ) ;
#9815 = CARTESIAN_POINT ( 'NONE',  ( 15.24356964374999990, 3.323476615752268604, -10.07812499938544804 ) ) ;
#9816 = DIRECTION ( 'NONE',  ( -0.000000000000000000, 1.000000000000000000, -0.000000000000000000 ) ) ;
#9817 = CARTESIAN_POINT ( 'NONE',  ( 27.67142010346968561, -5.407089921784865361, 162.0731445772388213 ) ) ;
#9818 = CARTESIAN_POINT ( 'NONE',  ( 24.85073125303158292, 3.464101615137757051, 162.8563391000564593 ) ) ;
#9819 = CARTESIAN_POINT ( 'NONE',  ( 15.00000000000000178, 245.5375000000000227, 3.464101615137757051 ) ) ;
#9820 = CARTESIAN_POINT ( 'NONE',  ( -13.62178482187498396, 196.2781250006145228, 23.59362340125808188 ) ) ;
#9821 = CARTESIAN_POINT ( 'NONE',  ( 4.944772684328420986, 95.61481371789857064, 11.48171059495408208 ) ) ;
#9822 = CARTESIAN_POINT ( 'NONE',  ( -10.49813415415989404, 105.5726862821014578, -7.228626920339069173 ) ) ;
#9823 = ORIENTED_EDGE ( 'NONE', *, *, #35496, .T. ) ;
#9824 = VERTEX_POINT ( 'NONE', #6362 ) ;
#9825 = CARTESIAN_POINT ( 'NONE',  ( -27.24356964374999635, 196.2406250006145285, 15.72908226750539384 ) ) ;
#9826 = CARTESIAN_POINT ( 'NONE',  ( 15.02283181144952628, 7.347880794884122694E-16, 50.52293445648592751 ) ) ;
#9827 = CARTESIAN_POINT ( 'NONE',  ( -5.770363421894122880, 69.16481371789853938, 14.38691631536194393 ) ) ;
#9828 =( BOUNDED_CURVE ( )  B_SPLINE_CURVE ( 2, ( #24260, #15161, #26710, #741, #552, #35051, #35803, #32589, #12312 ),
 .UNSPECIFIED., .F., .F. ) 
 B_SPLINE_CURVE_WITH_KNOTS ( ( 3, 2, 2, 2, 3 ),
 ( 0.1413043478260869457, 0.1449275362318840632, 0.1521739130434782705, 0.1594202898550724501, 0.1630434782608695676 ),
 .UNSPECIFIED. ) 
 CURVE ( )  GEOMETRIC_REPRESENTATION_ITEM ( )  RATIONAL_B_SPLINE_CURVE ( ( 0.9330127018922194093, 0.9330127018922190762, 1.000000000000000000, 0.8660254037844387076, 1.000000000000000000, 0.8660254037844387076, 1.000000000000000000, 0.9330127018922190762, 0.9330127018922194093 ) ) 
 REPRESENTATION_ITEM ( '' )  );
#9829 = CARTESIAN_POINT ( 'NONE',  ( 21.00000000000000000, 6.646953231504538984, -5.765624999385476457 ) ) ;
#9830 = CARTESIAN_POINT ( 'NONE',  ( 15.24356964374999990, 245.3218750006145399, -3.323476615752268604 ) ) ;
#9831 = CARTESIAN_POINT ( 'NONE',  ( 2.064181346179272847, 107.2976862821014521, -9.465287035748065847 ) ) ;
#9832 = CARTESIAN_POINT ( 'NONE',  ( 24.00000000000000000, 243.0062500012290627, 5.196152422706629359 ) ) ;
#9833 = CARTESIAN_POINT ( 'NONE',  ( 6.840914352311949109, 58.23981371789854222, 6.594114490232462877 ) ) ;
#9834 = CARTESIAN_POINT ( 'NONE',  ( 16.56230152254410726, -7.209453229046475009, -8.578124999385506655 ) ) ;
#9835 = ADVANCED_FACE ( 'NONE', ( #32133 ), #17933, .T. ) ;
#9836 = CARTESIAN_POINT ( 'NONE',  ( -9.500000000000005329, 116.8898137178985621, 0.1745138560723101806 ) ) ;
#9837 = CARTESIAN_POINT ( 'NONE',  ( 26.75643035624999655, 240.0343750006145740, 3.323476615752267271 ) ) ;
#9838 = CARTESIAN_POINT ( 'NONE',  ( 10.49813415416005213, 28.62731371789854506, -7.228626920338837358 ) ) ;
#9839 = DIRECTION ( 'NONE',  ( 0.000000000000000000, 0.000000000000000000, 1.000000000000000000 ) ) ;
#9840 = CARTESIAN_POINT ( 'NONE',  ( 6.932735513423970097, 83.14768628210144641, 10.69584247140445044 ) ) ;
#9841 = CARTESIAN_POINT ( 'NONE',  ( 13.56230152254411436, -5.196152422706632912, -5.662499998771053811 ) ) ;
#9842 = SHAPE_REPRESENTATION ( 'head', ( #17215 ), #29865 ) ;
#9843 = CARTESIAN_POINT ( 'NONE',  ( 15.00000000000000000, 0.000000000000000000, -0.07031249969274844247 ) ) ;
#9844 = CARTESIAN_POINT ( 'NONE',  ( 27.83320295094501162, -5.407089921784859143, 163.9223309855715911 ) ) ;
#9845 = CARTESIAN_POINT ( 'NONE',  ( 22.80587116629411781, 3.604726614523243278, -4.434374999385503280 ) ) ;
#9846 = CARTESIAN_POINT ( 'NONE',  ( 10.56230152254450338, 3.464101615137982204, -3.074999998770982845 ) ) ;
#9847 = LINE ( 'NONE', #21424, #28518 ) ;
#9848 = CARTESIAN_POINT ( 'NONE',  ( 26.99999999999936051, -3.464101615138118984, -5.606249998770957532 ) ) ;
#9849 = CARTESIAN_POINT ( 'NONE',  ( 9.500000000000005329, 118.5101862821014720, 0.1745138560725188748 ) ) ;
#9850 = CARTESIAN_POINT ( 'NONE',  ( 20.99999999999998579, 248.1437500012290229, -5.999999999999997335 ) ) ;
#9851 = CARTESIAN_POINT ( 'NONE',  ( -4.622313124798576922, 124.8351862821014748, -11.61527771782819762 ) ) ;
#9852 = CARTESIAN_POINT ( 'NONE',  ( -29.00000000000002487, 210.0000000000000000, -8.000000000000000000 ) ) ;
#9853 = CARTESIAN_POINT ( 'NONE',  ( 18.12178482187499640, 248.8843750006145399, -4.985214923628404904 ) ) ;
#9854 = ORIENTED_EDGE ( 'NONE', *, *, #36329, .T. ) ;
#9855 = CARTESIAN_POINT ( 'NONE',  ( 37.45380170677077558, 3.604726614523238837, 166.4308863659062183 ) ) ;
#9856 = CARTESIAN_POINT ( 'NONE',  ( 26.75643035624999655, 7.049594010296217766E-16, -2.615624999385474325 ) ) ;
#9857 = EDGE_CURVE ( 'NONE', #32744, #26637, #21377, .T. ) ;
#9858 = CARTESIAN_POINT ( 'NONE',  ( 24.53624671473563623, -4.728541327911522707, -8.000000000000000000 ) ) ;
#9859 = DIRECTION ( 'NONE',  ( -0.000000000000000000, 0.000000000000000000, 1.000000000000000000 ) ) ;
#9860 = AXIS2_PLACEMENT_3D ( 'NONE', #12838, #30658, #1083 ) ;
#9861 = CARTESIAN_POINT ( 'NONE',  ( 16.56230152254411436, -7.209453229046475009, -0.4781249993855187230 ) ) ;
#9862 = CARTESIAN_POINT ( 'NONE',  ( -3.474262827703527901, 23.16481371789855359, 8.843639120294245259 ) ) ;
#9863 = CARTESIAN_POINT ( 'NONE',  ( -13.62178482187500528, 196.1843750006145228, -23.59362340125807123 ) ) ;
#9865 = EDGE_LOOP ( 'NONE', ( #7542, #36939, #8519, #10869 ) ) ;
#9864 = ORIENTED_EDGE ( 'NONE', *, *, #15765, .T. ) ;
#9866 = CARTESIAN_POINT ( 'NONE',  ( 18.12178482187500350, 247.5718750006145115, 4.985214923628407568 ) ) ;
#9867 = CARTESIAN_POINT ( 'NONE',  ( -8.962234695871565293, 26.03981371789855359, -8.715434833792128799 ) ) ;
#9868 = CARTESIAN_POINT ( 'NONE',  ( 18.12178482187500350, -4.985214923628407568, -0.5156249993854555846 ) ) ;
#9869 = CARTESIAN_POINT ( 'NONE',  ( 2.908627838312458636, 128.6773137178985280, -15.53471296425188442 ) ) ;
#9870 = CARTESIAN_POINT ( 'NONE',  ( 24.00000000000000000, -5.196152422706629359, -9.243749998770949716 ) ) ;
#9871 = PLANE ( 'NONE',  #8737 ) ;
#9872 = EDGE_LOOP ( 'NONE', ( #36579, #32194, #28361, #31587 ) ) ;
#9873 = CARTESIAN_POINT ( 'NONE',  ( 19.68408634441911431, 5.407089921784862696, -6.196874999385537208 ) ) ;
#9874 =( GEOMETRIC_REPRESENTATION_CONTEXT ( 3 ) GLOBAL_UNCERTAINTY_ASSIGNED_CONTEXT ( ( #30177 ) ) GLOBAL_UNIT_ASSIGNED_CONTEXT ( ( #6522, #6900, #26793 ) ) REPRESENTATION_CONTEXT ( 'NONE', 'WORKASPACE' ) );
#9875 = ORIENTED_EDGE ( 'NONE', *, *, #28642, .F. ) ;
#9876 = CARTESIAN_POINT ( 'NONE',  ( -13.62178482187500528, 196.1281250006145171, -23.59362340125807123 ) ) ;
#9877 = CARTESIAN_POINT ( 'NONE',  ( 4.622313124798573369, 129.4351862821014549, 11.61527771782819940 ) ) ;
#9878 = AXIS2_PLACEMENT_3D ( 'NONE', #13817, #25364, #37468 ) ;
#9879 = CARTESIAN_POINT ( 'NONE',  ( 30.94147426890365438, -7.209453229046482114, 163.6315708601335359 ) ) ;
#9880 = CARTESIAN_POINT ( 'NONE',  ( -52.56919563604517265, 218.5000000000000000, -0.1155267958018185298 ) ) ;
#9881 = CARTESIAN_POINT ( 'NONE',  ( 15.24356964375000167, 247.0843750006145285, 3.323476615752272600 ) ) ;
#9882 = LINE ( 'NONE', #24109, #35143 ) ;
#9883 = CARTESIAN_POINT ( 'NONE',  ( -43.86086230271183695, 212.1499508600178387, -3.954877714930852495 ) ) ;
#9884 = CARTESIAN_POINT ( 'NONE',  ( 19.39230484541324984, 246.0424038105676630, 5.999999999999991118 ) ) ;
#9885 = CARTESIAN_POINT ( 'NONE',  ( 31.14247720061542424, -7.209453229046475009, 165.9290448826076272 ) ) ;
#9886 = VERTEX_POINT ( 'NONE', #36279 ) ;
#9887 = FACE_OUTER_BOUND ( 'NONE', #27859, .T. ) ;
#9888 = CARTESIAN_POINT ( 'NONE',  ( -11.08355503943142573, 131.1601862821014777, 10.83675517735155402 ) ) ;
#9889 = CARTESIAN_POINT ( 'NONE',  ( -44.06622103062156270, 212.1620413398628671, 8.530955311639223382 ) ) ;
#9890 = CARTESIAN_POINT ( 'NONE',  ( 9.465287035748067623, 109.5976862821014493, 2.064181346179272847 ) ) ;
#9891 = CARTESIAN_POINT ( 'NONE',  ( -20.68320042480036491, 194.9994763866750134, -17.35526491262920246 ) ) ;
#9892 = CARTESIAN_POINT ( 'NONE',  ( 10.49813415415989581, 27.37268628210144783, 7.228626920339068285 ) ) ;
#9893 = CARTESIAN_POINT ( 'NONE',  ( 10.56230152254410548, 0.000000000000000000, -6.750000000000061284 ) ) ;
#9894 = ORIENTED_EDGE ( 'NONE', *, *, #11097, .T. ) ;
#9895 =( NAMED_UNIT ( * ) PLANE_ANGLE_UNIT ( ) SI_UNIT ( $, .RADIAN. ) );
#9896 = CARTESIAN_POINT ( 'NONE',  ( 15.46528703574804986, 127.9976862821014265, 3.257655550457285720 ) ) ;
#9897 = DIRECTION ( 'NONE',  ( 0.8083506638593009885, 0.5887012860850802110, 0.000000000000000000 ) ) ;
#9898 = CARTESIAN_POINT ( 'NONE',  ( -8.843639120294245259, 135.8648137178985849, -3.474262827703533230 ) ) ;
#9899 = CARTESIAN_POINT ( 'NONE',  ( 27.24356964374999635, 199.1656250006145399, -15.72908226750539029 ) ) ;
#9900 = CARTESIAN_POINT ( 'NONE',  ( 15.00000000000000178, 246.9437500012290343, 3.464101615137757051 ) ) ;
#9901 = CARTESIAN_POINT ( 'NONE',  ( -13.50000000000000533, 195.8750000000000284, -23.38268590217984411 ) ) ;
#9902 = CARTESIAN_POINT ( 'NONE',  ( 21.58663455327491221, -3.463016004891044552, -9.999999999999998224 ) ) ;
#9903 = AXIS2_PLACEMENT_3D ( 'NONE', #7125, #6740, #18315 ) ;
#9904 = CYLINDRICAL_SURFACE ( 'NONE', #20689, 2.649999999999992806 ) ;
#9905 = CYLINDRICAL_SURFACE ( 'NONE', #10903, 5.999999999999998224 ) ;
#9906 = CARTESIAN_POINT ( 'NONE',  ( 7.954856959092311719, 74.62731371789853085, -5.529263428287300108 ) ) ;
#9907 = ORIENTED_EDGE ( 'NONE', *, *, #37267, .T. ) ;
#9908 = CARTESIAN_POINT ( 'NONE',  ( 26.99999999999999645, 243.5312500012290400, -7.347880794884117764E-16 ) ) ;
#9909 = CARTESIAN_POINT ( 'NONE',  ( 10.69584247140429589, 76.35231371789855359, 6.932735513424201024 ) ) ;
#9910 = CARTESIAN_POINT ( 'NONE',  ( 13.44051670066911086, -5.407089921784865361, -2.821874999385520777 ) ) ;
#9911 = CARTESIAN_POINT ( 'NONE',  ( -7.578999853579856172, 143.0000000000000284, 10.66724312669795083 ) ) ;
#9912 = CARTESIAN_POINT ( 'NONE',  ( 18.12178482187499640, 4.985214923628404904, -4.378124999385474503 ) ) ;
#9913 = CARTESIAN_POINT ( 'NONE',  ( 7.228626920338837358, 49.32731371789855501, 10.49813415416005036 ) ) ;
#9914 = VECTOR ( 'NONE', #27338, 1000.000000000000000 ) ;
#9915 = VERTEX_POINT ( 'NONE', #19064 ) ;
#9916 = CARTESIAN_POINT ( 'NONE',  ( 18.12178482187499640, 4.985214923628404904, -7.415624999385473259 ) ) ;
#9917 = CARTESIAN_POINT ( 'NONE',  ( 15.24356964375000167, 244.3843750006145115, 3.323476615752272600 ) ) ;
#9918 = CARTESIAN_POINT ( 'NONE',  ( -8.962234695871760692, 29.96018628210143930, 8.715434833791933400 ) ) ;
#9919 = CARTESIAN_POINT ( 'NONE',  ( -38.12127896937849414, 216.5309553116392181, 1.626142955000506429 ) ) ;
#9920 = CARTESIAN_POINT ( 'NONE',  ( -58.30877896937847993, 211.6261429550004607, -6.530955311639245586 ) ) ;
#9921 = CARTESIAN_POINT ( 'NONE',  ( 27.62360488411350801, -5.196152422706632912, 160.1292899952607627 ) ) ;
#9922 = CARTESIAN_POINT ( 'NONE',  ( -10.49813415416004858, 79.22731371789855359, 7.228626920338839135 ) ) ;
#9923 = EDGE_CURVE ( 'NONE', #1210, #5242, #12143, .T. ) ;
#9924 = CARTESIAN_POINT ( 'NONE',  ( -43.07663769728824121, 206.0451222850691408, 2.149950860017832532 ) ) ;
#9925 = VECTOR ( 'NONE', #11328, 1000.000000000000000 ) ;
#9927 = EDGE_CURVE ( 'NONE', #26175, #4869, #2266, .T. ) ;
#9926 = CARTESIAN_POINT ( 'NONE',  ( -57.92038769728821990, 208.1428034533959703, 6.469044688360770401 ) ) ;
#9928 = CARTESIAN_POINT ( 'NONE',  ( 15.24356964374999990, 3.323476615752268604, -7.040624999385501681 ) ) ;
#9929 = DIRECTION ( 'NONE',  ( 1.000000000000000000, 0.000000000000000000, 0.000000000000000000 ) ) ;
#9930 = CARTESIAN_POINT ( 'NONE',  ( -8.632099005475794229, 51.05231371789854222, 13.23911966647199812 ) ) ;
#9931 = CARTESIAN_POINT ( 'NONE',  ( -46.63169563604517265, 210.1155267958018271, 8.500000000000003553 ) ) ;
#9932 = CARTESIAN_POINT ( 'NONE',  ( 13.50000000000001421, 199.7000000000000171, 23.38268590217984055 ) ) ;
#9933 = CARTESIAN_POINT ( 'NONE',  ( 8.962234695871762469, 80.56018628210145494, -8.715434833791931624 ) ) ;
#9934 = CARTESIAN_POINT ( 'NONE',  ( 11.08355503943142750, 25.36018628210144854, -10.83675517735155225 ) ) ;
#9936 = EDGE_CURVE ( 'NONE', #30802, #6034, #21973, .T. ) ;
#9935 = CARTESIAN_POINT ( 'NONE',  ( -80.98946968704737515, 222.6276076386831733, -7.500000000000000000 ) ) ;
#9937 = DIRECTION ( 'NONE',  ( -4.130293990420971855E-17, 1.000000000000000000, 0.000000000000000000 ) ) ;
#9938 = ORIENTED_EDGE ( 'NONE', *, *, #21739, .T. ) ;
#9939 = CARTESIAN_POINT ( 'NONE',  ( 5.770363421893814682, 46.63518628210144357, 14.38691631536207183 ) ) ;
#9940 = CARTESIAN_POINT ( 'NONE',  ( -27.24356964375000345, 197.5156250006145342, -15.72908226750537786 ) ) ;
#9941 = CARTESIAN_POINT ( 'NONE',  ( -13.62178482187500528, 199.7843750006145456, -23.59362340125807123 ) ) ;
#9942 = CARTESIAN_POINT ( 'NONE',  ( 0.000000000000000000, 148.0000000000000000, 0.000000000000000000 ) ) ;
#9943 = CARTESIAN_POINT ( 'NONE',  ( -40.10788769728823411, 216.4690446883607535, 1.857196546604031662 ) ) ;
#9944 = LINE ( 'NONE', #19057, #28021 ) ;
#9945 = CARTESIAN_POINT ( 'NONE',  ( 0.1745138560725515708, 24.21018628210144641, -12.50000000000000355 ) ) ;
#9946 = CARTESIAN_POINT ( 'NONE',  ( 26.75643035624999655, 249.1843750006145228, -7.049594010296217766E-16 ) ) ;
#9947 = CARTESIAN_POINT ( 'NONE',  ( -5.233372021372612259, 133.8523137178985394, 8.152565276336593669 ) ) ;
#9948 = CARTESIAN_POINT ( 'NONE',  ( 26.75643035624999655, 244.6468750006145285, 3.323476615752267271 ) ) ;
#9949 = COLOUR_RGB ( '',0.8941176470588234615, 0.8941176470588234615, 0.8941176470588234615 ) ;
#9950 = ORIENTED_EDGE ( 'NONE', *, *, #23070, .F. ) ;
#9951 = DIRECTION ( 'NONE',  ( 0.000000000000000000, 0.000000000000000000, 1.000000000000000000 ) ) ;
#9952 = CARTESIAN_POINT ( 'NONE',  ( 4.622313124798831829, 128.9648137178985507, -11.61527771782809282 ) ) ;
#9953 = CARTESIAN_POINT ( 'NONE',  ( 10.31873187879411269, 3.604726614523236616, -6.028124999385552130 ) ) ;
#9954 = CARTESIAN_POINT ( 'NONE',  ( 27.83320295094501162, -5.407089921784859143, 163.9223309855715911 ) ) ;
#9955 = CARTESIAN_POINT ( 'NONE',  ( 16.56230152254411081, -6.928203230275506996, -2.474999998771027165 ) ) ;
#9956 = CARTESIAN_POINT ( 'NONE',  ( -13.49999999999998401, 196.9250000000000114, 23.38268590217985476 ) ) ;
#9957 = VERTEX_POINT ( 'NONE', #13844 ) ;
#9958 = CARTESIAN_POINT ( 'NONE',  ( -10.69584247140444866, 57.84768628210144925, 6.932735513423972762 ) ) ;
#9959 = ORIENTED_EDGE ( 'NONE', *, *, #32027, .F. ) ;
#9960 = EDGE_LOOP ( 'NONE', ( #24513, #3917, #5801, #30736 ) ) ;
#9961 = DIRECTION ( 'NONE',  ( -0.000000000000000000, 1.000000000000000000, -0.000000000000000000 ) ) ;
#9962 = CARTESIAN_POINT ( 'NONE',  ( 23.87821517812499650, 4.985214923628404904, -1.190624999385464511 ) ) ;
#9963 = DIRECTION ( 'NONE',  ( -2.057406622567553763E-16, 0.000000000000000000, 1.000000000000000000 ) ) ;
#9964 = CARTESIAN_POINT ( 'NONE',  ( -54.50000000000000711, 244.5000000000000000, 2.500000000000000000 ) ) ;
#9965 = CARTESIAN_POINT ( 'NONE',  ( 26.75643035624999655, -3.323476615752267715, -8.053124999385453009 ) ) ;
#9966 = CARTESIAN_POINT ( 'NONE',  ( 10.69584247140445221, 71.64768628210146062, -6.932735513423970097 ) ) ;
#9967 = CARTESIAN_POINT ( 'NONE',  ( -6.092822981423970496, 139.7851862821014493, 14.25334919248782661 ) ) ;
#9968 = CARTESIAN_POINT ( 'NONE',  ( 13.56230152254411792, -5.196152422706632912, -3.862499998771057541 ) ) ;
#9969 = CARTESIAN_POINT ( 'NONE',  ( 18.00000000000000355, 243.8312500012290513, 5.196152422706632912 ) ) ;
#9970 = CARTESIAN_POINT ( 'NONE',  ( -49.60044563604517265, 206.6211998817775566, -3.209657149897419348 ) ) ;
#9971 = CARTESIAN_POINT ( 'NONE',  ( 19.39230484541324628, 245.4075961894322973, -5.999999999999989342 ) ) ;
#9972 = CARTESIAN_POINT ( 'NONE',  ( 34.24790446256528753, 5.196152422706631135, 167.0031011721061134 ) ) ;
#9973 = CARTESIAN_POINT ( 'NONE',  ( -6.840914352311947333, 7.639813717898540801, -6.594114490232462877 ) ) ;
#9974 = CARTESIAN_POINT ( 'NONE',  ( -51.19122103062155560, 208.3738570449993404, -6.530955311639226935 ) ) ;
#9975 = CARTESIAN_POINT ( 'NONE',  ( -34.55877896937850124, 212.1620413398627534, -8.530955311639255356 ) ) ;
#9976 = APPLICATION_PROTOCOL_DEFINITION ( 'draft international standard', 'automotive_design', 1998, #3005 ) ;
#9977 = CARTESIAN_POINT ( 'NONE',  ( 24.81477950914817754, 0.000000000000000000, 162.4454087870936121 ) ) ;
#9978 = CARTESIAN_POINT ( 'NONE',  ( -27.24356964374999990, 199.3156250006145171, -15.72908226750537786 ) ) ;
#9979 = CARTESIAN_POINT ( 'NONE',  ( 3.257655550456945548, 105.1023137178985678, 15.46528703574811736 ) ) ;
#9980 = CARTESIAN_POINT ( 'NONE',  ( -51.57961230271182274, 211.8571965466040297, 6.469044688360755302 ) ) ;
#9981 = ORIENTED_EDGE ( 'NONE', *, *, #29819, .T. ) ;
#9982 = CARTESIAN_POINT ( 'NONE',  ( 8.715434833791931624, 27.66018628210144215, 8.962234695871760692 ) ) ;
#9983 = CARTESIAN_POINT ( 'NONE',  ( -27.00000000000000355, 196.0625000012290400, 0.000000000000000000 ) ) ;
#9984 = CARTESIAN_POINT ( 'NONE',  ( -7.234628195640328663, 197.8424038105676743, 26.99999999999999289 ) ) ;
#9985 = CARTESIAN_POINT ( 'NONE',  ( 24.91122703310946918, -3.604726614523244610, 166.3424572781808024 ) ) ;
#9986 = CARTESIAN_POINT ( 'NONE',  ( -14.38691631536207183, 104.1351862821014720, 5.770363421893814682 ) ) ;
#9987 = CARTESIAN_POINT ( 'NONE',  ( -59.70163769728823411, 215.6869285224996986, -3.149950860017881382 ) ) ;
#9988 = CARTESIAN_POINT ( 'NONE',  ( 19.68408634441910721, -5.407089921784855591, -4.940624999385550886 ) ) ;
#9989 = CARTESIAN_POINT ( 'NONE',  ( 5.529263428287477744, 43.47268628210144215, -7.954856959092191815 ) ) ;
#9990 = DIRECTION ( 'NONE',  ( 0.000000000000000000, 0.000000000000000000, 1.000000000000000000 ) ) ;
#9991 = CARTESIAN_POINT ( 'NONE',  ( -41.69122103062156270, 207.8379586601371329, -8.530955311639223382 ) ) ;
#9992 = CARTESIAN_POINT ( 'NONE',  ( 0.000000000000000000, 148.0000000000000000, 0.000000000000000000 ) ) ;
#9993 = CARTESIAN_POINT ( 'NONE',  ( 12.53471296425194836, 81.42268628210145209, -2.311890736173178418 ) ) ;
#9994 = CARTESIAN_POINT ( 'NONE',  ( -26.99999999999998934, 199.5874999999999773, 15.58845726811991561 ) ) ;
#9995 = CARTESIAN_POINT ( 'NONE',  ( 10.56230152254410726, 0.000000000000000000, -8.550000000000029132 ) ) ;
#9997 = CARTESIAN_POINT ( 'NONE',  ( 27.97700992647863316, 5.407089921784856479, 165.5660522374229799 ) ) ;
#9996 = CARTESIAN_POINT ( 'NONE',  ( 9.465287035748067623, 45.19768628210142225, 2.064181346179272847 ) ) ;
#9998 = CARTESIAN_POINT ( 'NONE',  ( 2.999999999999997335, 244.5000000000000000, -5.000000000000000000 ) ) ;
#9999 = ORIENTED_EDGE ( 'NONE', *, *, #31251, .T. ) ;
#10000 = CARTESIAN_POINT ( 'NONE',  ( 21.00000000000000000, -6.646953231504538984, -9.928124999385461891 ) ) ;
#10001 = CARTESIAN_POINT ( 'NONE',  ( -62.67038769728823411, 208.1428034533959703, 6.469044688360770401 ) ) ;
#10002 = CARTESIAN_POINT ( 'NONE',  ( 30.84342405831255007, 7.209453229046482114, 162.5108518247803318 ) ) ;
#10003 = CARTESIAN_POINT ( 'NONE',  ( 27.79682692271734012, 5.196152422706636465, 162.1092269564937851 ) ) ;
#10004 = CARTESIAN_POINT ( 'NONE',  ( 24.00000000000000000, 246.1000000000000227, 5.196152422706629359 ) ) ;
#10005 = CARTESIAN_POINT ( 'NONE',  ( 27.24356964374999279, 195.5656250006145171, -15.72908226750539207 ) ) ;
#10006 = CARTESIAN_POINT ( 'NONE',  ( -6.932735513424201912, 78.65231371789855075, 10.69584247140429412 ) ) ;
#10007 = CARTESIAN_POINT ( 'NONE',  ( -12.50000000000000355, 104.7101862821014606, -0.1745138560725492671 ) ) ;
#10008 = ORIENTED_EDGE ( 'NONE', *, *, #25253, .T. ) ;
#10009 = ORIENTED_EDGE ( 'NONE', *, *, #33282, .F. ) ;
#10010 = CARTESIAN_POINT ( 'NONE',  ( -27.00000000000000355, 197.8625000012290513, 0.000000000000000000 ) ) ;
#10011 = CARTESIAN_POINT ( 'NONE',  ( 16.56230152254411081, -6.928203230275506996, -9.224999998771027165 ) ) ;
#10012 = CARTESIAN_POINT ( 'NONE',  ( 13.04141134922778988, 74.62731371789853085, -8.927990412390371944 ) ) ;
#10013 = CARTESIAN_POINT ( 'NONE',  ( 15.24356964375000167, -3.323476615752272600, -6.065624999385484273 ) ) ;
#10014 = AXIS2_PLACEMENT_3D ( 'NONE', #18599, #6457, #18029 ) ;
#10015 = CARTESIAN_POINT ( 'NONE',  ( 15.24356964374999990, 245.8093750006145228, 0.000000000000000000 ) ) ;
#10016 = CARTESIAN_POINT ( 'NONE',  ( -53.36830436395490551, 209.8844732041982297, 4.499999999999996447 ) ) ;
#10017 = CARTESIAN_POINT ( 'NONE',  ( 20.99999999999999645, -6.928203230275506996, -6.581249998770967835 ) ) ;
#10018 = CARTESIAN_POINT ( 'NONE',  ( 2.064181346179061460, 49.90231371789854364, 9.465287035748106703 ) ) ;
#10019 = CARTESIAN_POINT ( 'NONE',  ( 22.80587116629411071, -3.604726614523235284, -7.603124999385553195 ) ) ;
#10020 = CARTESIAN_POINT ( 'NONE',  ( -8.152565276336593669, 108.5523137178985422, -5.233372021372610483 ) ) ;
#10021 = CARTESIAN_POINT ( 'NONE',  ( 15.24356964374999990, 240.2968750006145342, 0.000000000000000000 ) ) ;
#10022 = CARTESIAN_POINT ( 'NONE',  ( -12.46528703574811558, 33.80231371789854933, 2.660918448318003726 ) ) ;
#10023 = CARTESIAN_POINT ( 'NONE',  ( 8.962234695871762469, 80.56018628210145494, -8.715434833791931624 ) ) ;
#10024 = CARTESIAN_POINT ( 'NONE',  ( 16.56230152254410726, 6.928203230275506996, -8.099999998770989862 ) ) ;
#10025 = CYLINDRICAL_SURFACE ( 'NONE', #22585, 27.00000000000000000 ) ;
#10026 = CARTESIAN_POINT ( 'NONE',  ( 24.67427235751429393, 3.604726614523236616, 163.6340529427438639 ) ) ;
#10027 = AXIS2_PLACEMENT_3D ( 'NONE', #1323, #28180, #3979 ) ;
#10028 = CARTESIAN_POINT ( 'NONE',  ( 10.31873187879410736, 0.000000000000000000, -3.796874999385524418 ) ) ;
#10029 = CARTESIAN_POINT ( 'NONE',  ( 26.99999999999999645, 7.347880794884117764E-16, -4.725000000000006750 ) ) ;
#10030 = CARTESIAN_POINT ( 'NONE',  ( 20.99999999999999289, 248.5937500012290400, -5.999999999999997335 ) ) ;
#10031 = CARTESIAN_POINT ( 'NONE',  ( 8.710071997420127943, 100.6851862821014834, 3.796722387233375073 ) ) ;
#10032 = CARTESIAN_POINT ( 'NONE',  ( 15.00000000000000000, 248.2187500012290684, -3.464101615137752610 ) ) ;
#10033 = AXIS2_PLACEMENT_3D ( 'NONE', #13186, #24741, #36291 ) ;
#10034 = CARTESIAN_POINT ( 'NONE',  ( 11.61527771782819940, 136.3351862821014606, -4.622313124798573369 ) ) ;
#10035 =( REPRESENTATION_RELATIONSHIP ('NONE','NONE', #4304, #2638 ) REPRESENTATION_RELATIONSHIP_WITH_TRANSFORMATION ( #27226 )SHAPE_REPRESENTATION_RELATIONSHIP( ) );
#10036 = DIRECTION ( 'NONE',  ( 0.000000000000000000, 0.000000000000000000, 1.000000000000000000 ) ) ;
#10037 = CARTESIAN_POINT ( 'NONE',  ( 23.87821517812500005, 239.9968750006144944, 4.985214923628404016 ) ) ;
#10038 = ORIENTED_EDGE ( 'NONE', *, *, #1533, .T. ) ;
#10039 = CARTESIAN_POINT ( 'NONE',  ( 37.33287311370841621, 7.646167579472015790E-16, 165.0486662223039218 ) ) ;
#10040 = CARTESIAN_POINT ( 'NONE',  ( 21.00000000000000000, 6.646953231504538984, -3.853124999385470595 ) ) ;
#10041 = CARTESIAN_POINT ( 'NONE',  ( 20.99999999999997513, 246.7375000000000398, -5.999999999999999112 ) ) ;
#10043 = LINE ( 'NONE', #2027, #19125 ) ;
#10042 =( BOUNDED_SURFACE ( )  B_SPLINE_SURFACE ( 1, 2, ( 
 ( #6981, #19109, #7537, #18550, #4495, #16072, #15695, #24407, #35956, #4676, #27808, #9994, #36512, #18738, #27428, #30279, #15884, #13035, #24590, #36142, #10183, #33310, #13223, #10556, #22133, #5596, #23053, #16444, #5049, #36702, #34235, #37254, #22502, #8278, #16994, #19302, #13597, #16814, #28174, #16632, #27989, #4864, #17182, #28722, #2019, #7719, #8458, #25702, #7908, #31393, #19851, #2392, #20028, #2579, #5237, #22691, #13785, #14148, #30840, #5413, #11302, #25886, #31573, #10927, #28534, #2204, #37068, #2760, #25332, #25147, #8096, #11114, #34049, #36881, #22870, #19669, #31208, #13966, #28356, #25515, #10741, #34420, #22314, #19481, #14332, #37434, #11484, #33866, #31028, #6877, #2945, #17738, #35672, #14515, #4025, #1369, #20209, #24317, #12940, #35860, #34599, #11850, #20401, #29278, #23419, #99, #8641, #284, #34970, #31942, #9901, #7077, #15790, #17554, #4212, #18644, #9723, #21296, #31758, #32832, #5974, #29089, #30186, #33025, #18452, #3132, #987, #29994, #21485, #34785, #20583, #9013, #32127, #6164, #15597 ),
 ( #3318, #14700, #26249, #5788, #17368, #27339, #28909, #26071, #11663, #23237, #27153, #8829, #1176, #24129, #14889, #26437, #12750, #12563, #1925, #30571, #19391, #24502, #36605, #30934, #5140, #25239, #27713, #13493, #7441, #16346, #36790, #21850, #36048, #24868, #27895, #1743, #19013, #4951, #13309, #10459, #19203, #36416, #22037, #21663, #25051, #7256, #36233, #10645, #33588, #33402, #28268, #13691, #33775, #30376, #7628, #22223, #4398, #16533, #2300, #10093, #10833, #33216, #22408, #18830, #30750, #10275, #4773, #7815, #27529, #15979, #28080, #2113, #4588, #33956, #7998, #16721, #16164, #31122, #19570, #1554, #13126, #24680, #9, #11205, #22778, #34883, #11765, #25978, #34326, #17275, #34692, #3041, #14060, #37341, #17091, #14242, #28630, #37165, #19763, #31301, #14611, #5883, #5329, #26163, #8372, #22964, #2667, #36978, #8188, #25792, #25425, #25608, #16905, #19943, #32036, #23150, #23331, #29187, #22595, #31482, #28446, #2851, #11391, #2484, #17462, #13876, #5507, #14424, #34141, #197, #34511, #8551, #17652, #20118, #8922 ) ),
 .UNSPECIFIED., .F., .F., .F. ) 
 B_SPLINE_SURFACE_WITH_KNOTS ( ( 2, 2 ),
 ( 3, 2, 2, 2, 2, 2, 2, 2, 2, 2, 2, 2, 2, 2, 2, 2, 2, 2, 2, 2, 2, 2, 2, 2, 2, 2, 2, 2, 2, 2, 2, 2, 2, 2, 2, 2, 2, 2, 2, 2, 2, 2, 2, 2, 2, 2, 2, 2, 2, 2, 2, 2, 2, 2, 2, 2, 2, 2, 2, 2, 2, 2, 2, 2, 2, 2, 2, 3 ),
 ( 0.000000000000000000, 1.000000000000000000 ),
 ( 0.000000000000000000, 0.01388888888888888812, 0.02777777777777777624, 0.04166666666666666435, 0.05555555555555555247, 0.06944444444444444753, 0.08333333333333332871, 0.09722222222222222376, 0.1111111111111111049, 0.1250000000000000000, 0.1388888888888888951, 0.1527777777777777901, 0.1666666666666666574, 0.1805555555555555525, 0.1944444444444444475, 0.2083333333333333426, 0.2222222222222222099, 0.2361111111111111049, 0.2500000000000000000, 0.2638888888888888951, 0.2777777777777777901, 0.2916666666666666852, 0.3055555555555555802, 0.3194444444444444198, 0.3333333333333333148, 0.3472222222222222099, 0.3611111111111111049, 0.3750000000000000000, 0.3888888888888888951, 0.4027777777777777901, 0.4166666666666666852, 0.4305555555555555802, 0.4444444444444444198, 0.4583333333333333148, 0.4722222222222222099, 0.4861111111111111049, 0.5000000000000000000, 0.5138888888888888395, 0.5277777777777777901, 0.5416666666666666297, 0.5555555555555555802, 0.5694444444444444198, 0.5833333333333333703, 0.5972222222222222099, 0.6111111111111111605, 0.6250000000000000000, 0.6388888888888888395, 0.6527777777777777901, 0.6666666666666666297, 0.6805555555555555802, 0.6944444444444444198, 0.7083333333333333703, 0.7222222222222222099, 0.7361111111111111605, 0.7500000000000000000, 0.7638888888888888395, 0.7777777777777777901, 0.7916666666666666297, 0.8055555555555555802, 0.8194444444444444198, 0.8333333333333333703, 0.8472222222222222099, 0.8611111111111111605, 0.8750000000000000000, 0.8888888888888888395, 0.9027777777777777901, 0.9166666666666666297, 0.9258785558164617235 ),
 .UNSPECIFIED. ) 
 GEOMETRIC_REPRESENTATION_ITEM ( )  RATIONAL_B_SPLINE_SURFACE ( (
 ( 1.000000000000000000, 0.8660254037844387076, 1.000000000000000000, 0.8660254037844387076, 1.000000000000000000, 0.8660254037844387076, 1.000000000000000000, 0.8660254037844387076, 1.000000000000000000, 0.8660254037844387076, 1.000000000000000000, 0.8660254037844387076, 1.000000000000000000, 0.8660254037844387076, 1.000000000000000000, 0.8660254037844387076, 1.000000000000000000, 0.8660254037844387076, 1.000000000000000000, 0.8660254037844387076, 1.000000000000000000, 0.8660254037844387076, 1.000000000000000000, 0.8660254037844387076, 1.000000000000000000, 0.8660254037844387076, 1.000000000000000000, 0.8660254037844387076, 1.000000000000000000, 0.8660254037844387076, 1.000000000000000000, 0.8660254037844387076, 1.000000000000000000, 0.8660254037844387076, 1.000000000000000000, 0.8660254037844387076, 1.000000000000000000, 0.8660254037844387076, 1.000000000000000000, 0.8660254037844387076, 1.000000000000000000, 0.8660254037844387076, 1.000000000000000000, 0.8660254037844387076, 1.000000000000000000, 0.8660254037844387076, 1.000000000000000000, 0.8660254037844387076, 1.000000000000000000, 0.8660254037844387076, 1.000000000000000000, 0.8660254037844387076, 1.000000000000000000, 0.8660254037844387076, 1.000000000000000000, 0.8660254037844387076, 1.000000000000000000, 0.8660254037844387076, 1.000000000000000000, 0.8660254037844387076, 1.000000000000000000, 0.8660254037844387076, 1.000000000000000000, 0.8660254037844387076, 1.000000000000000000, 0.8660254037844387076, 1.000000000000000000, 0.8660254037844387076, 1.000000000000000000, 0.8660254037844387076, 1.000000000000000000, 0.8660254037844387076, 1.000000000000000000, 0.8660254037844387076, 1.000000000000000000, 0.8660254037844387076, 1.000000000000000000, 0.8660254037844387076, 1.000000000000000000, 0.8660254037844387076, 1.000000000000000000, 0.8660254037844387076, 1.000000000000000000, 0.8660254037844387076, 1.000000000000000000, 0.8660254037844387076, 1.000000000000000000, 0.8660254037844387076, 1.000000000000000000, 0.8660254037844387076, 1.000000000000000000, 0.8660254037844387076, 1.000000000000000000, 0.8660254037844387076, 1.000000000000000000, 0.8660254037844387076, 1.000000000000000000, 0.8660254037844387076, 1.000000000000000000, 0.8660254037844387076, 1.000000000000000000, 0.8660254037844387076, 1.000000000000000000, 0.8660254037844387076, 1.000000000000000000, 0.8660254037844387076, 1.000000000000000000, 0.8660254037844387076, 1.000000000000000000, 0.8660254037844387076, 1.000000000000000000, 0.8660254037844387076, 1.000000000000000000, 0.8660254037844387076, 1.000000000000000000, 0.8660254037844387076, 1.000000000000000000, 0.8660254037844387076, 1.000000000000000000, 0.8660254037844387076, 1.000000000000000000, 0.8660254037844387076, 1.000000000000000000, 0.8660254037844387076, 1.000000000000000000, 0.8660254037844387076, 1.000000000000000000, 0.8660254037844387076, 1.000000000000000000, 0.8660254037844387076, 1.000000000000000000, 0.8660254037844387076, 1.000000000000000000, 0.9111405426957062126, 0.9401542251575389919),
 ( 1.000000000000000000, 0.8660254037844387076, 1.000000000000000000, 0.8660254037844387076, 1.000000000000000000, 0.8660254037844387076, 1.000000000000000000, 0.8660254037844387076, 1.000000000000000000, 0.8660254037844387076, 1.000000000000000000, 0.8660254037844387076, 1.000000000000000000, 0.8660254037844387076, 1.000000000000000000, 0.8660254037844387076, 1.000000000000000000, 0.8660254037844387076, 1.000000000000000000, 0.8660254037844387076, 1.000000000000000000, 0.8660254037844387076, 1.000000000000000000, 0.8660254037844387076, 1.000000000000000000, 0.8660254037844387076, 1.000000000000000000, 0.8660254037844387076, 1.000000000000000000, 0.8660254037844387076, 1.000000000000000000, 0.8660254037844387076, 1.000000000000000000, 0.8660254037844387076, 1.000000000000000000, 0.8660254037844387076, 1.000000000000000000, 0.8660254037844387076, 1.000000000000000000, 0.8660254037844387076, 1.000000000000000000, 0.8660254037844387076, 1.000000000000000000, 0.8660254037844387076, 1.000000000000000000, 0.8660254037844387076, 1.000000000000000000, 0.8660254037844387076, 1.000000000000000000, 0.8660254037844387076, 1.000000000000000000, 0.8660254037844387076, 1.000000000000000000, 0.8660254037844387076, 1.000000000000000000, 0.8660254037844387076, 1.000000000000000000, 0.8660254037844387076, 1.000000000000000000, 0.8660254037844387076, 1.000000000000000000, 0.8660254037844387076, 1.000000000000000000, 0.8660254037844387076, 1.000000000000000000, 0.8660254037844387076, 1.000000000000000000, 0.8660254037844387076, 1.000000000000000000, 0.8660254037844387076, 1.000000000000000000, 0.8660254037844387076, 1.000000000000000000, 0.8660254037844387076, 1.000000000000000000, 0.8660254037844387076, 1.000000000000000000, 0.8660254037844387076, 1.000000000000000000, 0.8660254037844387076, 1.000000000000000000, 0.8660254037844387076, 1.000000000000000000, 0.8660254037844387076, 1.000000000000000000, 0.8660254037844387076, 1.000000000000000000, 0.8660254037844387076, 1.000000000000000000, 0.8660254037844387076, 1.000000000000000000, 0.8660254037844387076, 1.000000000000000000, 0.8660254037844387076, 1.000000000000000000, 0.8660254037844387076, 1.000000000000000000, 0.8660254037844387076, 1.000000000000000000, 0.8660254037844387076, 1.000000000000000000, 0.8660254037844387076, 1.000000000000000000, 0.8660254037844387076, 1.000000000000000000, 0.8660254037844387076, 1.000000000000000000, 0.8660254037844387076, 1.000000000000000000, 0.8660254037844387076, 1.000000000000000000, 0.8660254037844387076, 1.000000000000000000, 0.8660254037844387076, 1.000000000000000000, 0.8660254037844387076, 1.000000000000000000, 0.8660254037844387076, 1.000000000000000000, 0.8660254037844387076, 1.000000000000000000, 0.8660254037844387076, 1.000000000000000000, 0.8660254037844387076, 1.000000000000000000, 0.8660254037844387076, 1.000000000000000000, 0.8660254037844387076, 1.000000000000000000, 0.8660254037844387076, 1.000000000000000000, 0.8660254037844387076, 1.000000000000000000, 0.9111405426957062126, 0.9401542251575389919) ) ) 
 REPRESENTATION_ITEM ( '' )  SURFACE ( )  );
#10044 = CARTESIAN_POINT ( 'NONE',  ( 28.38512818626399081, 5.196152422706636465, 168.8335411686130669 ) ) ;
#10045 = CARTESIAN_POINT ( 'NONE',  ( 13.49999999999999645, 199.5125000012290286, -23.38268590217984766 ) ) ;
#10046 = CARTESIAN_POINT ( 'NONE',  ( 15.24356964374999990, 243.5593750006145228, 0.000000000000000000 ) ) ;
#10047 = EDGE_CURVE ( 'NONE', #24921, #5552, #22003, .T. ) ;
#10048 = CARTESIAN_POINT ( 'NONE',  ( 22.80587116629410360, 7.646167579472015790E-16, -2.165624999385551419 ) ) ;
#10049 = CARTESIAN_POINT ( 'NONE',  ( 5.529263428287300108, 12.52731371789855963, 7.954856959092309943 ) ) ;
#10050 = CARTESIAN_POINT ( 'NONE',  ( -13.62178482187498396, 197.6843750006145228, 23.59362340125808188 ) ) ;
#10052 = VERTEX_POINT ( 'NONE', #10987 ) ;
#10051 = ORIENTED_EDGE ( 'NONE', *, *, #30342, .T. ) ;
#10053 = CARTESIAN_POINT ( 'NONE',  ( 26.75643035624999655, 247.2343750006145058, 3.323476615752267715 ) ) ;
#10054 = CARTESIAN_POINT ( 'NONE',  ( -10.49813415416004858, 24.02731371789855430, 7.228626920338840023 ) ) ;
#10055 = CARTESIAN_POINT ( 'NONE',  ( 26.75643035624999655, 7.049594010296217766E-16, -0.8156249993854780556 ) ) ;
#10056 = CARTESIAN_POINT ( 'NONE',  ( 5.770363421894130873, 128.9648137178985792, -14.38691631536193860 ) ) ;
#10057 = CARTESIAN_POINT ( 'NONE',  ( 21.00000000000000000, -6.646953231504538984, -0.5906249993854776337 ) ) ;
#10058 = EDGE_CURVE ( 'NONE', #31332, #11570, #34106, .T. ) ;
#10059 = ORIENTED_EDGE ( 'NONE', *, *, #36489, .F. ) ;
#10060 = CARTESIAN_POINT ( 'NONE',  ( 19.68408634441911786, -5.407089921784861808, -4.996874999385530813 ) ) ;
#10061 = ORIENTED_EDGE ( 'NONE', *, *, #11969, .T. ) ;
#10062 = CARTESIAN_POINT ( 'NONE',  ( -27.24356964374999990, 195.2656250006145342, -15.72908226750537786 ) ) ;
#10063 = CARTESIAN_POINT ( 'NONE',  ( -10.69584247140444866, 131.4476862821014436, 6.932735513423972762 ) ) ;
#10064 = CARTESIAN_POINT ( 'NONE',  ( 24.67590652769081316, -3.604726614523244610, 163.6527315933331295 ) ) ;
#10065 = EDGE_CURVE ( 'NONE', #2262, #12420, #12265, .T. ) ;
#10066 = AXIS2_PLACEMENT_3D ( 'NONE', #31065, #16667, #10964 ) ;
#10067 =( BOUNDED_SURFACE ( )  B_SPLINE_SURFACE ( 1, 2, ( 
 ( #21040, #32577, #13062, #10213, #21786, #1114, #6618, #19510, #36540, #7746, #4891, #10769, #16471, #2604, #33893, #36352, #31237, #31057, #13814, #5078, #28205, #10583, #2234, #13627, #22162, #28565, #13994, #34076, #30687, #28384, #28016, #16658, #7935, #24801, #10399, #25545, #21975, #37097, #33520, #2048, #33706, #25361, #25178, #27832, #7563, #36908, #19138, #10956, #4705, #22529, #16285, #19329, #1862, #34265, #8126, #19697, #13431, #5267, #36730, #22342, #16845, #2421, #11144, #24980, #22721, #8309, #19881, #31423, #30868, #5443, #17025, #5628, #29503, #37283, #17401, #23269, #23643, #9046, #20434, #14735, #17211, #31785, #9231, #12068, #28752, #14176, #5820, #14920, #29120, #17961, #26469, #34628, #20806, #25918, #2790, #11513, #32348, #6386, #20618, #35003, #23450, #502, #31977, #11331, #25732, #26283, #34449, #32158, #317, #37463, #28941, #132, #6197, #31603, #17588, #11882, #11696, #3163, #17770, #22901, #29312, #8490, #14363, #20059, #8858, #23083, #3352, #8672, #2977, #35186, #20243, #14547, #26101, #34815, #6006 ),
 ( #18905, #21184, #4289, #18532, #7332, #15867, #24019, #10166, #15297, #6574, #879, #36125, #33291, #9978, #12822, #30263, #9610, #3544, #27228, #29691, #18335, #27410, #26850, #15107, #24574, #23829, #26658, #1442, #35748, #12450, #13018, #21559, #12638, #6964, #29883, #9422, #21742, #15487, #32724, #688, #12259, #3914, #32534, #35370, #20997, #9793, #32910, #24390, #35564, #6761, #21371, #27041, #1067, #24203, #30070, #4104, #18150, #15677, #3724, #33104, #1253, #35937, #7148, #18722, #4657, #33849, #19283, #27790, #34217, #19651, #2185, #36305, #34032, #10536, #36684, #2002, #8262, #16054, #31193, #30458, #5218, #4475, #7701, #16240, #13575, #30823, #33473, #27602, #2375, #24755, #4846, #25128, #13386, #13766, #19464, #1817, #10353, #1633, #36864, #10722, #7890, #16425, #27971, #16612, #22296, #13205, #21926, #31011, #8076, #22486, #5032, #28339, #28154, #25312, #24938, #10909, #16794, #36493, #7517, #13950, #19089, #30641, #11099, #25499, #22113, #37051, #33661, #22672, #34952, #23037, #8442, #12022, #8997, #29261, #23221 ) ),
 .UNSPECIFIED., .F., .F., .F. ) 
 B_SPLINE_SURFACE_WITH_KNOTS ( ( 2, 2 ),
 ( 3, 2, 2, 2, 2, 2, 2, 2, 2, 2, 2, 2, 2, 2, 2, 2, 2, 2, 2, 2, 2, 2, 2, 2, 2, 2, 2, 2, 2, 2, 2, 2, 2, 2, 2, 2, 2, 2, 2, 2, 2, 2, 2, 2, 2, 2, 2, 2, 2, 2, 2, 2, 2, 2, 2, 2, 2, 2, 2, 2, 2, 2, 2, 2, 2, 2, 2, 3 ),
 ( 0.000000000000000000, 1.000000000000000000 ),
 ( 0.000000000000000000, 0.01388888888888888812, 0.02777777777777777624, 0.04166666666666666435, 0.05555555555555555247, 0.06944444444444444753, 0.08333333333333332871, 0.09722222222222222376, 0.1111111111111111049, 0.1250000000000000000, 0.1388888888888888951, 0.1527777777777777901, 0.1666666666666666574, 0.1805555555555555525, 0.1944444444444444475, 0.2083333333333333426, 0.2222222222222222099, 0.2361111111111111049, 0.2500000000000000000, 0.2638888888888888951, 0.2777777777777777901, 0.2916666666666666852, 0.3055555555555555802, 0.3194444444444444198, 0.3333333333333333148, 0.3472222222222222099, 0.3611111111111111049, 0.3750000000000000000, 0.3888888888888888951, 0.4027777777777777901, 0.4166666666666666852, 0.4305555555555555802, 0.4444444444444444198, 0.4583333333333333148, 0.4722222222222222099, 0.4861111111111111049, 0.5000000000000000000, 0.5138888888888888395, 0.5277777777777777901, 0.5416666666666666297, 0.5555555555555555802, 0.5694444444444444198, 0.5833333333333333703, 0.5972222222222222099, 0.6111111111111111605, 0.6250000000000000000, 0.6388888888888888395, 0.6527777777777777901, 0.6666666666666666297, 0.6805555555555555802, 0.6944444444444444198, 0.7083333333333333703, 0.7222222222222222099, 0.7361111111111111605, 0.7500000000000000000, 0.7638888888888888395, 0.7777777777777777901, 0.7916666666666666297, 0.8055555555555555802, 0.8194444444444444198, 0.8333333333333333703, 0.8472222222222222099, 0.8611111111111111605, 0.8750000000000000000, 0.8888888888888888395, 0.9027777777777777901, 0.9166666666666666297, 0.9258785558287927486 ),
 .UNSPECIFIED. ) 
 GEOMETRIC_REPRESENTATION_ITEM ( )  RATIONAL_B_SPLINE_SURFACE ( (
 ( 1.000000000000000000, 0.8660254037844387076, 1.000000000000000000, 0.8660254037844387076, 1.000000000000000000, 0.8660254037844387076, 1.000000000000000000, 0.8660254037844387076, 1.000000000000000000, 0.8660254037844387076, 1.000000000000000000, 0.8660254037844387076, 1.000000000000000000, 0.8660254037844387076, 1.000000000000000000, 0.8660254037844387076, 1.000000000000000000, 0.8660254037844387076, 1.000000000000000000, 0.8660254037844387076, 1.000000000000000000, 0.8660254037844387076, 1.000000000000000000, 0.8660254037844387076, 1.000000000000000000, 0.8660254037844387076, 1.000000000000000000, 0.8660254037844387076, 1.000000000000000000, 0.8660254037844387076, 1.000000000000000000, 0.8660254037844387076, 1.000000000000000000, 0.8660254037844387076, 1.000000000000000000, 0.8660254037844387076, 1.000000000000000000, 0.8660254037844387076, 1.000000000000000000, 0.8660254037844387076, 1.000000000000000000, 0.8660254037844387076, 1.000000000000000000, 0.8660254037844387076, 1.000000000000000000, 0.8660254037844387076, 1.000000000000000000, 0.8660254037844387076, 1.000000000000000000, 0.8660254037844387076, 1.000000000000000000, 0.8660254037844387076, 1.000000000000000000, 0.8660254037844387076, 1.000000000000000000, 0.8660254037844387076, 1.000000000000000000, 0.8660254037844387076, 1.000000000000000000, 0.8660254037844387076, 1.000000000000000000, 0.8660254037844387076, 1.000000000000000000, 0.8660254037844387076, 1.000000000000000000, 0.8660254037844387076, 1.000000000000000000, 0.8660254037844387076, 1.000000000000000000, 0.8660254037844387076, 1.000000000000000000, 0.8660254037844387076, 1.000000000000000000, 0.8660254037844387076, 1.000000000000000000, 0.8660254037844387076, 1.000000000000000000, 0.8660254037844387076, 1.000000000000000000, 0.8660254037844387076, 1.000000000000000000, 0.8660254037844387076, 1.000000000000000000, 0.8660254037844387076, 1.000000000000000000, 0.8660254037844387076, 1.000000000000000000, 0.8660254037844387076, 1.000000000000000000, 0.8660254037844387076, 1.000000000000000000, 0.8660254037844387076, 1.000000000000000000, 0.8660254037844387076, 1.000000000000000000, 0.8660254037844387076, 1.000000000000000000, 0.8660254037844387076, 1.000000000000000000, 0.8660254037844387076, 1.000000000000000000, 0.8660254037844387076, 1.000000000000000000, 0.8660254037844387076, 1.000000000000000000, 0.8660254037844387076, 1.000000000000000000, 0.8660254037844387076, 1.000000000000000000, 0.8660254037844387076, 1.000000000000000000, 0.8660254037844387076, 1.000000000000000000, 0.8660254037844387076, 1.000000000000000000, 0.8660254037844387076, 1.000000000000000000, 0.8660254037844387076, 1.000000000000000000, 0.8660254037844387076, 1.000000000000000000, 0.8660254037844387076, 1.000000000000000000, 0.8660254037844387076, 1.000000000000000000, 0.8660254037844387076, 1.000000000000000000, 0.8660254037844387076, 1.000000000000000000, 0.8660254037844387076, 1.000000000000000000, 0.8660254037844387076, 1.000000000000000000, 0.9111405425767590271, 0.9401542252352144136),
 ( 1.000000000000000000, 0.8660254037844387076, 1.000000000000000000, 0.8660254037844387076, 1.000000000000000000, 0.8660254037844387076, 1.000000000000000000, 0.8660254037844387076, 1.000000000000000000, 0.8660254037844387076, 1.000000000000000000, 0.8660254037844387076, 1.000000000000000000, 0.8660254037844387076, 1.000000000000000000, 0.8660254037844387076, 1.000000000000000000, 0.8660254037844387076, 1.000000000000000000, 0.8660254037844387076, 1.000000000000000000, 0.8660254037844387076, 1.000000000000000000, 0.8660254037844387076, 1.000000000000000000, 0.8660254037844387076, 1.000000000000000000, 0.8660254037844387076, 1.000000000000000000, 0.8660254037844387076, 1.000000000000000000, 0.8660254037844387076, 1.000000000000000000, 0.8660254037844387076, 1.000000000000000000, 0.8660254037844387076, 1.000000000000000000, 0.8660254037844387076, 1.000000000000000000, 0.8660254037844387076, 1.000000000000000000, 0.8660254037844387076, 1.000000000000000000, 0.8660254037844387076, 1.000000000000000000, 0.8660254037844387076, 1.000000000000000000, 0.8660254037844387076, 1.000000000000000000, 0.8660254037844387076, 1.000000000000000000, 0.8660254037844387076, 1.000000000000000000, 0.8660254037844387076, 1.000000000000000000, 0.8660254037844387076, 1.000000000000000000, 0.8660254037844387076, 1.000000000000000000, 0.8660254037844387076, 1.000000000000000000, 0.8660254037844387076, 1.000000000000000000, 0.8660254037844387076, 1.000000000000000000, 0.8660254037844387076, 1.000000000000000000, 0.8660254037844387076, 1.000000000000000000, 0.8660254037844387076, 1.000000000000000000, 0.8660254037844387076, 1.000000000000000000, 0.8660254037844387076, 1.000000000000000000, 0.8660254037844387076, 1.000000000000000000, 0.8660254037844387076, 1.000000000000000000, 0.8660254037844387076, 1.000000000000000000, 0.8660254037844387076, 1.000000000000000000, 0.8660254037844387076, 1.000000000000000000, 0.8660254037844387076, 1.000000000000000000, 0.8660254037844387076, 1.000000000000000000, 0.8660254037844387076, 1.000000000000000000, 0.8660254037844387076, 1.000000000000000000, 0.8660254037844387076, 1.000000000000000000, 0.8660254037844387076, 1.000000000000000000, 0.8660254037844387076, 1.000000000000000000, 0.8660254037844387076, 1.000000000000000000, 0.8660254037844387076, 1.000000000000000000, 0.8660254037844387076, 1.000000000000000000, 0.8660254037844387076, 1.000000000000000000, 0.8660254037844387076, 1.000000000000000000, 0.8660254037844387076, 1.000000000000000000, 0.8660254037844387076, 1.000000000000000000, 0.8660254037844387076, 1.000000000000000000, 0.8660254037844387076, 1.000000000000000000, 0.8660254037844387076, 1.000000000000000000, 0.8660254037844387076, 1.000000000000000000, 0.8660254037844387076, 1.000000000000000000, 0.8660254037844387076, 1.000000000000000000, 0.8660254037844387076, 1.000000000000000000, 0.8660254037844387076, 1.000000000000000000, 0.8660254037844387076, 1.000000000000000000, 0.8660254037844387076, 1.000000000000000000, 0.9111405425767590271, 0.9401542252352144136) ) ) 
 REPRESENTATION_ITEM ( '' )  SURFACE ( )  );
#10068 = CARTESIAN_POINT ( 'NONE',  ( -58.70461230271184405, 207.6069050685336492, -8.469044688360751749 ) ) ;
#10069 = CARTESIAN_POINT ( 'NONE',  ( 18.12178482187500350, 246.6718750006145342, 4.985214923628407568 ) ) ;
#10070 =( NAMED_UNIT ( * ) PLANE_ANGLE_UNIT ( ) SI_UNIT ( $, .RADIAN. ) );
#10071 = EDGE_CURVE ( 'NONE', #2262, #26075, #34298, .T. ) ;
#10072 = CARTESIAN_POINT ( 'NONE',  ( 0.000000000000000000, 148.0000000000000000, 0.000000000000000000 ) ) ;
#10073 = CARTESIAN_POINT ( 'NONE',  ( -49.20461230271185116, 208.6787018382582346, -4.469044688360757966 ) ) ;
#10074 = CARTESIAN_POINT ( 'NONE',  ( -2.660918448318275509, 139.4976862821014549, 12.46528703574805874 ) ) ;
#10075 = CARTESIAN_POINT ( 'NONE',  ( 37.45380170677077558, 3.604726614523238837, 166.4308863659062183 ) ) ;
#10077 = ORIENTED_EDGE ( 'NONE', *, *, #13809, .F. ) ;
#10076 = EDGE_CURVE ( 'NONE', #21259, #7355, #7594, .T. ) ;
#10078 = CARTESIAN_POINT ( 'NONE',  ( 26.99999999999999645, 195.4250000012290229, -15.58845726811990495 ) ) ;
#10079 = CARTESIAN_POINT ( 'NONE',  ( 5.770363421894130873, 9.364813717898543999, -14.38691631536193860 ) ) ;
#10080 = CARTESIAN_POINT ( 'NONE',  ( -53.96205436395491262, 216.1378603801730094, 6.307003348497944195 ) ) ;
#10081 = VECTOR ( 'NONE', #16333, 1000.000000000000000 ) ;
#10082 = CARTESIAN_POINT ( 'NONE',  ( -8.710071997420127943, 114.4851862821014663, -3.796722387233380402 ) ) ;
#10083 = CARTESIAN_POINT ( 'NONE',  ( -89.83814373643217266, 60.44923248139874516, 5.000000000000000000 ) ) ;
#10084 = CARTESIAN_POINT ( 'NONE',  ( -10.69584247140444866, 21.04768628210144854, 6.932735513423972762 ) ) ;
#10085 = CARTESIAN_POINT ( 'NONE',  ( 10.56230152254411259, -3.464101615137761048, -6.712500000000003020 ) ) ;
#10086 = ORIENTED_EDGE ( 'NONE', *, *, #16832, .F. ) ;
#10087 = CARTESIAN_POINT ( 'NONE',  ( -32.98288769728823411, 203.5309553116391896, -1.857196546604028997 ) ) ;
#10088 = CARTESIAN_POINT ( 'NONE',  ( 13.04141134922759804, 128.5726862821014436, 8.927990412390657937 ) ) ;
#10089 = DIRECTION ( 'NONE',  ( -0.000000000000000000, 1.000000000000000000, -0.000000000000000000 ) ) ;
#10090 = CARTESIAN_POINT ( 'NONE',  ( 6.840914352312096547, 6.960186282101432198, -6.594114490232313663 ) ) ;
#10091 = CARTESIAN_POINT ( 'NONE',  ( 27.24356964374999635, 199.6156250006145285, -15.72908226750539029 ) ) ;
#10092 = CARTESIAN_POINT ( 'NONE',  ( 15.00000000000000178, 245.0875000000000057, 3.464101615137757051 ) ) ;
#10093 = CARTESIAN_POINT ( 'NONE',  ( -27.24356964374999635, 197.6468750006145285, 15.72908226750539384 ) ) ;
#10094 = CARTESIAN_POINT ( 'NONE',  ( 21.44299373557924682, -3.671490946209025719, -9.999999999999996447 ) ) ;
#10095 = DIRECTION ( 'NONE',  ( 0.000000000000000000, 0.000000000000000000, 1.000000000000000000 ) ) ;
#10096 = CARTESIAN_POINT ( 'NONE',  ( 8.843639120294245259, 66.86481371789854222, 3.474262827703527901 ) ) ;
#10097 = ORIENTED_EDGE ( 'NONE', *, *, #30257, .T. ) ;
#10098 = CARTESIAN_POINT ( 'NONE',  ( 15.00000000000000000, 244.6187500012290172, -3.464101615137752166 ) ) ;
#10099 = CARTESIAN_POINT ( 'NONE',  ( -4.944772684328424539, 81.81481371789855928, -11.48171059495408031 ) ) ;
#10100 = ADVANCED_FACE ( 'NONE', ( #18976 ), #2083, .F. ) ;
#10101 = CARTESIAN_POINT ( 'NONE',  ( 19.68408634441911786, -5.407089921784861808, -4.996874999385530813 ) ) ;
#10102 = CARTESIAN_POINT ( 'NONE',  ( 26.97716818855048260, 0.000000000000000000, 49.47706554351410801 ) ) ;
#10103 = CARTESIAN_POINT ( 'NONE',  ( 15.24356964374999990, 0.000000000000000000, -4.753124999385488714 ) ) ;
#10104 = CARTESIAN_POINT ( 'NONE',  ( 12.53471296425189330, 48.17731371789854933, 2.311890736173451977 ) ) ;
#10105 = ORIENTED_EDGE ( 'NONE', *, *, #10824, .T. ) ;
#10106 = CARTESIAN_POINT ( 'NONE',  ( 26.04366382382454859, 3.734992565117459140, -7.968838429997217254 ) ) ;
#10107 = CARTESIAN_POINT ( 'NONE',  ( 15.24356964375000167, 243.4843750006145058, 3.323476615752272600 ) ) ;
#10108 = CARTESIAN_POINT ( 'NONE',  ( -2.660918448318275509, 29.09768628210144925, 12.46528703574805874 ) ) ;
#10109 = ADVANCED_FACE ( 'NONE', ( #30533, #28786 ), #26640, .F. ) ;
#10110 = CARTESIAN_POINT ( 'NONE',  ( -43.86086230271183695, 213.1499508600178387, -5.686928522499747451 ) ) ;
#10111 = CARTESIAN_POINT ( 'NONE',  ( -54.94419563604517265, 203.5000000000000000, 0.1155267958017914542 ) ) ;
#10112 = EDGE_CURVE ( 'NONE', #20463, #29417, #2955, .T. ) ;
#10113 = DIRECTION ( 'NONE',  ( 0.000000000000000000, 0.000000000000000000, 1.000000000000000000 ) ) ;
#10114 = CARTESIAN_POINT ( 'NONE',  ( -8.962234695871565293, 72.03981371789855359, -8.715434833792128799 ) ) ;
#10115 = CARTESIAN_POINT ( 'NONE',  ( -50.20163769728823411, 213.9548777149308592, -2.149950860017830756 ) ) ;
#10116 = CARTESIAN_POINT ( 'NONE',  ( -57.12872103062157692, 203.4690446883607535, 1.626142955000567936 ) ) ;
#10117 = CARTESIAN_POINT ( 'NONE',  ( 22.56230152254503452, 3.464101615137219259, -1.874999998771022636 ) ) ;
#10118 = CARTESIAN_POINT ( 'NONE',  ( 16.56230152254410726, 0.000000000000000000, -10.00000000000000000 ) ) ;
#10119 = CARTESIAN_POINT ( 'NONE',  ( -8.927990412390371944, 63.12731371789852375, -13.04141134922778988 ) ) ;
#10120 = CARTESIAN_POINT ( 'NONE',  ( -42.87127896937849414, 218.5309553116392465, 2.162041339862725842 ) ) ;
#10121 = CARTESIAN_POINT ( 'NONE',  ( 20.00000000000024869, -5.916079783099657874, -7.999999999999998224 ) ) ;
#10122 = CARTESIAN_POINT ( 'NONE',  ( 7.228626920339068285, 89.47268628210144925, -10.49813415415989581 ) ) ;
#10123 = CARTESIAN_POINT ( 'NONE',  ( -13.04141134922759804, 31.97268628210143149, -8.927990412390657937 ) ) ;
#10124 = CARTESIAN_POINT ( 'NONE',  ( 22.46128102716605923, 1.096376214649937619, -10.00000000000000000 ) ) ;
#10125 = CARTESIAN_POINT ( 'NONE',  ( -4.694659320240884604E-14, 197.5250000012290172, 27.00000000000000000 ) ) ;
#10126 = EDGE_LOOP ( 'NONE', ( #37387, #24919, #12050, #3054 ) ) ;
#10127 = CARTESIAN_POINT ( 'NONE',  ( -15.53471296425195369, 30.82268628210143291, 2.908627838312118019 ) ) ;
#10128 = AXIS2_PLACEMENT_3D ( 'NONE', #5524, #28465, #20137 ) ;
#10129 = CARTESIAN_POINT ( 'NONE',  ( -1.926257025242585782E-15, 197.4406250006145740, -31.45816453501076637 ) ) ;
#10130 = CARTESIAN_POINT ( 'NONE',  ( 3.306546357697854128E-15, 200.0000000000000000, 27.00000000000000355 ) ) ;
#10131 = CARTESIAN_POINT ( 'NONE',  ( -13.49999999999998401, 199.1750000000000114, 23.38268590217985476 ) ) ;
#10132 = CARTESIAN_POINT ( 'NONE',  ( -40.30580436395489841, 216.5000000000000000, 0.1155267958017343610 ) ) ;
#10133 = CARTESIAN_POINT ( 'NONE',  ( -26.99999999999999645, 195.5374999999999943, 15.58845726811991561 ) ) ;
#10134 = CARTESIAN_POINT ( 'NONE',  ( 10.49813415415989581, 18.17268628210144854, 7.228626920339068285 ) ) ;
#10135 = FACE_OUTER_BOUND ( 'NONE', #15985, .T. ) ;
#10136 = CARTESIAN_POINT ( 'NONE',  ( 1.715153634034445762, 137.8773137178985735, -9.534712964251895073 ) ) ;
#10137 = CARTESIAN_POINT ( 'NONE',  ( 20.99999999999999645, 244.7968750006145342, -6.646953231504538984 ) ) ;
#10138 = ORIENTED_EDGE ( 'NONE', *, *, #26533, .T. ) ;
#10139 = DIRECTION ( 'NONE',  ( 0.08715574274765150453, 0.000000000000000000, 0.9961946980917461003 ) ) ;
#10140 = EDGE_CURVE ( 'NONE', #20388, #12454, #35382, .T. ) ;
#10141 = CARTESIAN_POINT ( 'NONE',  ( -10.69584247140429412, 126.9523137178985621, -6.932735513424201024 ) ) ;
#10142 = CARTESIAN_POINT ( 'NONE',  ( 13.44051670066911619, -5.407089921784859143, -7.265624999385544847 ) ) ;
#10143 = CARTESIAN_POINT ( 'NONE',  ( 30.96598682155142868, 7.209453229046475009, 163.9117506189718370 ) ) ;
#10144 = DIRECTION ( 'NONE',  ( -0.000000000000000000, -1.000000000000000000, -0.000000000000000000 ) ) ;
#10145 = CARTESIAN_POINT ( 'NONE',  ( 27.00000000000000355, 197.0749999999999886, -3.306546357697854128E-15 ) ) ;
#10146 = ORIENTED_EDGE ( 'NONE', *, *, #31383, .F. ) ;
#10147 = CARTESIAN_POINT ( 'NONE',  ( -12.50000000000000355, 31.11018628210143788, -0.1745138560725492671 ) ) ;
#10148 = EDGE_LOOP ( 'NONE', ( #33076, #37000 ) ) ;
#10149 = ORIENTED_EDGE ( 'NONE', *, *, #29307, .F. ) ;
#10150 = DIRECTION ( 'NONE',  ( -0.000000000000000000, -1.000000000000000000, -0.000000000000000000 ) ) ;
#10151 = CARTESIAN_POINT ( 'NONE',  ( 20.99999999999999645, -6.646953231504538984, -0.4781249993854547187 ) ) ;
#10152 = CARTESIAN_POINT ( 'NONE',  ( -13.49999999999998401, 199.2875000012290627, 23.38268590217985476 ) ) ;
#10153 = CARTESIAN_POINT ( 'NONE',  ( 21.00000000000000000, -6.646953231504538984, -7.678124999385482319 ) ) ;
#10154 = CARTESIAN_POINT ( 'NONE',  ( -2.660918448318275509, 84.29768628210145209, 12.46528703574805874 ) ) ;
#10155 = CARTESIAN_POINT ( 'NONE',  ( 5.770363421893814682, 138.6351862821014720, 14.38691631536207183 ) ) ;
#10156 = CARTESIAN_POINT ( 'NONE',  ( 36.75931086529713099, 7.347880794884117764E-16, 161.2874679718108553 ) ) ;
#10157 = CARTESIAN_POINT ( 'NONE',  ( 22.56230152254444832, 3.464101615137555878, -5.024999998771018106 ) ) ;
#10158 = CARTESIAN_POINT ( 'NONE',  ( -49.20461230271185116, 208.6787018382582346, -4.469044688360757966 ) ) ;
#10159 = CARTESIAN_POINT ( 'NONE',  ( 15.00000000000000355, 7.347880794884112834E-16, 50.26196565745150480 ) ) ;
#10160 = CARTESIAN_POINT ( 'NONE',  ( 34.16946429409239983, 5.196152422706631135, 166.1065259438235557 ) ) ;
#10161 = CARTESIAN_POINT ( 'NONE',  ( -8.715434833792127023, 143.3398137178985507, 8.962234695871568846 ) ) ;
#10162 = CARTESIAN_POINT ( 'NONE',  ( -46.44122103062156270, 208.3738570449993404, -6.530955311639226935 ) ) ;
#10163 = CARTESIAN_POINT ( 'NONE',  ( -61.08705436395490551, 203.8621396198270475, -6.307003348497942419 ) ) ;
#10164 = CONTEXT_DEPENDENT_SHAPE_REPRESENTATION ( #32056, #23802 ) ;
#10165 = CARTESIAN_POINT ( 'NONE',  ( 23.87821517812499650, 4.985214923628404904, -1.753124999385485827 ) ) ;
#10166 = CARTESIAN_POINT ( 'NONE',  ( 27.24356964375000700, 199.5406250006145683, 15.72908226750537075 ) ) ;
#10167 = VECTOR ( 'NONE', #1177, 1000.000000000000000 ) ;
#10168 = CARTESIAN_POINT ( 'NONE',  ( 14.38691631536194393, 122.0648137178985877, 5.770363421894124656 ) ) ;
#10169 = CARTESIAN_POINT ( 'NONE',  ( -46.63169563604516554, 210.1155267958017703, 6.500000000000000888 ) ) ;
#10170 = VERTEX_POINT ( 'NONE', #5476 ) ;
#10171 = CARTESIAN_POINT ( 'NONE',  ( 37.22668353578169587, -3.464101615137590073, 166.6295620403278122 ) ) ;
#10172 = CARTESIAN_POINT ( 'NONE',  ( -12.50000000000000355, 132.3101862821014549, -0.1745138560725492671 ) ) ;
#10173 = FACE_OUTER_BOUND ( 'NONE', #6359, .T. ) ;
#10174 = CARTESIAN_POINT ( 'NONE',  ( 37.20704201011650269, -3.604726614523238837, 163.6104101269339424 ) ) ;
#10175 = CARTESIAN_POINT ( 'NONE',  ( 14.38691631536207538, 99.53518628210146346, -5.770363421893813793 ) ) ;
#10176 = CARTESIAN_POINT ( 'NONE',  ( -58.51413769728823411, 213.1499508600178672, 5.686928522499718142 ) ) ;
#10177 = CARTESIAN_POINT ( 'NONE',  ( 13.44051670066911086, 5.407089921784856479, -4.265624999385542182 ) ) ;
#10178 = CARTESIAN_POINT ( 'NONE',  ( -8.152565276336710909, 48.64768628210144641, 5.233372021372435512 ) ) ;
#10179 = EDGE_CURVE ( 'NONE', #35635, #34832, #23778, .T. ) ;
#10180 = CARTESIAN_POINT ( 'NONE',  ( -32.58705436395489841, 203.8621396198270475, -6.307003348497942419 ) ) ;
#10181 = CARTESIAN_POINT ( 'NONE',  ( 22.80587116629412492, 3.604726614523243278, -9.834374999385516958 ) ) ;
#10182 = CARTESIAN_POINT ( 'NONE',  ( -2.311890736173176641, 69.92268628210146630, -12.53471296425194836 ) ) ;
#10183 = CARTESIAN_POINT ( 'NONE',  ( 13.50000000000001421, 199.2500000000000000, 23.38268590217984055 ) ) ;
#10184 = CARTESIAN_POINT ( 'NONE',  ( 1.069080835302379631E-14, 199.2125000000000057, 27.00000000000000000 ) ) ;
#10186 = CARTESIAN_POINT ( 'NONE',  ( 13.44051670066911264, -5.407089921784865361, -1.921874999385508875 ) ) ;
#10185 = CARTESIAN_POINT ( 'NONE',  ( -1.715153634034234598, 42.32268628210145067, -9.534712964251941258 ) ) ;
#10187 = CARTESIAN_POINT ( 'NONE',  ( 19.39230484541326049, 241.8075961894323029, -5.999999999999997335 ) ) ;
#10189 = EDGE_CURVE ( 'NONE', #34895, #24301, #8502, .T. ) ;
#10188 = ORIENTED_EDGE ( 'NONE', *, *, #5172, .F. ) ;
#10190 = CARTESIAN_POINT ( 'NONE',  ( 18.00000000000000000, 5.196152422706630247, -2.324999999999993960 ) ) ;
#10191 = CARTESIAN_POINT ( 'NONE',  ( 24.59092967851185207, 3.604726614523240613, 162.6814417626936518 ) ) ;
#10192 = CARTESIAN_POINT ( 'NONE',  ( 33.76745843056175289, 5.196152422706637353, 161.5115778976509944 ) ) ;
#10193 = CARTESIAN_POINT ( 'NONE',  ( 21.00000000000000000, 244.9375000000000000, -6.928203230275506996 ) ) ;
#10194 = CARTESIAN_POINT ( 'NONE',  ( -29.00000000000002487, 215.7563705986615901, -5.555555555555559799 ) ) ;
#10195 = EDGE_CURVE ( 'NONE', #36001, #29181, #36822, .T. ) ;
#10196 = CARTESIAN_POINT ( 'NONE',  ( -8.962234695871565293, 90.43981371789855928, -8.715434833792128799 ) ) ;
#10197 = CARTESIAN_POINT ( 'NONE',  ( 12.46528703574805874, 81.99768628210145494, 2.660918448318279950 ) ) ;
#10198 = ORIENTED_EDGE ( 'NONE', *, *, #8299, .F. ) ;
#10199 = VECTOR ( 'NONE', #31261, 1000.000000000000000 ) ;
#10200 = ORIENTED_EDGE ( 'NONE', *, *, #30521, .F. ) ;
#10201 = PRODUCT_DEFINITION ( 'UNKNOWN', '', #22055, #26269 ) ;
#10202 = CARTESIAN_POINT ( 'NONE',  ( 13.49999999999999645, 197.7125000012290172, -23.38268590217984766 ) ) ;
#10203 = CARTESIAN_POINT ( 'NONE',  ( 15.00000000000000000, 248.7062500012290229, 0.000000000000000000 ) ) ;
#10204 = CARTESIAN_POINT ( 'NONE',  ( -11.08355503943118592, 62.83981371789855785, -10.83675517735179383 ) ) ;
#10205 = CARTESIAN_POINT ( 'NONE',  ( 23.87821517812500005, -4.985214923628404016, -7.303124999385484983 ) ) ;
#10206 = CARTESIAN_POINT ( 'NONE',  ( 26.75643035624999655, 245.1343750006145115, -7.049594010296217766E-16 ) ) ;
#10207 = CARTESIAN_POINT ( 'NONE',  ( -53.17038769728823411, 208.6787018382581778, 4.469044688360752637 ) ) ;
#10208 = CARTESIAN_POINT ( 'NONE',  ( 23.99999999999999645, 243.1562500012290400, -5.196152422706631135 ) ) ;
#10209 = CARTESIAN_POINT ( 'NONE',  ( 9.534712964251900402, 57.37731371789855928, 1.715153634034445540 ) ) ;
#10210 = CARTESIAN_POINT ( 'NONE',  ( 13.44051670066911619, -5.407089921784859143, -7.715624999385550353 ) ) ;
#10211 = AXIS2_PLACEMENT_3D ( 'NONE', #33299, #1259, #7339 ) ;
#10212 = CARTESIAN_POINT ( 'NONE',  ( 0.1745138560723095977, 105.3898137178985479, 9.500000000000005329 ) ) ;
#10213 = CARTESIAN_POINT ( 'NONE',  ( -1.926257025242585782E-15, 199.7468750006145513, -31.45816453501075927 ) ) ;
#10214 = CARTESIAN_POINT ( 'NONE',  ( 10.69584247140429589, 30.35231371789855359, 6.932735513424201024 ) ) ;
#10215 = CARTESIAN_POINT ( 'NONE',  ( -4.622313124798576922, 78.83518628210146062, -11.61527771782819762 ) ) ;
#10216 = CARTESIAN_POINT ( 'NONE',  ( 13.56230152254410548, 5.196152422706630247, -8.512499998770989507 ) ) ;
#10217 = CARTESIAN_POINT ( 'NONE',  ( 13.49999999999999645, 196.2500000000000000, -23.38268590217984766 ) ) ;
#10218 = CARTESIAN_POINT ( 'NONE',  ( 24.59583218904140978, 3.604726614523236616, 162.7374777144612779 ) ) ;
#10219 = CARTESIAN_POINT ( 'NONE',  ( 19.68408634441911431, -5.407089921784861808, -5.896874999385542715 ) ) ;
#10220 = CARTESIAN_POINT ( 'NONE',  ( -7.234628195640328663, 197.8424038105676743, 26.99999999999999289 ) ) ;
#10221 = CARTESIAN_POINT ( 'NONE',  ( 24.00000000000000000, -5.196152422706629359, -3.843749998770962240 ) ) ;
#10222 = DIRECTION ( 'NONE',  ( 0.000000000000000000, 0.000000000000000000, -1.000000000000000000 ) ) ;
#10223 = CARTESIAN_POINT ( 'NONE',  ( 9.534712964251941258, 99.82268628210142936, -1.715153634034235708 ) ) ;
#10224 = CARTESIAN_POINT ( 'NONE',  ( 16.56230152254410726, 0.000000000000000000, -10.00000000000000000 ) ) ;
#10225 = CARTESIAN_POINT ( 'NONE',  ( -2.311890736173176641, 134.3226862821014436, -12.53471296425194836 ) ) ;
#10226 = DIRECTION ( 'NONE',  ( -0.9925324990730152175, 0.1219804832088933616, 0.000000000000000000 ) ) ;
#10227 = CARTESIAN_POINT ( 'NONE',  ( 26.75643035624999655, 241.0093750006144830, -3.323476615752271712 ) ) ;
#10228 = EDGE_LOOP ( 'NONE', ( #23702, #4805, #8471, #29708, #35245, #3368, #31267, #31177, #24684, #10149, #14924, #11173, #773, #23433, #14704, #9404, #28967, #33137, #27626, #37011, #18458, #37479, #19196, #31222, #17591, #14716, #24736, #4500, #10077, #27748, #12658, #7181, #10427, #26265, #21309, #19263, #13602, #9757, #35338, #5378, #20013, #2774, #23288, #4402, #28047, #19356, #22556, #35706 ) ) ;
#10229 = CARTESIAN_POINT ( 'NONE',  ( 37.17599277676264080, 7.646167579472015790E-16, 163.2555157657388065 ) ) ;
#10230 = CARTESIAN_POINT ( 'NONE',  ( 21.00000000000000000, 6.646953231504538984, -5.203124999385457805 ) ) ;
#10231 = CARTESIAN_POINT ( 'NONE',  ( 5.778771075727756162E-15, 198.1718750006145342, 31.45816453501076637 ) ) ;
#10232 = CARTESIAN_POINT ( 'NONE',  ( 31.35083389806797527, -6.928203230275514990, 168.3105728321210393 ) ) ;
#10233 = CARTESIAN_POINT ( 'NONE',  ( 15.00000000000000355, 7.347880794884112834E-16, -8.000000000000000000 ) ) ;
#10234 = CARTESIAN_POINT ( 'NONE',  ( 21.00000000000000000, 242.7718750006145854, 6.646953231504538984 ) ) ;
#10235 = CARTESIAN_POINT ( 'NONE',  ( -0.1745138560722763466, 137.5898137178985792, -12.50000000000000355 ) ) ;
#10236 = CARTESIAN_POINT ( 'NONE',  ( -27.24356964374999279, 196.7468750006145513, 15.72908226750539384 ) ) ;
#10238 = ORIENTED_EDGE ( 'NONE', *, *, #23118, .F. ) ;
#10237 = ORIENTED_EDGE ( 'NONE', *, *, #3391, .T. ) ;
#10239 = CARTESIAN_POINT ( 'NONE',  ( 21.00000000000000000, 244.4593750006145001, 6.646953231504538984 ) ) ;
#10240 = CARTESIAN_POINT ( 'NONE',  ( -11.48171059495408208, 33.51481371789854791, 4.944772684328421875 ) ) ;
#10241 = CARTESIAN_POINT ( 'NONE',  ( 23.87821517812499650, 4.985214923628404904, -3.890624999385472460 ) ) ;
#10242 = CARTESIAN_POINT ( 'NONE',  ( 13.04141134922778988, 120.6273137178985451, -8.927990412390371944 ) ) ;
#10243 = CARTESIAN_POINT ( 'NONE',  ( 15.00000000000000000, 3.464101615137752166, -9.881249998770957887 ) ) ;
#10244 = EDGE_CURVE ( 'NONE', #27444, #35917, #20090, .T. ) ;
#10245 = ORIENTED_EDGE ( 'NONE', *, *, #3572, .T. ) ;
#10246 = CARTESIAN_POINT ( 'NONE',  ( 22.80587116629412492, 3.604726614523243278, -6.234374999385519089 ) ) ;
#10247 = ORIENTED_EDGE ( 'NONE', *, *, #1776, .F. ) ;
#10248 = CARTESIAN_POINT ( 'NONE',  ( 27.24356964375000700, 196.3906250006145058, 15.72908226750537075 ) ) ;
#10249 = CARTESIAN_POINT ( 'NONE',  ( 11.61527771782819940, 127.1351862821014578, -4.622313124798573369 ) ) ;
#10250 = CARTESIAN_POINT ( 'NONE',  ( 10.31873187879410736, -3.604726614523240613, -0.5531249993855127389 ) ) ;
#10251 = CARTESIAN_POINT ( 'NONE',  ( 30.68654372136677821, 7.209453229046482114, 160.7177013682151596 ) ) ;
#10252 = CARTESIAN_POINT ( 'NONE',  ( -50.19419563604517975, 201.5000000000000000, 0.1155267958018195706 ) ) ;
#10253 = CARTESIAN_POINT ( 'NONE',  ( 26.75643035624999655, 246.8218750006145115, -7.049594010296217766E-16 ) ) ;
#10254 = DIRECTION ( 'NONE',  ( 0.08715574274765150453, 0.000000000000000000, 0.9961946980917461003 ) ) ;
#10255 = CARTESIAN_POINT ( 'NONE',  ( -41.48586230271182984, 207.8500491399821613, 3.954877714930852495 ) ) ;
#10257 = EDGE_CURVE ( 'NONE', #24412, #20178, #16043, .T. ) ;
#10256 = CARTESIAN_POINT ( 'NONE',  ( 2.311890736173175753, 138.9226862821014663, 12.53471296425194836 ) ) ;
#10258 = CARTESIAN_POINT ( 'NONE',  ( 16.56230152254411436, 6.928203230275506996, -0.8999999987709939031 ) ) ;
#10259 = EDGE_LOOP ( 'NONE', ( #16320, #36183, #33664, #12933 ) ) ;
#10260 = LINE ( 'NONE', #33576, #2793 ) ;
#10261 = EDGE_CURVE ( 'NONE', #952, #18435, #20279, .T. ) ;
#10262 = CARTESIAN_POINT ( 'NONE',  ( 2.908627838312118019, 111.3226862821014578, 15.53471296425195369 ) ) ;
#10263 = CARTESIAN_POINT ( 'NONE',  ( 5.233372021372432847, 110.7476862821014691, 8.152565276336710909 ) ) ;
#10264 =( BOUNDED_CURVE ( )  B_SPLINE_CURVE ( 2, ( #13146, #1764, #22427, #31320, #19592, #31141, #2503 ),
 .UNSPECIFIED., .F., .F. ) 
 B_SPLINE_CURVE_WITH_KNOTS ( ( 3, 2, 2, 3 ),
 ( 0.7173913043478249429, 0.7246376811594192890, 0.7318840579710136351, 0.7391304347826078702 ),
 .UNSPECIFIED. ) 
 CURVE ( )  GEOMETRIC_REPRESENTATION_ITEM ( )  RATIONAL_B_SPLINE_CURVE ( ( 1.000000000000020428, 0.8660254037844181685, 1.000000000000000000, 0.8660254037844387076, 1.000000000000000000, 0.8660254037844530295, 0.9999999999999856781 ) ) 
 REPRESENTATION_ITEM ( '' )  );
#10265 = DIRECTION ( 'NONE',  ( -0.000000000000000000, -0.000000000000000000, -1.000000000000000000 ) ) ;
#10266 = CARTESIAN_POINT ( 'NONE',  ( 7.228626920339068285, 6.672686282101436106, -10.49813415415989581 ) ) ;
#10267 = CARTESIAN_POINT ( 'NONE',  ( 13.56230152254410726, 5.196152422706636465, -8.175000000000043343 ) ) ;
#10268 = ORIENTED_EDGE ( 'NONE', *, *, #32424, .T. ) ;
#10269 = FACE_OUTER_BOUND ( 'NONE', #29814, .T. ) ;
#10270 = CARTESIAN_POINT ( 'NONE',  ( -5.233372021372430183, 87.74768628210144072, -8.152565276336710909 ) ) ;
#10271 = DIRECTION ( 'NONE',  ( -0.5887012860850814322, 0.8083506638593001004, 0.000000000000000000 ) ) ;
#10272 = CARTESIAN_POINT ( 'NONE',  ( -5.233372021372612259, 133.8523137178985394, 8.152565276336593669 ) ) ;
#10273 = CARTESIAN_POINT ( 'NONE',  ( 27.24356964375000345, 195.9781250006145399, -3.336375036156643733E-15 ) ) ;
#10274 = CARTESIAN_POINT ( 'NONE',  ( 2.999999999999997335, 244.5000000000000000, -5.000000000000000000 ) ) ;
#10275 = CARTESIAN_POINT ( 'NONE',  ( 27.24356964374999635, 197.4218750006145342, -15.72908226750539029 ) ) ;
#10276 = CARTESIAN_POINT ( 'NONE',  ( 27.00000000000058620, -3.464101615137410661, -1.556249998770949716 ) ) ;
#10277 = ADVANCED_FACE ( 'NONE', ( #5854, #31452 ), #4088, .F. ) ;
#10278 = CARTESIAN_POINT ( 'NONE',  ( 24.67097253372098820, -3.464101615137358703, 160.8016875364666305 ) ) ;
#10279 = CARTESIAN_POINT ( 'NONE',  ( -3.796722387233185003, 63.41481371789855359, -8.710071997420207879 ) ) ;
#10280 = ORIENTED_EDGE ( 'NONE', *, *, #28353, .F. ) ;
#10281 = CARTESIAN_POINT ( 'NONE',  ( 26.99999999999999645, 244.9187500012290286, -3.464101615137755275 ) ) ;
#10282 = CARTESIAN_POINT ( 'NONE',  ( 6.932735513424201024, 83.25231371789857349, -10.69584247140429412 ) ) ;
#10283 = CARTESIAN_POINT ( 'NONE',  ( 16.56230152254411436, 7.209453229046482114, -7.509374999385480365 ) ) ;
#10284 = LINE ( 'NONE', #21495, #25755 ) ;
#10285 = CARTESIAN_POINT ( 'NONE',  ( 15.24356964375000167, -3.323476615752272600, -7.865624999385466332 ) ) ;
#10286 = CARTESIAN_POINT ( 'NONE',  ( -4.944772684328424539, 45.01481371789854791, -11.48171059495408031 ) ) ;
#10287 = EDGE_CURVE ( 'NONE', #29663, #11836, #21908, .T. ) ;
#10288 =( BOUNDED_CURVE ( )  B_SPLINE_CURVE ( 2, ( #4442, #24171, #6926, #12417, #35532, #21151, #23797, #35715, #15263 ),
 .UNSPECIFIED., .F., .F. ) 
 B_SPLINE_CURVE_WITH_KNOTS ( ( 3, 2, 2, 2, 3 ),
 ( 0.2065217391304347838, 0.2101449275362318736, 0.2173913043478260809, 0.2246376811594202882, 0.2282608695652173780 ),
 .UNSPECIFIED. ) 
 CURVE ( )  GEOMETRIC_REPRESENTATION_ITEM ( )  RATIONAL_B_SPLINE_CURVE ( ( 0.9330127018922194093, 0.9330127018922194093, 1.000000000000000000, 0.8660254037844387076, 1.000000000000000000, 0.8660254037844387076, 1.000000000000000000, 0.9330127018922196314, 0.9330127018922194093 ) ) 
 REPRESENTATION_ITEM ( '' )  );
#10289 = EDGE_LOOP ( 'NONE', ( #3035, #23545, #21906, #28663 ) ) ;
#10290 = CARTESIAN_POINT ( 'NONE',  ( 15.24356964374999990, 3.323476615752268604, -6.478124999385451055 ) ) ;
#10291 = CARTESIAN_POINT ( 'NONE',  ( 12.50000000000000355, 26.51018628210144357, 0.1745138560725507937 ) ) ;
#10292 = CARTESIAN_POINT ( 'NONE',  ( 34.44684893975629336, -5.407089921784861808, 167.8797228278759803 ) ) ;
#10293 = VECTOR ( 'NONE', #19798, 1000.000000000000000 ) ;
#10294 = CARTESIAN_POINT ( 'NONE',  ( -55.73586230271182984, 206.8500491399821328, 5.686928522499748340 ) ) ;
#10295 = CARTESIAN_POINT ( 'NONE',  ( 24.70365593725203368, 3.464101615137752166, 161.1752605482509750 ) ) ;
#10296 = CARTESIAN_POINT ( 'NONE',  ( -8.715434833792127023, 69.73981371789855643, 8.962234695871568846 ) ) ;
#10297 = CARTESIAN_POINT ( 'NONE',  ( -44.06622103062156270, 211.0902445701382533, 4.530955311639240257 ) ) ;
#10299 = EDGE_CURVE ( 'NONE', #33635, #17895, #36290, .T. ) ;
#10298 = CARTESIAN_POINT ( 'NONE',  ( -63.85788769728821279, 216.4690446883607535, 1.857196546604031662 ) ) ;
#10300 = DIRECTION ( 'NONE',  ( 0.000000000000000000, 0.000000000000000000, 1.000000000000000000 ) ) ;
#10301 = CARTESIAN_POINT ( 'NONE',  ( -10.38983282724226065, 218.0043899860427530, -3.786144536302608277 ) ) ;
#10302 = CARTESIAN_POINT ( 'NONE',  ( -2.908627838312453306, 41.27731371789855075, 15.53471296425188797 ) ) ;
#10303 = CARTESIAN_POINT ( 'NONE',  ( -47.42336230271184405, 217.4189793300686233, 4.149950860017807663 ) ) ;
#10304 = VECTOR ( 'NONE', #30574, 1000.000000000000000 ) ;
#10305 = CARTESIAN_POINT ( 'NONE',  ( 27.00000000000031619, -3.464101615137567869, -7.912499999999997868 ) ) ;
#10306 = CARTESIAN_POINT ( 'NONE',  ( -0.1745138560725500443, 65.61018628210145209, 12.50000000000000355 ) ) ;
#10307 = CARTESIAN_POINT ( 'NONE',  ( -15.50000000000000533, 31.11018628210143433, -0.1745138560725808530 ) ) ;
#10308 = CARTESIAN_POINT ( 'NONE',  ( 10.56230152254410903, 3.464101615137757051, -1.837500000000043876 ) ) ;
#10309 = DIRECTION ( 'NONE',  ( 0.08715574274765150453, 0.000000000000000000, 0.9961946980917461003 ) ) ;
#10310 = ORIENTED_EDGE ( 'NONE', *, *, #32309, .F. ) ;
#10311 = CARTESIAN_POINT ( 'NONE',  ( -13.23911966647218463, 30.24768628210144783, 8.632099005475506459 ) ) ;
#10312 = CARTESIAN_POINT ( 'NONE',  ( -27.24356964374999279, 198.0406250006145399, 15.72908226750539384 ) ) ;
#10313 = DIRECTION ( 'NONE',  ( 0.000000000000000000, 0.000000000000000000, -1.000000000000000000 ) ) ;
#10314 = CARTESIAN_POINT ( 'NONE',  ( 37.09921826190632999, -3.464101615137494594, 165.1726272931442452 ) ) ;
#10315 = CARTESIAN_POINT ( 'NONE',  ( -39.90997103062156270, 215.5714017266979852, 3.350049139982118618 ) ) ;
#10316 = CARTESIAN_POINT ( 'NONE',  ( 13.56230152254410370, 5.196152422706630247, -7.612499998771005139 ) ) ;
#10317 = CARTESIAN_POINT ( 'NONE',  ( 25.09912511996950713, 0.000000000000000000, 165.6954939908422944 ) ) ;
#10318 = CARTESIAN_POINT ( 'NONE',  ( 18.12178482187500350, 247.2343750006145342, 4.985214923628407568 ) ) ;
#10319 = CARTESIAN_POINT ( 'NONE',  ( -5.233372021372612259, 124.6523137178985650, 8.152565276336593669 ) ) ;
#10320 = CARTESIAN_POINT ( 'NONE',  ( 15.24356964374999990, 243.9718750006145456, -3.323476615752268604 ) ) ;
#10321 = PRESENTATION_LAYER_ASSIGNMENT (  '', '', ( #26656 ) ) ;
#10322 = ORIENTED_EDGE ( 'NONE', *, *, #21252, .T. ) ;
#10323 =( BOUNDED_CURVE ( )  B_SPLINE_CURVE ( 2, ( #10925, #22500, #19667, #16812, #28354, #14513, #5786, #3505, #23604 ),
 .UNSPECIFIED., .F., .F. ) 
 B_SPLINE_CURVE_WITH_KNOTS ( ( 3, 2, 2, 2, 3 ),
 ( 0.07608695652173913526, 0.07971014492753622505, 0.08695652173913043237, 0.09420289855072463969, 0.09782608695652174335 ),
 .UNSPECIFIED. ) 
 CURVE ( )  GEOMETRIC_REPRESENTATION_ITEM ( )  RATIONAL_B_SPLINE_CURVE ( ( 0.9330127018922192983, 0.9330127018922194093, 1.000000000000000000, 0.8660254037844387076, 1.000000000000000000, 0.8660254037844387076, 1.000000000000000000, 0.9330127018922194093, 0.9330127018922194093 ) ) 
 REPRESENTATION_ITEM ( '' )  );
#10324 = CARTESIAN_POINT ( 'NONE',  ( 13.56230152254411792, -5.196152422706638241, -7.125000000000075495 ) ) ;
#10325 = EDGE_CURVE ( 'NONE', #21823, #14348, #30432, .T. ) ;
#10326 = CARTESIAN_POINT ( 'NONE',  ( -42.59364919042334918, 252.0388376121882175, 0.5000000000000000000 ) ) ;
#10327 = CARTESIAN_POINT ( 'NONE',  ( -7.228626920338836470, 136.7273137178985678, -10.49813415416005213 ) ) ;
#10328 = CARTESIAN_POINT ( 'NONE',  ( 16.56230152254410726, -7.209453229046475009, -6.778124999385522820 ) ) ;
#10329 = CARTESIAN_POINT ( 'NONE',  ( 24.79520095057666396, 0.000000000000000000, 165.0162730863461604 ) ) ;
#10330 = CYLINDRICAL_SURFACE ( 'NONE', #32926, 27.00000000000000355 ) ;
#10331 = CARTESIAN_POINT ( 'NONE',  ( 5.727106289114498080E-15, 197.8625000000000114, 31.17691453623979214 ) ) ;
#10332 = ORIENTED_EDGE ( 'NONE', *, *, #13410, .T. ) ;
#10333 = CARTESIAN_POINT ( 'NONE',  ( -4.944772684328673229, 29.38518628210144712, 11.48171059495397728 ) ) ;
#10334 = VERTEX_POINT ( 'NONE', #19266 ) ;
#10335 = VERTEX_POINT ( 'NONE', #9777 ) ;
#10336 = CARTESIAN_POINT ( 'NONE',  ( 26.99999999999999645, -3.464101615137751278, -4.256249998770931242 ) ) ;
#10337 = CARTESIAN_POINT ( 'NONE',  ( 20.99999999999999645, 6.646953231504538984, -0.2531249993854407521 ) ) ;
#10338 = CARTESIAN_POINT ( 'NONE',  ( -27.00000000000000355, 199.1750000012290513, -15.58845726811989429 ) ) ;
#10339 = CARTESIAN_POINT ( 'NONE',  ( 33.77726345172796840, 5.196152422706631135, 161.6236498024106822 ) ) ;
#10340 = CARTESIAN_POINT ( 'NONE',  ( 18.12178482187499640, 4.985214923628404904, -7.865624999385478766 ) ) ;
#10341 = CARTESIAN_POINT ( 'NONE',  ( 8.962234695871762469, 80.56018628210145494, -8.715434833791931624 ) ) ;
#10342 = CARTESIAN_POINT ( 'NONE',  ( 13.04141134922778988, 10.22731371789853405, -8.927990412390371944 ) ) ;
#10343 = CARTESIAN_POINT ( 'NONE',  ( -47.00000000000000711, 244.5000000000000000, 2.500000000000001776 ) ) ;
#10344 = FACE_OUTER_BOUND ( 'NONE', #30664, .T. ) ;
#10345 = CARTESIAN_POINT ( 'NONE',  ( -59.69419563604517265, 205.4999999999999716, 0.1155267958017633378 ) ) ;
#10346 = CARTESIAN_POINT ( 'NONE',  ( 37.11555996377816058, 3.464101615137755275, 165.3594138002608247 ) ) ;
#10347 = CARTESIAN_POINT ( 'NONE',  ( 0.1745138560722779009, 123.7898137178985678, 12.50000000000000355 ) ) ;
#10348 = CARTESIAN_POINT ( 'NONE',  ( -44.06622103062156981, 211.6261429550005744, 6.530955311639227823 ) ) ;
#10349 = CARTESIAN_POINT ( 'NONE',  ( -59.30580436395490551, 218.5000000000000000, 0.1155267958017064944 ) ) ;
#10350 = ITEM_DEFINED_TRANSFORMATION ( 'NONE', 'NONE', #34757,  #17215 ) ;
#10351 = VECTOR ( 'NONE', #2464, 1000.000000000000000 ) ;
#10352 = CARTESIAN_POINT ( 'NONE',  ( 18.12178482187500350, -4.985214923628407568, -2.878124999385472726 ) ) ;
#10353 = CARTESIAN_POINT ( 'NONE',  ( -27.24356964375000345, 196.2031250006145342, 0.000000000000000000 ) ) ;
#10354 = CARTESIAN_POINT ( 'NONE',  ( 2.908627838312458636, 91.87731371789854506, -15.53471296425188442 ) ) ;
#10355 = CARTESIAN_POINT ( 'NONE',  ( -43.86086230271183695, 213.1499508600178387, -5.686928522499747451 ) ) ;
#10356 = EDGE_CURVE ( 'NONE', #17848, #28808, #27394, .T. ) ;
#10357 = EDGE_LOOP ( 'NONE', ( #31713, #31910, #5647, #27351 ) ) ;
#10358 = CARTESIAN_POINT ( 'NONE',  ( 34.23483110115314787, -5.196152422706629359, 166.8536719673923017 ) ) ;
#10359 = CARTESIAN_POINT ( 'NONE',  ( -12.50000000000000355, 123.1101862821014663, -0.1745138560725492671 ) ) ;
#10360 = CARTESIAN_POINT ( 'NONE',  ( -15.50000000000000533, 77.11018628210145209, -0.1745138560725808530 ) ) ;
#10361 = CARTESIAN_POINT ( 'NONE',  ( 20.99999999999998579, 247.6937500012290059, -5.999999999999997335 ) ) ;
#10362 = CARTESIAN_POINT ( 'NONE',  ( 37.21031035046954116, 7.646167579472024665E-16, 163.6477674281124450 ) ) ;
#10363 = CARTESIAN_POINT ( 'NONE',  ( -15.53471296425195369, 86.02268628210144641, 2.908627838312118019 ) ) ;
#10364 = CARTESIAN_POINT ( 'NONE',  ( -59.50372103062156981, 216.5309553116392181, -1.626142955000564383 ) ) ;
#10365 = CARTESIAN_POINT ( 'NONE',  ( 10.31873187879411269, 3.604726614523236616, -4.228124999385536320 ) ) ;
#10366 = CARTESIAN_POINT ( 'NONE',  ( 6.840914352312096547, 34.56018628210144783, -6.594114490232313663 ) ) ;
#10367 = CARTESIAN_POINT ( 'NONE',  ( 20.99999999999999645, 6.928203230275506996, -2.756249998770956111 ) ) ;
#10368 = CARTESIAN_POINT ( 'NONE',  ( -42.48288769728823411, 201.5309553116392181, -2.393094931466246855 ) ) ;
#10369 = CARTESIAN_POINT ( 'NONE',  ( 0.000000000000000000, 148.0000000000000000, 0.000000000000000000 ) ) ;
#10370 = CARTESIAN_POINT ( 'NONE',  ( -10.49813415415989581, 50.37268628210145494, -7.228626920339068285 ) ) ;
#10371 = CARTESIAN_POINT ( 'NONE',  ( 2.999999999999997335, 244.5000000000000000, 1.000000000000000000 ) ) ;
#10372 = CARTESIAN_POINT ( 'NONE',  ( 25.01079625726091749, 203.5081962293401148, -3.000000000000000000 ) ) ;
#10374 = CARTESIAN_POINT ( 'NONE',  ( 19.68408634441912142, -5.407089921784861808, -1.396874999385538940 ) ) ;
#10373 = CARTESIAN_POINT ( 'NONE',  ( 9.534712964251941258, 35.42268628210144499, -1.715153634034235708 ) ) ;
#10375 = DIRECTION ( 'NONE',  ( -0.000000000000000000, -1.000000000000000000, -0.000000000000000000 ) ) ;
#10376 = VERTEX_POINT ( 'NONE', #30438 ) ;
#10377 = CARTESIAN_POINT ( 'NONE',  ( 18.00000000000000355, -5.196152422706632912, -1.725000000000004308 ) ) ;
#10378 = CARTESIAN_POINT ( 'NONE',  ( 27.81522707900330715, 5.407089921784862696, 163.7168658290902101 ) ) ;
#10379 = CARTESIAN_POINT ( 'NONE',  ( 27.69224003142016954, -5.196152422706638241, 160.9137933187836609 ) ) ;
#10380 = CARTESIAN_POINT ( 'NONE',  ( 15.00000000000000178, 246.4375000000000000, 3.464101615137757051 ) ) ;
#10381 = DIRECTION ( 'NONE',  ( 0.000000000000000000, -1.000000000000000000, 0.000000000000000000 ) ) ;
#10382 = CARTESIAN_POINT ( 'NONE',  ( 6.932735513424201024, 83.25231371789857349, -10.69584247140429412 ) ) ;
#10383 = CARTESIAN_POINT ( 'NONE',  ( 10.49813415415989581, 91.77268628210144641, 7.228626920339069173 ) ) ;
#10384 = ORIENTED_EDGE ( 'NONE', *, *, #3104, .T. ) ;
#10385 = VERTEX_POINT ( 'NONE', #18705 ) ;
#10386 = CARTESIAN_POINT ( 'NONE',  ( 5.727106289114498080E-15, 197.5250000012290457, 31.17691453623979214 ) ) ;
#10387 = CARTESIAN_POINT ( 'NONE',  ( 15.00000000000000355, 7.347880794884112834E-16, -8.000000000000000000 ) ) ;
#10388 = CARTESIAN_POINT ( 'NONE',  ( 0.1745138560722461762, 50.18981371789855217, 15.50000000000000533 ) ) ;
#10389 = CARTESIAN_POINT ( 'NONE',  ( 26.75643035624999655, 7.049594010296217766E-16, -5.428124999385497418 ) ) ;
#10390 = CARTESIAN_POINT ( 'NONE',  ( 26.75643035624999655, 245.5843750006145285, -7.049594010296217766E-16 ) ) ;
#10391 = CARTESIAN_POINT ( 'NONE',  ( -58.11830436395491262, 209.8844732041982297, 4.499999999999996447 ) ) ;
#10392 = FACE_OUTER_BOUND ( 'NONE', #20693, .T. ) ;
#10393 = CARTESIAN_POINT ( 'NONE',  ( -9.465287035748106703, 43.00231371789853796, 2.064181346179061460 ) ) ;
#10394 = EDGE_CURVE ( 'NONE', #113, #15950, #4414, .T. ) ;
#10395 = CARTESIAN_POINT ( 'NONE',  ( 16.56230152254411081, -7.209453229046475009, -7.678124999385514293 ) ) ;
#10396 = EDGE_CURVE ( 'NONE', #27950, #7860, #4457, .T. ) ;
#10397 = SHAPE_REPRESENTATION ( 'rivet 1', ( #17215 ), #19008 ) ;
#10398 = CARTESIAN_POINT ( 'NONE',  ( 5.529263428287300108, 95.32731371789854791, 7.954856959092309943 ) ) ;
#10399 = CARTESIAN_POINT ( 'NONE',  ( -13.62178482187498396, 198.5843750006145569, 23.59362340125808188 ) ) ;
#10400 = CARTESIAN_POINT ( 'NONE',  ( -12.50000000000000355, 24.88981371789854435, 0.1745138560722786503 ) ) ;
#10401 = EDGE_CURVE ( 'NONE', #34897, #34009, #10712, .T. ) ;
#10402 = CARTESIAN_POINT ( 'NONE',  ( 2.660918448318279950, 88.89768628210146062, -12.46528703574805697 ) ) ;
#10403 = CARTESIAN_POINT ( 'NONE',  ( 19.56230152254411436, -5.196152422706629359, -9.187499998771025744 ) ) ;
#10404 = EDGE_CURVE ( 'NONE', #15602, #1464, #18478, .T. ) ;
#10405 = CARTESIAN_POINT ( 'NONE',  ( 0.000000000000000000, 210.0000000000000284, 0.000000000000000000 ) ) ;
#10406 = CARTESIAN_POINT ( 'NONE',  ( 37.01911243981686539, 7.646167579472015790E-16, 161.4623653091736628 ) ) ;
#10407 = CARTESIAN_POINT ( 'NONE',  ( 16.56230152254411436, 7.209453229046482114, -9.759374999385554972 ) ) ;
#10408 = CIRCLE ( 'NONE', #28551, 5.000000000000000888 ) ;
#10409 = CARTESIAN_POINT ( 'NONE',  ( 22.80587116629411781, -3.604726614523238837, -5.859374999385517313 ) ) ;
#10410 = CARTESIAN_POINT ( 'NONE',  ( -26.99999999999999645, 195.6500000012290457, 15.58845726811991561 ) ) ;
#10411 = CARTESIAN_POINT ( 'NONE',  ( -0.1745138560725182642, 93.21018628210146062, 9.500000000000005329 ) ) ;
#10412 = CARTESIAN_POINT ( 'NONE',  ( 0.000000000000000000, 210.0000000000000284, -27.00000000000000000 ) ) ;
#10413 = CARTESIAN_POINT ( 'NONE',  ( -6.932735513423968321, 124.5476862821014663, -10.69584247140445221 ) ) ;
#10414 = CARTESIAN_POINT ( 'NONE',  ( -11.00000000000001421, 143.0000000000000000, 1.001863997985030341 ) ) ;
#10415 = CARTESIAN_POINT ( 'NONE',  ( 15.24356964374999990, 239.8468750006145171, 0.000000000000000000 ) ) ;
#10416 = VERTEX_POINT ( 'NONE', #24144 ) ;
#10417 = CARTESIAN_POINT ( 'NONE',  ( 24.83115269446006934, 3.604726614523236616, 165.4272033993090076 ) ) ;
#10418 = CARTESIAN_POINT ( 'NONE',  ( 18.12178482187500350, -4.985214923628407568, -5.465624999385465088 ) ) ;
#10419 = CARTESIAN_POINT ( 'NONE',  ( 27.24356964374999279, 198.3218750006145399, -15.72908226750539207 ) ) ;
#10420 = CARTESIAN_POINT ( 'NONE',  ( 31.39005398230442268, -6.928203230275514990, 168.7588604462623039 ) ) ;
#10421 = CARTESIAN_POINT ( 'NONE',  ( 30.68409246604844043, -6.928203230275514990, 160.6896833917191714 ) ) ;
#10422 = CARTESIAN_POINT ( 'NONE',  ( 26.75643035624999655, 242.0218750006145285, -3.323476615752271712 ) ) ;
#10423 = DIRECTION ( 'NONE',  ( 0.08715574274765150453, 0.000000000000000000, 0.9961946980917461003 ) ) ;
#10424 = CARTESIAN_POINT ( 'NONE',  ( 7.228626920338837358, 141.3273137178985337, 10.49813415416005036 ) ) ;
#10425 = CARTESIAN_POINT ( 'NONE',  ( 13.62178482187501416, 195.0593750006145513, 23.59362340125806767 ) ) ;
#10427 = ORIENTED_EDGE ( 'NONE', *, *, #34596, .F. ) ;
#10426 = ORIENTED_EDGE ( 'NONE', *, *, #15759, .F. ) ;
#10428 = VECTOR ( 'NONE', #12836, 1000.000000000000000 ) ;
#10429 = CARTESIAN_POINT ( 'NONE',  ( 15.24356964374999990, 245.2468750006145228, 0.000000000000000000 ) ) ;
#10430 = DIRECTION ( 'NONE',  ( 1.000000000000000000, 6.123233995736766036E-17, -0.000000000000000000 ) ) ;
#10431 = CARTESIAN_POINT ( 'NONE',  ( 15.24356964375000167, -3.323476615752272600, -2.803124999385491645 ) ) ;
#10432 = CARTESIAN_POINT ( 'NONE',  ( -8.632099005475794229, 106.2523137178985451, 13.23911966647199812 ) ) ;
#10433 = DIRECTION ( 'NONE',  ( 0.8083506638593009885, 0.5887012860850803220, -0.000000000000000000 ) ) ;
#10434 = CARTESIAN_POINT ( 'NONE',  ( 21.00000000000000000, 6.928203230275506996, -9.056249998770928400 ) ) ;
#10435 = CARTESIAN_POINT ( 'NONE',  ( 13.44051670066911441, -5.407089921784865361, -9.121874999385520155 ) ) ;
#10436 = ORIENTED_EDGE ( 'NONE', *, *, #31965, .F. ) ;
#10437 = CARTESIAN_POINT ( 'NONE',  ( -27.24356964375000345, 194.8531250006145115, 0.000000000000000000 ) ) ;
#10438 = CARTESIAN_POINT ( 'NONE',  ( 8.962234695871762469, 126.5601862821014691, -8.715434833791931624 ) ) ;
#10439 = CARTESIAN_POINT ( 'NONE',  ( 10.31873187879410736, -3.604726614523240613, -1.453124999385536187 ) ) ;
#10440 = CARTESIAN_POINT ( 'NONE',  ( 33.79318086914889818, 5.407089921784862696, 160.4082625921878673 ) ) ;
#10441 = CARTESIAN_POINT ( 'NONE',  ( -58.90252896937851546, 205.6499508600178103, -7.303452534266820173 ) ) ;
#10442 = CARTESIAN_POINT ( 'NONE',  ( 15.24356964375000167, 245.7343750006144774, 3.323476615752272600 ) ) ;
#10443 = DIRECTION ( 'NONE',  ( 1.000000000000000000, 0.000000000000000000, 0.000000000000000000 ) ) ;
#10444 = CARTESIAN_POINT ( 'NONE',  ( -31.19419563604517265, 205.4999999999999716, 0.1155267958017633378 ) ) ;
#10445 = CARTESIAN_POINT ( 'NONE',  ( 16.56230152254411081, 6.928203230275506996, -2.249999998771013310 ) ) ;
#10446 = ORIENTED_EDGE ( 'NONE', *, *, #26971, .T. ) ;
#10447 = LINE ( 'NONE', #36592, #10081 ) ;
#10448 = CARTESIAN_POINT ( 'NONE',  ( 22.56230152254502741, -3.464101615137234358, -8.812500000000046185 ) ) ;
#10449 = CARTESIAN_POINT ( 'NONE',  ( 11.08355503943142750, 126.5601862821014834, -10.83675517735155225 ) ) ;
#10450 = CARTESIAN_POINT ( 'NONE',  ( -0.1745138560725500443, 19.61018628210144144, 12.50000000000000355 ) ) ;
#10451 = VECTOR ( 'NONE', #1986, 1000.000000000000000 ) ;
#10452 = CARTESIAN_POINT ( 'NONE',  ( 19.56230152254412502, -5.196152422706635576, -8.400000000000073186 ) ) ;
#10453 = VERTEX_POINT ( 'NONE', #12764 ) ;
#10454 = LINE ( 'NONE', #4767, #34862 ) ;
#10455 = CARTESIAN_POINT ( 'NONE',  ( 5.529263428287477744, 89.47268628210143504, -7.954856959092191815 ) ) ;
#10456 = CARTESIAN_POINT ( 'NONE',  ( -6.594114490232462877, 134.1398137178985621, 6.840914352311949109 ) ) ;
#10457 = CARTESIAN_POINT ( 'NONE',  ( -13.62178482187500528, 195.6781250006145569, -23.59362340125807123 ) ) ;
#10458 = DIRECTION ( 'NONE',  ( 0.9961946980917462113, 0.000000000000000000, -0.08715574274765118534 ) ) ;
#10459 = CARTESIAN_POINT ( 'NONE',  ( -1.926257025242585782E-15, 198.3968750006145285, -31.45816453501075927 ) ) ;
#10460 = DIRECTION ( 'NONE',  ( 0.1219804832088915297, 0.9925324990730154395, 0.000000000000000000 ) ) ;
#10461 = DIRECTION ( 'NONE',  ( 0.000000000000000000, 0.000000000000000000, 1.000000000000000000 ) ) ;
#10462 = CARTESIAN_POINT ( 'NONE',  ( -5.529263428287297444, 53.92731371789854222, -7.954856959092311719 ) ) ;
#10463 = DIRECTION ( 'NONE',  ( 1.000000000000000000, 0.000000000000000000, 0.000000000000000000 ) ) ;
#10464 = EDGE_LOOP ( 'NONE', ( #10725, #31213, #2875, #18973 ) ) ;
#10465 = AXIS2_PLACEMENT_3D ( 'NONE', #23912, #769, #18420 ) ;
#10466 = CARTESIAN_POINT ( 'NONE',  ( 21.00000000000000000, 240.9437500012290911, -6.928203230275506996 ) ) ;
#10467 = CARTESIAN_POINT ( 'NONE',  ( -6.932735513424201912, 60.25231371789854506, 10.69584247140429412 ) ) ;
#10468 = CARTESIAN_POINT ( 'NONE',  ( 19.68408634441912142, -5.407089921784861808, -7.246874999385532590 ) ) ;
#10469 = CARTESIAN_POINT ( 'NONE',  ( 27.24356964375000345, 198.6781250006145569, -3.336375036156643733E-15 ) ) ;
#10470 = CARTESIAN_POINT ( 'NONE',  ( 21.00000000000000000, -6.646953231504538984, -7.790624999385473259 ) ) ;
#10471 = CARTESIAN_POINT ( 'NONE',  ( -4.622313124798826500, 23.16481371789855359, 11.61527771782809637 ) ) ;
#10472 = ORIENTED_EDGE ( 'NONE', *, *, #11690, .T. ) ;
#10473 = CARTESIAN_POINT ( 'NONE',  ( 23.87821517812499650, 4.985214923628404904, -7.940624999385470062 ) ) ;
#10474 = CARTESIAN_POINT ( 'NONE',  ( 12.50000000000000355, 17.31018628210144428, 0.1745138560725507937 ) ) ;
#10475 = CARTESIAN_POINT ( 'NONE',  ( 25.18576762276457259, -3.604726614523244610, 169.4804705771697968 ) ) ;
#10476 = CARTESIAN_POINT ( 'NONE',  ( -55.14211230271182274, 203.5309553116391612, 1.857196546604092280 ) ) ;
#10477 = CARTESIAN_POINT ( 'NONE',  ( -7.234628195640316228, 196.3075961894323598, -27.00000000000000000 ) ) ;
#10478 = CARTESIAN_POINT ( 'NONE',  ( -0.1745138560722763466, 73.18981371789855928, -12.50000000000000355 ) ) ;
#10479 = CARTESIAN_POINT ( 'NONE',  ( -67.41294563604516554, 213.2096571498974527, -3.378800118222469617 ) ) ;
#10480 =( BOUNDED_CURVE ( )  B_SPLINE_CURVE ( 2, ( #2096, #33754, #13476, #4567, #27875, #22205, #36587, #13674, #16887 ),
 .UNSPECIFIED., .F., .F. ) 
 B_SPLINE_CURVE_WITH_KNOTS ( ( 3, 2, 2, 2, 3 ),
 ( 0.3958333333333333703, 0.4027777777777777901, 0.4166666666666666852, 0.4305555555555555802, 0.4375000000000000000 ),
 .UNSPECIFIED. ) 
 CURVE ( )  GEOMETRIC_REPRESENTATION_ITEM ( )  RATIONAL_B_SPLINE_CURVE ( ( 0.9330127018922194093, 0.9330127018922196314, 1.000000000000000000, 0.8660254037844387076, 1.000000000000000000, 0.8660254037844387076, 1.000000000000000000, 0.9330127018922194093, 0.9330127018922194093 ) ) 
 REPRESENTATION_ITEM ( '' )  );
#10481 = CARTESIAN_POINT ( 'NONE',  ( -61.28497103062156981, 204.4285982733020148, -3.350049139982115509 ) ) ;
#10482 = CARTESIAN_POINT ( 'NONE',  ( -66.61573224020317241, 223.4103818930302054, 7.500000000000000000 ) ) ;
#10483 = CARTESIAN_POINT ( 'NONE',  ( 26.99999999999999645, 7.347880794884117764E-16, -2.868749998770958598 ) ) ;
#10484 = CARTESIAN_POINT ( 'NONE',  ( -5.770363421894122880, 41.56481371789855217, 14.38691631536194393 ) ) ;
#10485 = CARTESIAN_POINT ( 'NONE',  ( -43.86086230271183695, 214.1499508600178387, -7.418979330068641964 ) ) ;
#10486 = PRESENTATION_LAYER_ASSIGNMENT (  '', '', ( #7467 ) ) ;
#10487 = DIRECTION ( 'NONE',  ( 1.000000000000000000, 0.000000000000000000, 0.000000000000000000 ) ) ;
#10488 = CARTESIAN_POINT ( 'NONE',  ( 11.61527771782819940, 71.93518628210145494, -4.622313124798573369 ) ) ;
#10489 = CARTESIAN_POINT ( 'NONE',  ( 3.257655550457285720, 15.29768628210142722, -15.46528703574804986 ) ) ;
#10490 = CARTESIAN_POINT ( 'NONE',  ( 10.56230152254410548, 3.464101615137757051, -1.387500000000016165 ) ) ;
#10491 = CARTESIAN_POINT ( 'NONE',  ( -7.234628195640328663, 197.5049038117967086, 26.99999999999999289 ) ) ;
#10492 = ORIENTED_EDGE ( 'NONE', *, *, #23719, .F. ) ;
#10493 = CARTESIAN_POINT ( 'NONE',  ( 15.46528703574804986, 26.79768628210144144, 3.257655550457285720 ) ) ;
#10494 = CARTESIAN_POINT ( 'NONE',  ( -27.24356964374999279, 195.7906250006145399, 15.72908226750539384 ) ) ;
#10495 = CARTESIAN_POINT ( 'NONE',  ( -13.62178482187498396, 197.2343750006145626, 23.59362340125808188 ) ) ;
#10496 = CARTESIAN_POINT ( 'NONE',  ( -12.50000000000000355, 6.489813717898557321, 0.1745138560722785670 ) ) ;
#10497 = CARTESIAN_POINT ( 'NONE',  ( 37.22995187613445012, 7.347880794884117764E-16, 166.6669193415062580 ) ) ;
#10498 = CARTESIAN_POINT ( 'NONE',  ( 27.00000000000000355, 195.7250000000000227, -3.306546357697854128E-15 ) ) ;
#10499 = CARTESIAN_POINT ( 'NONE',  ( 10.69584247140445221, 7.247686282101428290, -6.932735513423970097 ) ) ;
#10500 =( BOUNDED_SURFACE ( )  B_SPLINE_SURFACE ( 1, 2, ( 
 ( #8567, #3245, #20888, #17290, #29012, #22978, #14439, #8753, #5710, #26740, #34706, #32429, #8938, #6083, #23, #580, #20134, #214, #17668, #25993, #18045, #17856, #6474, #11589, #29204, #14626, #14819, #20515, #32053, #28831, #6281, #32241, #23725, #26363, #31680, #2866, #398, #17479, #31865, #23534, #3056, #26177, #11964, #23165, #35080, #9130, #20696, #29398, #3432, #15000, #3624, #11779, #26552, #35263, #9318, #29587, #15192, #774, #15382, #15570, #32997, #32621, #15761, #6846, #21083, #12342, #13098, #30348, #27504, #18805, #4372, #15951, #1525, #21637, #9507, #3806, #7415, #27311, #6658, #24653, #18986, #36204, #35835, #7232, #1341, #12912, #18233, #7049, #12721, #24102, #24476, #10248, #21824, #35647, #33376, #26932, #962, #30543, #9876, #33189, #4560, #3996, #4188, #16135, #27126, #12538, #27687, #23916, #1151, #29775, #9693, #21269, #32807, #35457, #21457, #18617, #36022, #18423, #29967, #24291, #30159, #10062, #22382, #33931, #25023, #22566, #4748, #4927, #7972, #22010, #5117, #33748, #10437, #1714, #2458 ),
 ( #8164, #19738, #10994, #36391, #30725, #34302, #16696, #33564, #16882, #8346, #31276, #25216, #34113, #28244, #2274, #7601, #19547, #2091, #13471, #13851, #14031, #25582, #36580, #37135, #16321, #27868, #19917, #36767, #5303, #11180, #30906, #31095, #28418, #16509, #1901, #31457, #22753, #28056, #19176, #10621, #22200, #7788, #13284, #5480, #17063, #24839, #19366, #13666, #10810, #25398, #36948, #6427, #26136, #28602, #9274, #3015, #14584, #14216, #8893, #26508, #22940, #34666, #2639, #20094, #14398, #11368, #32386, #2826, #539, #170, #11737, #5668, #6237, #25766, #5858, #23307, #31640, #23678, #23488, #12105, #17248, #34853, #20283, #20471, #32010, #6041, #34485, #11921, #357, #29352, #17627, #37318, #8528, #29157, #11548, #25955, #3199, #37497, #31823, #14776, #28789, #26320, #35039, #20846, #9086, #35225, #23122, #8711, #17436, #28974, #20655, #32202, #17812, #3392, #14961, #24056, #33332, #4145, #6613, #30303, #3953, #6800, #36162, #1484, #725, #18001, #18761, #4328, #21224, #12297, #21036, #27083, #21410, #18375, #23871 ) ),
 .UNSPECIFIED., .F., .F., .F. ) 
 B_SPLINE_SURFACE_WITH_KNOTS ( ( 2, 2 ),
 ( 3, 2, 2, 2, 2, 2, 2, 2, 2, 2, 2, 2, 2, 2, 2, 2, 2, 2, 2, 2, 2, 2, 2, 2, 2, 2, 2, 2, 2, 2, 2, 2, 2, 2, 2, 2, 2, 2, 2, 2, 2, 2, 2, 2, 2, 2, 2, 2, 2, 2, 2, 2, 2, 2, 2, 2, 2, 2, 2, 2, 2, 2, 2, 2, 2, 2, 2, 3 ),
 ( 0.000000000000000000, 1.000000000000000000 ),
 ( 0.000000000000000000, 0.01388888888888888812, 0.02777777777777777624, 0.04166666666666666435, 0.05555555555555555247, 0.06944444444444444753, 0.08333333333333332871, 0.09722222222222222376, 0.1111111111111111049, 0.1250000000000000000, 0.1388888888888888951, 0.1527777777777777901, 0.1666666666666666574, 0.1805555555555555525, 0.1944444444444444475, 0.2083333333333333426, 0.2222222222222222099, 0.2361111111111111049, 0.2500000000000000000, 0.2638888888888888951, 0.2777777777777777901, 0.2916666666666666852, 0.3055555555555555802, 0.3194444444444444198, 0.3333333333333333148, 0.3472222222222222099, 0.3611111111111111049, 0.3750000000000000000, 0.3888888888888888951, 0.4027777777777777901, 0.4166666666666666852, 0.4305555555555555802, 0.4444444444444444198, 0.4583333333333333148, 0.4722222222222222099, 0.4861111111111111049, 0.5000000000000000000, 0.5138888888888888395, 0.5277777777777777901, 0.5416666666666666297, 0.5555555555555555802, 0.5694444444444444198, 0.5833333333333333703, 0.5972222222222222099, 0.6111111111111111605, 0.6250000000000000000, 0.6388888888888888395, 0.6527777777777777901, 0.6666666666666666297, 0.6805555555555555802, 0.6944444444444444198, 0.7083333333333333703, 0.7222222222222222099, 0.7361111111111111605, 0.7500000000000000000, 0.7638888888888888395, 0.7777777777777777901, 0.7916666666666666297, 0.8055555555555555802, 0.8194444444444444198, 0.8333333333333333703, 0.8472222222222222099, 0.8611111111111111605, 0.8750000000000000000, 0.8888888888888888395, 0.9027777777777777901, 0.9166666666666666297, 0.9258785558287927486 ),
 .UNSPECIFIED. ) 
 GEOMETRIC_REPRESENTATION_ITEM ( )  RATIONAL_B_SPLINE_SURFACE ( (
 ( 1.000000000000000000, 0.8660254037844387076, 1.000000000000000000, 0.8660254037844387076, 1.000000000000000000, 0.8660254037844387076, 1.000000000000000000, 0.8660254037844387076, 1.000000000000000000, 0.8660254037844387076, 1.000000000000000000, 0.8660254037844387076, 1.000000000000000000, 0.8660254037844387076, 1.000000000000000000, 0.8660254037844387076, 1.000000000000000000, 0.8660254037844387076, 1.000000000000000000, 0.8660254037844387076, 1.000000000000000000, 0.8660254037844387076, 1.000000000000000000, 0.8660254037844387076, 1.000000000000000000, 0.8660254037844387076, 1.000000000000000000, 0.8660254037844387076, 1.000000000000000000, 0.8660254037844387076, 1.000000000000000000, 0.8660254037844387076, 1.000000000000000000, 0.8660254037844387076, 1.000000000000000000, 0.8660254037844387076, 1.000000000000000000, 0.8660254037844387076, 1.000000000000000000, 0.8660254037844387076, 1.000000000000000000, 0.8660254037844387076, 1.000000000000000000, 0.8660254037844387076, 1.000000000000000000, 0.8660254037844387076, 1.000000000000000000, 0.8660254037844387076, 1.000000000000000000, 0.8660254037844387076, 1.000000000000000000, 0.8660254037844387076, 1.000000000000000000, 0.8660254037844387076, 1.000000000000000000, 0.8660254037844387076, 1.000000000000000000, 0.8660254037844387076, 1.000000000000000000, 0.8660254037844387076, 1.000000000000000000, 0.8660254037844387076, 1.000000000000000000, 0.8660254037844387076, 1.000000000000000000, 0.8660254037844387076, 1.000000000000000000, 0.8660254037844387076, 1.000000000000000000, 0.8660254037844387076, 1.000000000000000000, 0.8660254037844387076, 1.000000000000000000, 0.8660254037844387076, 1.000000000000000000, 0.8660254037844387076, 1.000000000000000000, 0.8660254037844387076, 1.000000000000000000, 0.8660254037844387076, 1.000000000000000000, 0.8660254037844387076, 1.000000000000000000, 0.8660254037844387076, 1.000000000000000000, 0.8660254037844387076, 1.000000000000000000, 0.8660254037844387076, 1.000000000000000000, 0.8660254037844387076, 1.000000000000000000, 0.8660254037844387076, 1.000000000000000000, 0.8660254037844387076, 1.000000000000000000, 0.8660254037844387076, 1.000000000000000000, 0.8660254037844387076, 1.000000000000000000, 0.8660254037844387076, 1.000000000000000000, 0.8660254037844387076, 1.000000000000000000, 0.8660254037844387076, 1.000000000000000000, 0.8660254037844387076, 1.000000000000000000, 0.8660254037844387076, 1.000000000000000000, 0.8660254037844387076, 1.000000000000000000, 0.8660254037844387076, 1.000000000000000000, 0.8660254037844387076, 1.000000000000000000, 0.8660254037844387076, 1.000000000000000000, 0.8660254037844387076, 1.000000000000000000, 0.8660254037844387076, 1.000000000000000000, 0.8660254037844387076, 1.000000000000000000, 0.8660254037844387076, 1.000000000000000000, 0.8660254037844387076, 1.000000000000000000, 0.8660254037844387076, 1.000000000000000000, 0.8660254037844387076, 1.000000000000000000, 0.8660254037844387076, 1.000000000000000000, 0.9111405425767590271, 0.9401542252352144136),
 ( 1.000000000000000000, 0.8660254037844387076, 1.000000000000000000, 0.8660254037844387076, 1.000000000000000000, 0.8660254037844387076, 1.000000000000000000, 0.8660254037844387076, 1.000000000000000000, 0.8660254037844387076, 1.000000000000000000, 0.8660254037844387076, 1.000000000000000000, 0.8660254037844387076, 1.000000000000000000, 0.8660254037844387076, 1.000000000000000000, 0.8660254037844387076, 1.000000000000000000, 0.8660254037844387076, 1.000000000000000000, 0.8660254037844387076, 1.000000000000000000, 0.8660254037844387076, 1.000000000000000000, 0.8660254037844387076, 1.000000000000000000, 0.8660254037844387076, 1.000000000000000000, 0.8660254037844387076, 1.000000000000000000, 0.8660254037844387076, 1.000000000000000000, 0.8660254037844387076, 1.000000000000000000, 0.8660254037844387076, 1.000000000000000000, 0.8660254037844387076, 1.000000000000000000, 0.8660254037844387076, 1.000000000000000000, 0.8660254037844387076, 1.000000000000000000, 0.8660254037844387076, 1.000000000000000000, 0.8660254037844387076, 1.000000000000000000, 0.8660254037844387076, 1.000000000000000000, 0.8660254037844387076, 1.000000000000000000, 0.8660254037844387076, 1.000000000000000000, 0.8660254037844387076, 1.000000000000000000, 0.8660254037844387076, 1.000000000000000000, 0.8660254037844387076, 1.000000000000000000, 0.8660254037844387076, 1.000000000000000000, 0.8660254037844387076, 1.000000000000000000, 0.8660254037844387076, 1.000000000000000000, 0.8660254037844387076, 1.000000000000000000, 0.8660254037844387076, 1.000000000000000000, 0.8660254037844387076, 1.000000000000000000, 0.8660254037844387076, 1.000000000000000000, 0.8660254037844387076, 1.000000000000000000, 0.8660254037844387076, 1.000000000000000000, 0.8660254037844387076, 1.000000000000000000, 0.8660254037844387076, 1.000000000000000000, 0.8660254037844387076, 1.000000000000000000, 0.8660254037844387076, 1.000000000000000000, 0.8660254037844387076, 1.000000000000000000, 0.8660254037844387076, 1.000000000000000000, 0.8660254037844387076, 1.000000000000000000, 0.8660254037844387076, 1.000000000000000000, 0.8660254037844387076, 1.000000000000000000, 0.8660254037844387076, 1.000000000000000000, 0.8660254037844387076, 1.000000000000000000, 0.8660254037844387076, 1.000000000000000000, 0.8660254037844387076, 1.000000000000000000, 0.8660254037844387076, 1.000000000000000000, 0.8660254037844387076, 1.000000000000000000, 0.8660254037844387076, 1.000000000000000000, 0.8660254037844387076, 1.000000000000000000, 0.8660254037844387076, 1.000000000000000000, 0.8660254037844387076, 1.000000000000000000, 0.8660254037844387076, 1.000000000000000000, 0.8660254037844387076, 1.000000000000000000, 0.8660254037844387076, 1.000000000000000000, 0.8660254037844387076, 1.000000000000000000, 0.8660254037844387076, 1.000000000000000000, 0.8660254037844387076, 1.000000000000000000, 0.8660254037844387076, 1.000000000000000000, 0.8660254037844387076, 1.000000000000000000, 0.8660254037844387076, 1.000000000000000000, 0.9111405425767590271, 0.9401542252352144136) ) ) 
 REPRESENTATION_ITEM ( '' )  SURFACE ( )  );
#10501 = VECTOR ( 'NONE', #18451, 1000.000000000000000 ) ;
#10502 = CARTESIAN_POINT ( 'NONE',  ( 18.12178482187500350, 248.5843750006145285, 4.985214923628407568 ) ) ;
#10503 = CARTESIAN_POINT ( 'NONE',  ( -5.529263428287297444, 109.1273137178985451, -7.954856959092311719 ) ) ;
#10504 = CARTESIAN_POINT ( 'NONE',  ( 18.12178482187499640, 243.9343750006145513, -4.985214923628404904 ) ) ;
#10505 = EDGE_LOOP ( 'NONE', ( #26264, #20176, #6313, #35665 ) ) ;
#10506 = CARTESIAN_POINT ( 'NONE',  ( 3.253724281355069334E-15, 199.8875000000000455, -27.00000000000000000 ) ) ;
#10507 = CARTESIAN_POINT ( 'NONE',  ( 0.1745138560722779009, 142.1898137178985735, 12.50000000000000355 ) ) ;
#10508 = CARTESIAN_POINT ( 'NONE',  ( 10.31873187879411091, -3.604726614523240613, -9.553124999385522287 ) ) ;
#10509 = CARTESIAN_POINT ( 'NONE',  ( 24.68080903822037087, -3.604726614523240613, 163.7087675451007271 ) ) ;
#10510 = CARTESIAN_POINT ( 'NONE',  ( 24.93243976185750554, 0.000000000000000000, 163.7902716295174912 ) ) ;
#10511 = CARTESIAN_POINT ( 'NONE',  ( -13.50000000000000533, 197.2250000000000227, -23.38268590217984411 ) ) ;
#10512 = EDGE_CURVE ( 'NONE', #30621, #18936, #21310, .T. ) ;
#10513 = ORIENTED_EDGE ( 'NONE', *, *, #29163, .T. ) ;
#10514 = CARTESIAN_POINT ( 'NONE',  ( -12.46528703574805874, 31.39768628210144641, -2.660918448318280838 ) ) ;
#10515 = ORIENTED_EDGE ( 'NONE', *, *, #20929, .T. ) ;
#10516 = ORIENTED_EDGE ( 'NONE', *, *, #6720, .F. ) ;
#10517 = CARTESIAN_POINT ( 'NONE',  ( 18.00000000000000000, 5.196152422706630247, -4.068749998770964993 ) ) ;
#10518 = CARTESIAN_POINT ( 'NONE',  ( 26.75643035624999655, -3.323476615752267271, -0.4031249993854607028 ) ) ;
#10519 = CARTESIAN_POINT ( 'NONE',  ( 1.255007937094097924E-14, 199.1000000012290627, -27.00000000000000000 ) ) ;
#10521 = CARTESIAN_POINT ( 'NONE',  ( 1.069080835302379631E-14, 195.6124999999999829, 27.00000000000000000 ) ) ;
#10520 = PRESENTATION_LAYER_ASSIGNMENT (  '', '', ( #16564 ) ) ;
#10522 = CARTESIAN_POINT ( 'NONE',  ( 23.87821517812500005, 249.4468750006145115, 4.985214923628404016 ) ) ;
#10523 = CARTESIAN_POINT ( 'NONE',  ( 11.48171059495397728, 73.08518628210144641, 4.944772684328674117 ) ) ;
#10524 = CARTESIAN_POINT ( 'NONE',  ( 13.04141134922759804, 137.7726862821014606, 8.927990412390657937 ) ) ;
#10525 = VECTOR ( 'NONE', #33268, 1000.000000000000000 ) ;
#10526 = CARTESIAN_POINT ( 'NONE',  ( -62.26711230271183695, 216.4690446883607535, -1.857196546604089393 ) ) ;
#10527 = ADVANCED_FACE ( 'NONE', ( #35873 ), #33042, .F. ) ;
#10528 = CARTESIAN_POINT ( 'NONE',  ( 7.136082524517427750, 215.1989690533051771, -3.001545256184917854 ) ) ;
#10529 = CARTESIAN_POINT ( 'NONE',  ( -57.91294563604517265, 213.2096571498974527, -3.378800118222469617 ) ) ;
#10530 = DIRECTION ( 'NONE',  ( 0.000000000000000000, 0.000000000000000000, 1.000000000000000000 ) ) ;
#10531 = CARTESIAN_POINT ( 'NONE',  ( 24.94551312337678084, -3.464101615137757051, 163.9397008354555965 ) ) ;
#10532 = CARTESIAN_POINT ( 'NONE',  ( 6.932735513424201024, 129.2523137178985451, -10.69584247140429412 ) ) ;
#10533 = CARTESIAN_POINT ( 'NONE',  ( -45.84747103062156981, 213.3500491399821328, -5.571401726697985168 ) ) ;
#10534 = CARTESIAN_POINT ( 'NONE',  ( -62.67038769728824121, 207.6069050685337913, 8.469044688360781947 ) ) ;
#10535 = CARTESIAN_POINT ( 'NONE',  ( 15.24356964375000167, -3.323476615752272600, -2.015624999385490668 ) ) ;
#10536 = CARTESIAN_POINT ( 'NONE',  ( -27.24356964374999990, 197.0656250006145171, -15.72908226750537786 ) ) ;
#10537 = CARTESIAN_POINT ( 'NONE',  ( -14.38691631536193860, 99.06481371789857349, -5.770363421894132649 ) ) ;
#10538 = CARTESIAN_POINT ( 'NONE',  ( -49.00669563604516554, 209.8844732041982013, -6.500000000000000888 ) ) ;
#10539 = EDGE_CURVE ( 'NONE', #19993, #28398, #30083, .T. ) ;
#10540 = ORIENTED_EDGE ( 'NONE', *, *, #2412, .F. ) ;
#10541 = CARTESIAN_POINT ( 'NONE',  ( 30.86058284511243599, 6.928203230275514990, 162.7069776553549616 ) ) ;
#10542 = CARTESIAN_POINT ( 'NONE',  ( 10.69584247140445221, 117.6476862821014464, -6.932735513423970097 ) ) ;
#10543 = CARTESIAN_POINT ( 'NONE',  ( -15.53471296425195369, 67.62268628210145494, 2.908627838312118019 ) ) ;
#10544 = CARTESIAN_POINT ( 'NONE',  ( -98.52697526167152375, 63.53212182842481326, -3.000000000000000000 ) ) ;
#10545 = CARTESIAN_POINT ( 'NONE',  ( 24.79029844004710625, 0.000000000000000000, 164.9602371345785343 ) ) ;
#10546 = VECTOR ( 'NONE', #23007, 1000.000000000000000 ) ;
#10547 = CARTESIAN_POINT ( 'NONE',  ( 13.04141134922759804, 91.77268628210144641, 8.927990412390657937 ) ) ;
#10548 =( BOUNDED_CURVE ( )  B_SPLINE_CURVE ( 2, ( #15259, #24166, #29274, #6728, #9760, #29841, #3313 ),
 .UNSPECIFIED., .F., .F. ) 
 B_SPLINE_CURVE_WITH_KNOTS ( ( 3, 2, 2, 3 ),
 ( 0.06521739130434869858, 0.07246376811594300305, 0.07971014492753727976, 0.08695652173913158423 ),
 .UNSPECIFIED. ) 
 CURVE ( )  GEOMETRIC_REPRESENTATION_ITEM ( )  RATIONAL_B_SPLINE_CURVE ( ( 0.9999999999999837907, 0.8660254037844549169, 1.000000000000000000, 0.8660254037844387076, 1.000000000000000000, 0.8660254037844173913, 1.000000000000021316 ) ) 
 REPRESENTATION_ITEM ( '' )  );
#10549 = CARTESIAN_POINT ( 'NONE',  ( -60.09747103062156981, 213.3500491399821328, -5.571401726697985168 ) ) ;
#10550 = VECTOR ( 'NONE', #10708, 1000.000000000000000 ) ;
#10551 = CARTESIAN_POINT ( 'NONE',  ( 22.80587116629410716, 7.646167579472015790E-16, -5.765624999385543958 ) ) ;
#10552 = CARTESIAN_POINT ( 'NONE',  ( 9.465287035748067623, 45.19768628210142225, 2.064181346179272847 ) ) ;
#10553 = CARTESIAN_POINT ( 'NONE',  ( -59.50372103062156981, 216.5309553116391612, -1.626142955000564383 ) ) ;
#10554 = CARTESIAN_POINT ( 'NONE',  ( 27.73146011565660984, -5.196152422706638241, 161.3620809329249539 ) ) ;
#10555 = CARTESIAN_POINT ( 'NONE',  ( 7.228626920339068285, 61.87268628210145494, -10.49813415415989581 ) ) ;
#10556 = CARTESIAN_POINT ( 'NONE',  ( -26.99999999999998934, 199.1375000000000171, 15.58845726811991561 ) ) ;
#10557 = CARTESIAN_POINT ( 'NONE',  ( -29.00000000000002487, 215.7563705986615901, 5.555555555555559799 ) ) ;
#10559 = CARTESIAN_POINT ( 'NONE',  ( 19.68408634441911076, 5.407089921784862696, -1.246874999385527705 ) ) ;
#10558 = CARTESIAN_POINT ( 'NONE',  ( 5.233372021372432847, 18.74768628210143362, 8.152565276336710909 ) ) ;
#10560 = DIRECTION ( 'NONE',  ( 0.000000000000000000, -0.000000000000000000, -1.000000000000000000 ) ) ;
#10561 = VERTEX_POINT ( 'NONE', #24405 ) ;
#10562 = CARTESIAN_POINT ( 'NONE',  ( 24.00000000000000000, -5.196152422706629359, -2.099999999999990763 ) ) ;
#10563 = CARTESIAN_POINT ( 'NONE',  ( 27.86752052465190133, -5.407089921784865361, 164.3145826479452296 ) ) ;
#10564 = CARTESIAN_POINT ( 'NONE',  ( 27.67916667000801212, 5.196152422706636465, 160.7643641140699344 ) ) ;
#10565 = CARTESIAN_POINT ( 'NONE',  ( 15.00000000000000178, 244.6375000000000171, 3.464101615137757051 ) ) ;
#10566 = CARTESIAN_POINT ( 'NONE',  ( 29.51984228635672380, 5.908847293266075162, 159.3365288790247121 ) ) ;
#10567 = CARTESIAN_POINT ( 'NONE',  ( 2.660918448318002838, 86.70231371789854791, 12.46528703574811558 ) ) ;
#10568 = CARTESIAN_POINT ( 'NONE',  ( -4.622313124798576922, 88.03518628210144925, -11.61527771782819762 ) ) ;
#10569 = VERTEX_POINT ( 'NONE', #27244 ) ;
#10570 = EDGE_LOOP ( 'NONE', ( #29914, #32232, #28673, #10009, #18077, #26451 ) ) ;
#10571 = CARTESIAN_POINT ( 'NONE',  ( 5.727106289114498080E-15, 198.8750000012290400, 31.17691453623979214 ) ) ;
#10572 = CARTESIAN_POINT ( 'NONE',  ( 26.99999999999999645, 7.347880794884117764E-16, -3.824999999999994849 ) ) ;
#10573 = ADVANCED_FACE ( 'NONE', ( #18548 ), #21758, .F. ) ;
#10574 = CARTESIAN_POINT ( 'NONE',  ( -8.632099005475794229, 51.05231371789854222, 13.23911966647199812 ) ) ;
#10575 = CARTESIAN_POINT ( 'NONE',  ( 15.24356964374999990, 0.000000000000000000, -7.903124999385474858 ) ) ;
#10576 = CARTESIAN_POINT ( 'NONE',  ( 21.00000000000000000, 242.9968750006145228, -6.646953231504538984 ) ) ;
#10577 = CARTESIAN_POINT ( 'NONE',  ( -61.28497103062156981, 206.1606490808709111, -2.350049139982163027 ) ) ;
#10578 = DIRECTION ( 'NONE',  ( 0.000000000000000000, 0.000000000000000000, -1.000000000000000000 ) ) ;
#10579 = CARTESIAN_POINT ( 'NONE',  ( 6.594114490232462877, 46.73981371789855643, -6.840914352311949109 ) ) ;
#10580 = EDGE_CURVE ( 'NONE', #3896, #33538, #9239, .T. ) ;
#10581 = CARTESIAN_POINT ( 'NONE',  ( 13.44051670066911619, -5.407089921784859143, -7.265624999385544847 ) ) ;
#10582 = CARTESIAN_POINT ( 'NONE',  ( -8.152565276336593669, 90.15231371789855075, -5.233372021372610483 ) ) ;
#10583 = CARTESIAN_POINT ( 'NONE',  ( 5.778771075727756162E-15, 199.0718750006145399, 31.45816453501075927 ) ) ;
#10584 = CARTESIAN_POINT ( 'NONE',  ( -12.46528703574811558, 15.40231371789854542, 2.660918448318003726 ) ) ;
#10585 = CARTESIAN_POINT ( 'NONE',  ( -4.944772684328673229, 56.98518628210144499, 11.48171059495397728 ) ) ;
#10586 = CARTESIAN_POINT ( 'NONE',  ( 10.56230152254410903, 0.000000000000000000, -7.987499998771019349 ) ) ;
#10587 = DIRECTION ( 'NONE',  ( 1.000000000000000000, 0.000000000000000000, 0.000000000000000000 ) ) ;
#10588 = CARTESIAN_POINT ( 'NONE',  ( 30.76988640036921652, 7.209453229046475009, 161.6703125482654286 ) ) ;
#10589 = CARTESIAN_POINT ( 'NONE',  ( 26.99999999999999645, -3.464101615137751278, -1.106249998770961307 ) ) ;
#10590 = CARTESIAN_POINT ( 'NONE',  ( 10.31873187879410736, -3.604726614523244610, -6.909374999385495819 ) ) ;
#10591 = DIRECTION ( 'NONE',  ( 0.000000000000000000, 0.000000000000000000, -1.000000000000000000 ) ) ;
#10592 = CARTESIAN_POINT ( 'NONE',  ( -7.954856959092191815, 87.17268628210142367, -5.529263428287477744 ) ) ;
#10593 = CARTESIAN_POINT ( 'NONE',  ( 22.56230152254395094, 3.464101615137851642, -6.037500000000023626 ) ) ;
#10594 = CARTESIAN_POINT ( 'NONE',  ( 4.944772684328679446, 116.7851862821014635, -11.48171059495397373 ) ) ;
#10595 = DIRECTION ( 'NONE',  ( 1.000000000000000000, 0.000000000000000000, 0.000000000000000000 ) ) ;
#10596 = CARTESIAN_POINT ( 'NONE',  ( -49.64999999999999858, 244.5000000000000000, 0.4999999999999995559 ) ) ;
#10597 = ORIENTED_EDGE ( 'NONE', *, *, #25981, .T. ) ;
#10598 = CARTESIAN_POINT ( 'NONE',  ( 34.07262396933355575, 5.407089921784857367, 163.6023118429445162 ) ) ;
#10599 = CARTESIAN_POINT ( 'NONE',  ( 15.24356964374999990, 0.000000000000000000, -5.990624999385463667 ) ) ;
#10600 = CARTESIAN_POINT ( 'NONE',  ( -1.926257025242585782E-15, 197.4968750006145513, -31.45816453501076637 ) ) ;
#10601 = DIRECTION ( 'NONE',  ( 1.000000000000000000, 0.000000000000000000, 0.000000000000000000 ) ) ;
#10602 = CARTESIAN_POINT ( 'NONE',  ( 34.31653960987195973, 5.196152422706637353, 167.7876044956290116 ) ) ;
#10603 = CARTESIAN_POINT ( 'NONE',  ( 0.000000000000000000, 200.0000000000000000, -27.00000000000000355 ) ) ;
#10604 = CARTESIAN_POINT ( 'NONE',  ( 18.12178482187500350, 243.1843750006145513, 4.985214923628407568 ) ) ;
#10605 = CARTESIAN_POINT ( 'NONE',  ( 1.120210788295102201E-13, 195.3875000000000455, -27.00000000000000711 ) ) ;
#10606 = VECTOR ( 'NONE', #9489, 1000.000000000000000 ) ;
#10607 = CARTESIAN_POINT ( 'NONE',  ( -12.50000000000000355, 144.4898137178985564, 0.1745138560722786503 ) ) ;
#10608 = CARTESIAN_POINT ( 'NONE',  ( 13.62178482187501416, 195.9593750006145569, 23.59362340125806767 ) ) ;
#10610 = ORIENTED_EDGE ( 'NONE', *, *, #8355, .T. ) ;
#10609 = VERTEX_POINT ( 'NONE', #1267 ) ;
#10611 = ADVANCED_BREP_SHAPE_REPRESENTATION ( '', ( #21232, #17215 ), #34722 ) ;
#10612 = CARTESIAN_POINT ( 'NONE',  ( 23.87821517812499650, 245.5468750006145058, -4.985214923628404904 ) ) ;
#10613 = CARTESIAN_POINT ( 'NONE',  ( -10.69584247140429412, 7.352313717898545598, -6.932735513424201024 ) ) ;
#10614 = ADVANCED_FACE ( 'NONE', ( #7535 ), #32927, .T. ) ;
#10615 = CARTESIAN_POINT ( 'NONE',  ( 26.75643035624999655, 7.049594010296217766E-16, -3.065624999385479832 ) ) ;
#10616 = CARTESIAN_POINT ( 'NONE',  ( -11.08355503943118592, 118.0398137178985536, -10.83675517735179383 ) ) ;
#10617 = CARTESIAN_POINT ( 'NONE',  ( 24.00000000000000000, 244.2999999999999829, 5.196152422706629359 ) ) ;
#10618 = CARTESIAN_POINT ( 'NONE',  ( 18.00000000000000000, 5.196152422706630247, -10.36874999877096570 ) ) ;
#10619 = CARTESIAN_POINT ( 'NONE',  ( 13.44051670066911086, 5.407089921784862696, -8.371874999385548577 ) ) ;
#10620 = ORIENTED_EDGE ( 'NONE', *, *, #14204, .T. ) ;
#10621 = CARTESIAN_POINT ( 'NONE',  ( -1.909035429704832693E-15, 198.2000000012290286, -31.17691453623979214 ) ) ;
#10622 = CARTESIAN_POINT ( 'NONE',  ( 10.49813415415989581, 119.3726862821014549, 7.228626920339068285 ) ) ;
#10623 = CARTESIAN_POINT ( 'NONE',  ( 19.68408634441910721, -5.407089921784855591, -0.4406249993855471114 ) ) ;
#10624 = CARTESIAN_POINT ( 'NONE',  ( -48.21502896937850124, 217.3034525342667962, -4.350049139982195001 ) ) ;
#10625 = CARTESIAN_POINT ( 'NONE',  ( 18.12178482187499640, 243.3718750006145228, -4.985214923628404904 ) ) ;
#10626 = CARTESIAN_POINT ( 'NONE',  ( 25.08932009880328096, 0.000000000000000000, 165.5834220860826349 ) ) ;
#10627 = CARTESIAN_POINT ( 'NONE',  ( -34.95461230271183695, 208.6787018382582346, -4.469044688360757966 ) ) ;
#10628 = CARTESIAN_POINT ( 'NONE',  ( 37.37702719191401002, 7.347880794884125653E-16, 168.3479978933117422 ) ) ;
#10629 = CARTESIAN_POINT ( 'NONE',  ( 10.56230152254410903, 0.000000000000000000, -0.7874999987710074034 ) ) ;
#10630 = ORIENTED_EDGE ( 'NONE', *, *, #26990, .F. ) ;
#10631 = VECTOR ( 'NONE', #10707, 1000.000000000000000 ) ;
#10632 = CARTESIAN_POINT ( 'NONE',  ( 1.069080835302379631E-14, 195.2750000012290457, 27.00000000000000000 ) ) ;
#10633 = CARTESIAN_POINT ( 'NONE',  ( -27.00000000000000355, 199.5500000000000114, 0.000000000000000000 ) ) ;
#10634 = CARTESIAN_POINT ( 'NONE',  ( 14.25334919248782661, 119.0851862821014606, 6.092822981423971385 ) ) ;
#10635 = CARTESIAN_POINT ( 'NONE',  ( 22.60769515458670753, 242.7236538117967086, -6.000000000000011546 ) ) ;
#10636 = CARTESIAN_POINT ( 'NONE',  ( -2.311890736173176641, 14.72268628210143859, -12.53471296425194836 ) ) ;
#10637 = CARTESIAN_POINT ( 'NONE',  ( 10.31873187879411091, 0.000000000000000000, -0.1406249993855246405 ) ) ;
#10638 = ORIENTED_EDGE ( 'NONE', *, *, #2939, .T. ) ;
#10639 = CARTESIAN_POINT ( 'NONE',  ( -13.99999999999999467, 143.0000000000000000, -1.543483589373963192E-13 ) ) ;
#10640 = CARTESIAN_POINT ( 'NONE',  ( -7.954856959092191815, 87.17268628210142367, -5.529263428287477744 ) ) ;
#10641 = PRESENTATION_STYLE_ASSIGNMENT (( #2297 ) ) ;
#10642 = CARTESIAN_POINT ( 'NONE',  ( 9.465287035748106703, 130.4023137178985792, -2.064181346179063237 ) ) ;
#10643 = CARTESIAN_POINT ( 'NONE',  ( -27.24356964374999635, 196.6906250006145456, 15.72908226750539384 ) ) ;
#10644 = CARTESIAN_POINT ( 'NONE',  ( 21.00000000000001066, 247.0187500012290513, 5.999999999999998224 ) ) ;
#10645 = CARTESIAN_POINT ( 'NONE',  ( -27.24356964374999635, 198.0968750006145456, 15.72908226750539384 ) ) ;
#10646 = EDGE_CURVE ( 'NONE', #5744, #12855, #9269, .T. ) ;
#10647 = CARTESIAN_POINT ( 'NONE',  ( -47.00000000000000711, 244.5000000000000000, -5.000000000000001776 ) ) ;
#10648 = CARTESIAN_POINT ( 'NONE',  ( 26.99999999999999645, 243.8875000000000171, 3.464101615137751278 ) ) ;
#10649 = CARTESIAN_POINT ( 'NONE',  ( 2.064181346179061460, 59.10231371789854649, 9.465287035748106703 ) ) ;
#10650 = CARTESIAN_POINT ( 'NONE',  ( 26.99999999999999645, -3.464101615137751278, -8.812499999999992895 ) ) ;
#10651 = ORIENTED_EDGE ( 'NONE', *, *, #19461, .F. ) ;
#10652 = CARTESIAN_POINT ( 'NONE',  ( 18.00000000000000000, 240.5312500012290400, -5.196152422706630247 ) ) ;
#10653 = CARTESIAN_POINT ( 'NONE',  ( 12.50000000000000355, 66.28981371789855359, -0.1745138560722771515 ) ) ;
#10654 = CARTESIAN_POINT ( 'NONE',  ( 22.80587116629411781, -3.604726614523238837, -6.759374999385539873 ) ) ;
#10655 = CARTESIAN_POINT ( 'NONE',  ( 27.24356964375000700, 198.1906250006145740, 15.72908226750537075 ) ) ;
#10656 = CARTESIAN_POINT ( 'NONE',  ( 23.87821517812500005, -4.985214923628404016, -7.303124999385484983 ) ) ;
#10657 = CARTESIAN_POINT ( 'NONE',  ( 11.48171059495408208, 28.91481371789854293, -4.944772684328420986 ) ) ;
#10658 = ADVANCED_FACE ( 'NONE', ( #36322 ), #27426, .T. ) ;
#10659 =( GEOMETRIC_REPRESENTATION_CONTEXT ( 3 ) GLOBAL_UNCERTAINTY_ASSIGNED_CONTEXT ( ( #25255 ) ) GLOBAL_UNIT_ASSIGNED_CONTEXT ( ( #1171, #9895, #33018 ) ) REPRESENTATION_CONTEXT ( 'NONE', 'WORKASPACE' ) );
#10660 = VERTEX_POINT ( 'NONE', #13032 ) ;
#10661 = CARTESIAN_POINT ( 'NONE',  ( 13.44051670066911086, 5.407089921784862696, -1.621874999385541916 ) ) ;
#10662 = DIRECTION ( 'NONE',  ( 0.000000000000000000, -1.000000000000000000, 0.000000000000000000 ) ) ;
#10663 = CARTESIAN_POINT ( 'NONE',  ( 34.49914238540488043, 5.407089921784862696, 168.4774396467310282 ) ) ;
#10664 = CARTESIAN_POINT ( 'NONE',  ( -45.24627896937850835, 203.4690446883607535, -1.626142955000504209 ) ) ;
#10665 =( LENGTH_UNIT ( ) NAMED_UNIT ( * ) SI_UNIT ( .MILLI., .METRE. ) );
#10666 = CARTESIAN_POINT ( 'NONE',  ( -3.253724281355068545E-15, 196.2874999999999659, -27.00000000000000000 ) ) ;
#10667 = CARTESIAN_POINT ( 'NONE',  ( -4.622313124798826500, 59.96481371789855075, 11.61527771782809637 ) ) ;
#10668 = CARTESIAN_POINT ( 'NONE',  ( -40.30580436395490551, 214.5000000000000284, 0.1155267958017899832 ) ) ;
#10669 = CARTESIAN_POINT ( 'NONE',  ( -53.76413769728823411, 213.1499508600178672, 5.686928522499718142 ) ) ;
#10670 = CARTESIAN_POINT ( 'NONE',  ( 26.99999999999999645, 7.347880794884117764E-16, -6.975000000000008527 ) ) ;
#10671 = CARTESIAN_POINT ( 'NONE',  ( 30.81155773992399460, -6.928203230275506996, 162.1466181389027099 ) ) ;
#10672 = CARTESIAN_POINT ( 'NONE',  ( 10.83675517735179206, 46.73981371789855643, -11.08355503943118769 ) ) ;
#10673 = CARTESIAN_POINT ( 'NONE',  ( -36.93377896937849414, 207.8379586601372750, 8.530955311639258909 ) ) ;
#10674 = CARTESIAN_POINT ( 'NONE',  ( -6.932735513423968321, 23.34768628210144570, -10.69584247140445221 ) ) ;
#10675 = LINE ( 'NONE', #11565, #25498 ) ;
#10676 = CARTESIAN_POINT ( 'NONE',  ( 0.1745138560725515708, 61.01018628210145067, -12.50000000000000355 ) ) ;
#10677 = CARTESIAN_POINT ( 'NONE',  ( -6.092822981423970496, 10.98518628210143433, 14.25334919248782661 ) ) ;
#10678 = CARTESIAN_POINT ( 'NONE',  ( 10.56230152254410903, 0.000000000000000000, -1.800000000000051559 ) ) ;
#10679 = CARTESIAN_POINT ( 'NONE',  ( 18.00000000000000000, 244.1312500012290343, -5.196152422706630247 ) ) ;
#10680 = ORIENTED_EDGE ( 'NONE', *, *, #2732, .T. ) ;
#10681 = CARTESIAN_POINT ( 'NONE',  ( 2.908627838312118019, 37.72268628210143504, 15.53471296425195369 ) ) ;
#10682 = CARTESIAN_POINT ( 'NONE',  ( 27.24356964375000700, 195.4906250006145001, 15.72908226750537075 ) ) ;
#10683 = CARTESIAN_POINT ( 'NONE',  ( 13.62178482187501416, 197.7593750006145399, 23.59362340125806767 ) ) ;
#10684 = DIRECTION ( 'NONE',  ( -0.000000000000000000, -1.000000000000000000, -0.000000000000000000 ) ) ;
#10685 = CARTESIAN_POINT ( 'NONE',  ( 21.00000000000000000, 210.0000000000000284, 8.000000000000000000 ) ) ;
#10686 = CARTESIAN_POINT ( 'NONE',  ( 23.99999999999999645, 5.196152422706631135, -5.493749998770947052 ) ) ;
#10687 = CARTESIAN_POINT ( 'NONE',  ( 11.48171059495397728, 8.685186282101437172, 4.944772684328674117 ) ) ;
#10688 = CARTESIAN_POINT ( 'NONE',  ( 15.24356964374999990, 247.6093750006145342, 0.000000000000000000 ) ) ;
#10689 = CARTESIAN_POINT ( 'NONE',  ( -9.534712964251895073, 117.1773137178985706, -1.715153634034446428 ) ) ;
#10690 = CARTESIAN_POINT ( 'NONE',  ( 23.87821517812500005, 240.5593750006145228, 4.985214923628404016 ) ) ;
#10691 = ORIENTED_EDGE ( 'NONE', *, *, #5436, .T. ) ;
#10692 = CARTESIAN_POINT ( 'NONE',  ( -62.47247103062156981, 206.6499508600178672, 5.571401726697986057 ) ) ;
#10693 = SURFACE_STYLE_USAGE ( .BOTH. , #27759 ) ;
#10694 = AXIS2_PLACEMENT_3D ( 'NONE', #14970, #3213, #29740 ) ;
#10695 = CARTESIAN_POINT ( 'NONE',  ( 18.00000000000000000, 249.0812500012290513, -5.196152422706630247 ) ) ;
#10696 = CARTESIAN_POINT ( 'NONE',  ( -12.50000000000000355, 126.0898137178985650, 0.1745138560722786503 ) ) ;
#10697 = CARTESIAN_POINT ( 'NONE',  ( 16.56230152254411081, -7.209453229046475009, -9.028124999385500615 ) ) ;
#10698 = CARTESIAN_POINT ( 'NONE',  ( 36.97662401522738662, -3.604726614523235284, 160.9767203938538955 ) ) ;
#10699 = CARTESIAN_POINT ( 'NONE',  ( 26.99999999999999645, 240.8312500012290513, -7.347880794884117764E-16 ) ) ;
#10700 = CARTESIAN_POINT ( 'NONE',  ( -27.00000000000000355, 196.8500000000000227, 0.000000000000000000 ) ) ;
#10701 = ORIENTED_EDGE ( 'NONE', *, *, #28626, .F. ) ;
#10702 = CARTESIAN_POINT ( 'NONE',  ( -7.228626920339070061, 29.67268628210143788, 10.49813415415989404 ) ) ;
#10703 = VERTEX_POINT ( 'NONE', #19107 ) ;
#10704 = ORIENTED_EDGE ( 'NONE', *, *, #412, .T. ) ;
#10705 = CARTESIAN_POINT ( 'NONE',  ( 15.00000000000000000, 0.000000000000000000, -5.343749998770963572 ) ) ;
#10706 = CARTESIAN_POINT ( 'NONE',  ( 23.87821517812500005, -4.985214923628404016, -3.140624999385472016 ) ) ;
#10707 = DIRECTION ( 'NONE',  ( 0.000000000000000000, 1.000000000000000000, 0.000000000000000000 ) ) ;
#10708 = DIRECTION ( 'NONE',  ( -0.000000000000000000, 1.000000000000000000, -0.000000000000000000 ) ) ;
#10709 = CARTESIAN_POINT ( 'NONE',  ( 0.000000000000000000, 2.000000000000000000, -5.000000000000000000 ) ) ;
#10710 = CARTESIAN_POINT ( 'NONE',  ( 2.660918448318279950, 52.09768628210144215, -12.46528703574805697 ) ) ;
#10711 = CARTESIAN_POINT ( 'NONE',  ( -14.38691631536207183, 140.9351862821014549, 5.770363421893814682 ) ) ;
#10712 =( BOUNDED_CURVE ( )  B_SPLINE_CURVE ( 2, ( #18515, #13369, #24924, #10337, #13002, #27211, #36477, #10518, #36108, #10151, #35731, #22097, #33647, #24375, #32894, #7686, #30806, #21725, #4828, #16037, #16409, #27955, #13557, #33275, #1615, #12805, #13185, #30054, #9962, #27586, #35919, #24740, #7132, #21354, #6946, #21542, #33089, #13752, #25667, #22466, #11269, #37403, #8059, #30997, #34013, #34570, #8429, #14115, #16778, #28140, #36668, #28323, #8610, #28688, #37034, #7874, #17335, #16962, #5016, #20180, #31728, #2728, #19998, #25298, #19634, #22655, #10894, #5757, #16596, #2548, #37223, #25855, #31542, #19447, #11081, #31180, #5202, #36850, #33836, #2361, #10706, #13935, #19821, #25483, #28879, #14302, #34202, #2170, #2913, #28505, #8247, #25111, #22283, #31357, #5382, #22839, #34387, #5567, #11453, #17152, #23022, #14860, #11633, #625, #3287, #9171, #6129, #23389, #23765, #26594, #29441, #32661, #3477, #14669, #20739, #15046, #3100, #23207, #6702, #26219, #34755, #255, #17522, #31913, #12193, #35306, #8799, #29057, #32282, #9360, #11820, #20935, #20370, #32470, #21122, #20553, #23578, #26408, #34937, #5943, #6326, #8982, #35122, #18274, #26785, #29816, #35500, #15235, #6513, #29629, #14485, #3665, #17897, #9548, #816, #18088, #12387, #32097, #23957, #26039, #67, #17706, #29247, #441, #12006, #24514, #33415, #6893, #27541, #10290, #36063, #15994, #4600, #13138, #21862, #32846, #13323, #1002, #24694, #7454, #27352, #7268, #36246, #1382, #1569, #19029, #21676, #3851, #24883, #30389, #30009, #18844, #15611, #33230, #9916, #21499, #1757, #35686, #16178, #24332, #9739, #18468, #4039, #36430, #30584, #27728, #12954, #12577, #10473, #10106, #4411 ),
 .UNSPECIFIED., .F., .F. ) 
 B_SPLINE_CURVE_WITH_KNOTS ( ( 3, 2, 2, 2, 2, 2, 2, 2, 2, 2, 2, 2, 2, 2, 2, 2, 2, 2, 2, 2, 2, 2, 2, 2, 2, 2, 2, 2, 2, 2, 2, 2, 2, 2, 2, 2, 2, 2, 2, 2, 2, 2, 2, 2, 2, 2, 2, 2, 2, 2, 2, 2, 2, 2, 2, 2, 2, 2, 2, 2, 2, 2, 2, 2, 2, 2, 2, 2, 2, 2, 2, 2, 2, 2, 2, 2, 2, 2, 2, 2, 2, 2, 2, 2, 2, 2, 2, 2, 2, 2, 2, 2, 2, 2, 2, 2, 2, 2, 2, 2, 2, 2, 2, 2, 2, 3 ),
 ( 0.000000000000000000, 0.007246376811594202987, 0.01449275362318840597, 0.02173913043478260809, 0.02898550724637681195, 0.03623188405797101580, 0.04347826086956521618, 0.05072463768115942351, 0.05797101449275362389, 0.06521739130434782428, 0.07246376811594203160, 0.07971014492753622505, 0.08695652173913043237, 0.09420289855072463969, 0.1014492753623188470, 0.1086956521739130266, 0.1159420289855072478, 0.1231884057971014551, 0.1304347826086956486, 0.1376811594202898559, 0.1449275362318840632, 0.1521739130434782705, 0.1594202898550724501, 0.1666666666666666574, 0.1739130434782608647, 0.1811594202898550721, 0.1884057971014492794, 0.1956521739130435145, 0.2028985507246376940, 0.2101449275362318736, 0.2173913043478260532, 0.2246376811594202882, 0.2318840579710144956, 0.2391304347826087029, 0.2463768115942029102, 0.2536231884057971175, 0.2608695652173912971, 0.2681159420289855322, 0.2753623188405797118, 0.2826086956521738913, 0.2898550724637681264, 0.2971014492753623060, 0.3043478260869565410, 0.3115942028985507206, 0.3188405797101449002, 0.3260869565217391353, 0.3333333333333333148, 0.3405797101449275499, 0.3478260869565217295, 0.3550724637681159090, 0.3623188405797101441, 0.3695652173913043237, 0.3768115942028985588, 0.3840579710144927383, 0.3913043478260870289, 0.3985507246376811530, 0.4057971014492753881, 0.4130434782608696231, 0.4202898550724637472, 0.4275362318840579823, 0.4347826086956521063, 0.4420289855072463969, 0.4492753623188405765, 0.4565217391304347561, 0.4637681159420289911, 0.4710144927536232262, 0.4782608695652174058, 0.4855072463768115854, 0.4927536231884058204, 0.5000000000000000000, 0.5072463768115942351, 0.5144927536231883591, 0.5217391304347825942, 0.5289855072463768293, 0.5362318840579710644, 0.5434782608695651884, 0.5507246376811594235, 0.5579710144927536586, 0.5652173913043477826, 0.5724637681159420177, 0.5797101449275362528, 0.5869565217391304879, 0.5942028985507246119, 0.6014492753623188470, 0.6086956521739130821, 0.6159420289855072062, 0.6231884057971014412, 0.6304347826086956763, 0.6376811594202898004, 0.6449275362318840354, 0.6521739130434782705, 0.6594202898550725056, 0.6666666666666666297, 0.6739130434782608647, 0.6811594202898550998, 0.6884057971014492239, 0.6956521739130434590, 0.7028985507246376940, 0.7101449275362318181, 0.7173913043478260532, 0.7246376811594202882, 0.7318840579710144123, 0.7391304347826086474, 0.7463768115942028825, 0.7536231884057971175, 0.7592621468213750502 ),
 .UNSPECIFIED. ) 
 CURVE ( )  GEOMETRIC_REPRESENTATION_ITEM ( )  RATIONAL_B_SPLINE_CURVE ( ( 1.000000000000000000, 0.8660254037844387076, 1.000000000000000000, 0.8660254037844387076, 1.000000000000000000, 0.8660254037844387076, 1.000000000000000000, 0.8660254037844387076, 1.000000000000000000, 0.8660254037844387076, 1.000000000000000000, 0.8660254037844387076, 1.000000000000000000, 0.8660254037844387076, 1.000000000000000000, 0.8660254037844387076, 1.000000000000000000, 0.8660254037844387076, 1.000000000000000000, 0.8660254037844387076, 1.000000000000000000, 0.8660254037844387076, 1.000000000000000000, 0.8660254037844387076, 1.000000000000000000, 0.8660254037844387076, 1.000000000000000000, 0.8660254037844387076, 1.000000000000000000, 0.8660254037844387076, 1.000000000000000000, 0.8660254037844387076, 1.000000000000000000, 0.8660254037844387076, 1.000000000000000000, 0.8660254037844387076, 1.000000000000000000, 0.8660254037844387076, 1.000000000000000000, 0.8660254037844387076, 1.000000000000000000, 0.8660254037844387076, 1.000000000000000000, 0.8660254037844387076, 1.000000000000000000, 0.8660254037844387076, 1.000000000000000000, 0.8660254037844387076, 1.000000000000000000, 0.8660254037844387076, 1.000000000000000000, 0.8660254037844387076, 1.000000000000000000, 0.8660254037844387076, 1.000000000000000000, 0.8660254037844387076, 1.000000000000000000, 0.8660254037844387076, 1.000000000000000000, 0.8660254037844387076, 1.000000000000000000, 0.8660254037844387076, 1.000000000000000000, 0.8660254037844387076, 1.000000000000000000, 0.8660254037844387076, 1.000000000000000000, 0.8660254037844387076, 1.000000000000000000, 0.8660254037844387076, 1.000000000000000000, 0.8660254037844387076, 1.000000000000000000, 0.8660254037844387076, 1.000000000000000000, 0.8660254037844387076, 1.000000000000000000, 0.8660254037844387076, 1.000000000000000000, 0.8660254037844387076, 1.000000000000000000, 0.8660254037844387076, 1.000000000000000000, 0.8660254037844387076, 1.000000000000000000, 0.8660254037844387076, 1.000000000000000000, 0.8660254037844387076, 1.000000000000000000, 0.8660254037844387076, 1.000000000000000000, 0.8660254037844387076, 1.000000000000000000, 0.8660254037844387076, 1.000000000000000000, 0.8660254037844387076, 1.000000000000000000, 0.8660254037844387076, 1.000000000000000000, 0.8660254037844387076, 1.000000000000000000, 0.8660254037844387076, 1.000000000000000000, 0.8660254037844387076, 1.000000000000000000, 0.8660254037844387076, 1.000000000000000000, 0.8660254037844387076, 1.000000000000000000, 0.8660254037844387076, 1.000000000000000000, 0.8660254037844387076, 1.000000000000000000, 0.8660254037844387076, 1.000000000000000000, 0.8660254037844387076, 1.000000000000000000, 0.8660254037844387076, 1.000000000000000000, 0.8660254037844387076, 1.000000000000000000, 0.8660254037844387076, 1.000000000000000000, 0.8660254037844387076, 1.000000000000000000, 0.8660254037844387076, 1.000000000000000000, 0.8660254037844387076, 1.000000000000000000, 0.8660254037844387076, 1.000000000000000000, 0.8660254037844387076, 1.000000000000000000, 0.8660254037844387076, 1.000000000000000000, 0.8660254037844387076, 1.000000000000000000, 0.8660254037844387076, 1.000000000000000000, 0.8660254037844387076, 1.000000000000000000, 0.8660254037844387076, 1.000000000000000000, 0.8660254037844387076, 1.000000000000000000, 0.8660254037844387076, 1.000000000000000000, 0.8660254037844387076, 1.000000000000000000, 0.8660254037844387076, 1.000000000000000000, 0.8660254037844387076, 1.000000000000000000, 0.8660254037844387076, 1.000000000000000000, 0.8660254037844387076, 1.000000000000000000, 0.8660254037844387076, 1.000000000000000000, 0.8660254037844387076, 1.000000000000000000, 0.8660254037844387076, 1.000000000000000000, 0.8660254037844387076, 1.000000000000000000, 0.8660254037844387076, 1.000000000000000000, 0.8660254037844387076, 1.000000000000000000, 0.8660254037844387076, 1.000000000000000000, 0.8660254037844387076, 1.000000000000000000, 0.8660254037844387076, 1.000000000000000000, 0.8660254037844387076, 1.000000000000000000, 0.8660254037844387076, 1.000000000000000000, 0.8660254037844387076, 1.000000000000000000, 0.8660254037844387076, 1.000000000000000000, 0.8660254037844387076, 1.000000000000000000, 0.8660254037844387076, 1.000000000000000000, 0.8660254037844387076, 1.000000000000000000, 0.8660254037844387076, 1.000000000000000000, 0.8660254037844387076, 1.000000000000000000, 0.8660254037844387076, 1.000000000000000000, 0.8660254037844387076, 1.000000000000000000, 0.8660254037844387076, 1.000000000000000000, 0.8660254037844387076, 1.000000000000000000, 0.8660254037844387076, 1.000000000000000000, 0.8660254037844387076, 1.000000000000000000, 0.8660254037844387076, 1.000000000000000000, 0.8660254037844387076, 1.000000000000000000, 0.8957441496011320226, 0.9537471549767242429 ) ) 
 REPRESENTATION_ITEM ( '' )  );
#10713 = CARTESIAN_POINT ( 'NONE',  ( -58.70461230271182984, 208.1428034533958851, -6.469044688360754414 ) ) ;
#10714 = CARTESIAN_POINT ( 'NONE',  ( 14.59897497552647749, 216.4010250244744498, 0.7232488345312237943 ) ) ;
#10715 = CARTESIAN_POINT ( 'NONE',  ( -52.17336230271184405, 213.9548777149308023, 2.149950860017852960 ) ) ;
#10716 = AXIS2_PLACEMENT_3D ( 'NONE', #32870, #9194, #9005 ) ;
#10717 = CARTESIAN_POINT ( 'NONE',  ( 25.02395329184966144, -3.464101615137757051, 164.8362760637381541 ) ) ;
#10718 = CARTESIAN_POINT ( 'NONE',  ( -7.228626920338836470, 118.3273137178985621, -10.49813415416005213 ) ) ;
#10719 = CARTESIAN_POINT ( 'NONE',  ( -32.58705436395489841, 205.3262412349647263, -4.842901733360204020 ) ) ;
#10720 = CARTESIAN_POINT ( 'NONE',  ( -56.73288769728824832, 201.5309553116392181, -2.393094931466246855 ) ) ;
#10721 = CARTESIAN_POINT ( 'NONE',  ( 15.24356964374999990, 3.323476615752268604, -2.090624999385484628 ) ) ;
#10722 = CARTESIAN_POINT ( 'NONE',  ( -1.926257025242585782E-15, 196.0906250006145228, -31.45816453501075927 ) ) ;
#10723 = CARTESIAN_POINT ( 'NONE',  ( -8.927990412390371944, 99.92731371789854222, -13.04141134922778988 ) ) ;
#10724 = CARTESIAN_POINT ( 'NONE',  ( -30.79836230271183695, 204.3130714775002446, -3.149950860017828091 ) ) ;
#10725 = ORIENTED_EDGE ( 'NONE', *, *, #24289, .F. ) ;
#10726 = CARTESIAN_POINT ( 'NONE',  ( -3.253724281355068545E-15, 195.9500000012290002, -27.00000000000000000 ) ) ;
#10727 = CARTESIAN_POINT ( 'NONE',  ( -10.49813415415989581, 123.9726862821014493, -7.228626920339068285 ) ) ;
#10728 = EDGE_CURVE ( 'NONE', #16873, #18271, #20141, .T. ) ;
#10729 = CARTESIAN_POINT ( 'NONE',  ( 15.46528703574804986, 63.59768628210142793, 3.257655550457285720 ) ) ;
#10730 = LINE ( 'NONE', #7897, #11981 ) ;
#10731 =( BOUNDED_CURVE ( )  B_SPLINE_CURVE ( 2, ( #2323, #36810, #34160, #13894, #16554, #13011, #22613 ),
 .UNSPECIFIED., .F., .F. ) 
 B_SPLINE_CURVE_WITH_KNOTS ( ( 3, 2, 2, 3 ),
 ( 0.02173913043478229237, 0.02898550724637658296, 0.03623188405797087008, 0.04347826086956516067 ),
 .UNSPECIFIED. ) 
 CURVE ( )  GEOMETRIC_REPRESENTATION_ITEM ( )  RATIONAL_B_SPLINE_CURVE ( ( 1.000000000000005773, 0.8660254037844328234, 1.000000000000000000, 0.8660254037844387076, 1.000000000000000000, 0.8660254037844397068, 0.9999999999999990008 ) ) 
 REPRESENTATION_ITEM ( '' )  );
#10732 = CARTESIAN_POINT ( 'NONE',  ( 24.70858993122118363, 3.604726614523240613, 164.0263046051175024 ) ) ;
#10733 = CARTESIAN_POINT ( 'NONE',  ( 10.83675517735155225, 92.06018628210145494, 11.08355503943142573 ) ) ;
#10734 = CARTESIAN_POINT ( 'NONE',  ( -43.86830436395490551, 209.8844732041982581, 6.500000000000000888 ) ) ;
#10735 = CARTESIAN_POINT ( 'NONE',  ( 13.44051670066911086, 5.407089921784856479, -7.415624999385555860 ) ) ;
#10736 = CARTESIAN_POINT ( 'NONE',  ( -0.1745138560725182642, 28.81018628210143717, 9.500000000000005329 ) ) ;
#10737 = CARTESIAN_POINT ( 'NONE',  ( 18.00000000000000355, -5.196152422706632912, -3.525000000000000355 ) ) ;
#10738 = CARTESIAN_POINT ( 'NONE',  ( -60.49330436395489841, 210.1155267958017134, -6.500000000000000888 ) ) ;
#10739 = CARTESIAN_POINT ( 'NONE',  ( -3.253724281355068545E-15, 198.6500000012290172, -27.00000000000000000 ) ) ;
#10740 = CARTESIAN_POINT ( 'NONE',  ( -7.228626920339069173, 66.47268628210144925, 10.49813415415989581 ) ) ;
#10741 = CARTESIAN_POINT ( 'NONE',  ( 13.50000000000001421, 197.0000000000000000, 23.38268590217984055 ) ) ;
#10742 = CARTESIAN_POINT ( 'NONE',  ( -42.15435043487492095, 254.8329415120769283, -2.500000000000000000 ) ) ;
#10744 = CARTESIAN_POINT ( 'NONE',  ( 16.56230152254411436, 7.209453229046482114, -0.7593749993855121172 ) ) ;
#10743 = CARTESIAN_POINT ( 'NONE',  ( -2.064181346179269738, 19.89768628210143930, 9.465287035748067623 ) ) ;
#10745 = CARTESIAN_POINT ( 'NONE',  ( 15.00000000000000000, 241.8625000000000114, -3.464101615137752610 ) ) ;
#10746 = ORIENTED_EDGE ( 'NONE', *, *, #30201, .F. ) ;
#10747 = CARTESIAN_POINT ( 'NONE',  ( 26.99999999999999645, 3.464101615137755275, -2.887499999999991296 ) ) ;
#10748 = CARTESIAN_POINT ( 'NONE',  ( 25.05010001456683710, 0.000000000000000000, 165.1351344719413419 ) ) ;
#10749 = CARTESIAN_POINT ( 'NONE',  ( 36.85406125198851157, -3.604726614523238837, 159.5758215996624187 ) ) ;
#10750 = CARTESIAN_POINT ( 'NONE',  ( 10.31873187879411091, 3.604726614523236616, -2.428124999385521399 ) ) ;
#10751 = CARTESIAN_POINT ( 'NONE',  ( 28.30384396178233075, -5.407089921784859143, 169.3017823552670507 ) ) ;
#10752 = CARTESIAN_POINT ( 'NONE',  ( 18.00000000000000000, 242.7249999999999943, -5.196152422706630247 ) ) ;
#10753 = DIRECTION ( 'NONE',  ( -0.1219804832088915297, -0.9925324990730154395, 0.000000000000000000 ) ) ;
#10754 = EDGE_CURVE ( 'NONE', #22746, #29322, #9500, .T. ) ;
#10755 = CARTESIAN_POINT ( 'NONE',  ( -4.944772684328424539, 81.81481371789855928, -11.48171059495408031 ) ) ;
#10756 = CARTESIAN_POINT ( 'NONE',  ( 7.228626920339069173, 89.47268628210144925, -10.49813415415989404 ) ) ;
#10757 = ORIENTED_EDGE ( 'NONE', *, *, #18561, .T. ) ;
#10758 = EDGE_LOOP ( 'NONE', ( #27822, #7183, #1445, #23423 ) ) ;
#10759 = CARTESIAN_POINT ( 'NONE',  ( 26.99999999999999645, 197.2250000012290059, -15.58845726811990495 ) ) ;
#10760 = DIRECTION ( 'NONE',  ( 0.000000000000000000, 0.000000000000000000, 1.000000000000000000 ) ) ;
#10761 = CARTESIAN_POINT ( 'NONE',  ( -14.38691631536193860, 62.26481371789854791, -5.770363421894132649 ) ) ;
#10762 = CARTESIAN_POINT ( 'NONE',  ( 26.75643035624999655, 3.323476615752271712, -8.540624999385476812 ) ) ;
#10763 = ADVANCED_FACE ( 'NONE', ( #36510, #32739 ), #35954, .T. ) ;
#10764 = CARTESIAN_POINT ( 'NONE',  ( 21.00000000000000000, 242.3218750006145115, 6.646953231504538984 ) ) ;
#10765 = CARTESIAN_POINT ( 'NONE',  ( -56.13913769728823411, 207.8500491399821613, -3.954877714930864485 ) ) ;
#10766 = CARTESIAN_POINT ( 'NONE',  ( 8.710071997420211432, 47.31481371789856638, -3.796722387233181895 ) ) ;
#10767 = CARTESIAN_POINT ( 'NONE',  ( 22.80587116629411071, 3.604726614523238837, -9.778124999385536142 ) ) ;
#10768 = CARTESIAN_POINT ( 'NONE',  ( 0.1745138560723095977, 86.98981371789857064, 9.500000000000005329 ) ) ;
#10769 = CARTESIAN_POINT ( 'NONE',  ( -27.24356964374999635, 199.4468750006145399, 15.72908226750539384 ) ) ;
#10770 = CARTESIAN_POINT ( 'NONE',  ( -0.1745138560722763466, 8.789813717898553591, -12.50000000000000355 ) ) ;
#10771 =( BOUNDED_CURVE ( )  B_SPLINE_CURVE ( 2, ( #3403, #26331, #31835, #32212, #9097, #34865, #23501 ),
 .UNSPECIFIED., .F., .F. ) 
 B_SPLINE_CURVE_WITH_KNOTS ( ( 3, 2, 2, 3 ),
 ( 0.8260869565217380250, 0.8333333333333321491, 0.8405797101449260511, 0.8478260869565201752 ),
 .UNSPECIFIED. ) 
 CURVE ( )  GEOMETRIC_REPRESENTATION_ITEM ( )  RATIONAL_B_SPLINE_CURVE ( ( 1.000000000000020428, 0.8660254037844181685, 1.000000000000000000, 0.8660254037844387076, 1.000000000000000000, 0.8660254037844674624, 0.9999999999999712452 ) ) 
 REPRESENTATION_ITEM ( '' )  );
#10772 = CARTESIAN_POINT ( 'NONE',  ( -10.69584247140444866, 57.84768628210144925, 6.932735513423972762 ) ) ;
#10773 = CARTESIAN_POINT ( 'NONE',  ( 16.56230152254411081, -6.928203230275506996, -9.674999998771022902 ) ) ;
#10774 = CARTESIAN_POINT ( 'NONE',  ( 34.04199902021685631, 5.196152422706637353, 164.6495911966399888 ) ) ;
#10775 = CARTESIAN_POINT ( 'NONE',  ( 33.79808337967844523, 5.407089921784857367, 160.4642985439555218 ) ) ;
#10776 = CARTESIAN_POINT ( 'NONE',  ( 10.31873187879410736, 0.000000000000000000, -10.09687499938552513 ) ) ;
#10777 = CARTESIAN_POINT ( 'NONE',  ( 16.56230152254411436, 7.209453229046482114, -7.059374999385483740 ) ) ;
#10778 = CARTESIAN_POINT ( 'NONE',  ( 27.61379986294728184, -5.196152422706638241, 160.0172180905011032 ) ) ;
#10779 = ADVANCED_FACE ( 'NONE', ( #33119 ), #18350, .T. ) ;
#10780 = CARTESIAN_POINT ( 'NONE',  ( 0.000000000000000000, 143.0000000000000000, -24.80000000000000426 ) ) ;
#10781 = CARTESIAN_POINT ( 'NONE',  ( 5.233372021372432847, 101.5476862821014663, 8.152565276336710909 ) ) ;
#10782 = DIRECTION ( 'NONE',  ( 0.000000000000000000, 1.000000000000000000, 0.000000000000000000 ) ) ;
#10783 = CARTESIAN_POINT ( 'NONE',  ( 10.69584247140445221, 117.6476862821014464, -6.932735513423970097 ) ) ;
#10784 = DIRECTION ( 'NONE',  ( 1.000000000000000000, 0.000000000000000000, 0.000000000000000000 ) ) ;
#10785 = CARTESIAN_POINT ( 'NONE',  ( 10.56230152254410903, 0.000000000000000000, -0.4500000000000614619 ) ) ;
#10786 = ORIENTED_EDGE ( 'NONE', *, *, #15018, .T. ) ;
#10787 = CARTESIAN_POINT ( 'NONE',  ( 24.83442103481310781, 0.000000000000000000, 165.4645607004874535 ) ) ;
#10788 = CIRCLE ( 'NONE', #17447, 8.000000000000000000 ) ;
#10789 = CARTESIAN_POINT ( 'NONE',  ( 15.24356964374999990, 3.323476615752268604, -6.028124999385455318 ) ) ;
#10791 = EDGE_CURVE ( 'NONE', #30939, #33575, #5629, .T. ) ;
#10790 = CARTESIAN_POINT ( 'NONE',  ( -13.62178482187498396, 197.6843750006145228, 23.59362340125808188 ) ) ;
#10792 = CARTESIAN_POINT ( 'NONE',  ( 19.80074372294634344, 5.630122097104456991, -7.999999999999998224 ) ) ;
#10793 = CARTESIAN_POINT ( 'NONE',  ( 25.44556919728430699, -3.464101615137761048, 169.6553679145326328 ) ) ;
#10794 = CARTESIAN_POINT ( 'NONE',  ( 18.00000000000000000, 239.6312500012290343, -5.196152422706630247 ) ) ;
#10795 = CARTESIAN_POINT ( 'NONE',  ( 15.24356964374999990, 239.9593750006145285, 0.000000000000000000 ) ) ;
#10796 = LINE ( 'NONE', #27854, #27544 ) ;
#10797 = CARTESIAN_POINT ( 'NONE',  ( 4.622313124798831829, 138.1648137178985678, -11.61527771782809282 ) ) ;
#10798 = CARTESIAN_POINT ( 'NONE',  ( 10.69584247140445221, 136.0476862821014663, -6.932735513423970097 ) ) ;
#10800 = ORIENTED_EDGE ( 'NONE', *, *, #19639, .F. ) ;
#10799 = VERTEX_POINT ( 'NONE', #36171 ) ;
#10801 = CARTESIAN_POINT ( 'NONE',  ( 18.12178482187500350, 245.3218750006145115, 4.985214923628407568 ) ) ;
#10802 = EDGE_CURVE ( 'NONE', #6368, #31527, #6810, .T. ) ;
#10803 = CARTESIAN_POINT ( 'NONE',  ( -11.48171059495408208, 15.11481371789855110, 4.944772684328421875 ) ) ;
#10804 = CARTESIAN_POINT ( 'NONE',  ( 15.24356964375000167, -3.323476615752272600, -3.253124999385455407 ) ) ;
#10805 = CARTESIAN_POINT ( 'NONE',  ( 14.25334919248795451, 120.9148137178985678, -6.092822981423661410 ) ) ;
#10806 = CARTESIAN_POINT ( 'NONE',  ( 0.000000000000000000, 200.0000000000000000, 0.000000000000000000 ) ) ;
#10807 = CARTESIAN_POINT ( 'NONE',  ( 18.12178482187500350, -4.985214923628407568, -2.878124999385472726 ) ) ;
#10808 = CIRCLE ( 'NONE', #31983, 2.649999999999992806 ) ;
#10809 = CARTESIAN_POINT ( 'NONE',  ( 10.31873187879410381, -3.604726614523244610, -9.159374999385505589 ) ) ;
#10810 = CARTESIAN_POINT ( 'NONE',  ( -27.00000000000000355, 197.8625000012290513, 0.000000000000000000 ) ) ;
#10811 = CARTESIAN_POINT ( 'NONE',  ( -2.660918448318275509, 111.8976862821014606, 12.46528703574805874 ) ) ;
#10812 = CARTESIAN_POINT ( 'NONE',  ( 16.56230152254411081, -7.209453229046475009, -2.278124999385533922 ) ) ;
#10813 = ADVANCED_FACE ( 'NONE', ( #7013 ), #18773, .F. ) ;
#10814 = CARTESIAN_POINT ( 'NONE',  ( -39.11086230271183695, 214.1499508600178387, -7.418979330068641964 ) ) ;
#10815 = CARTESIAN_POINT ( 'NONE',  ( 15.24356964374999990, 244.3468750006145171, 0.000000000000000000 ) ) ;
#10816 = CARTESIAN_POINT ( 'NONE',  ( -77.00000000000002842, 210.0000000000000000, -2.499999999999998668 ) ) ;
#10817 = CARTESIAN_POINT ( 'NONE',  ( -30.20461230271183339, 208.6787018382582346, -4.469044688360757966 ) ) ;
#10818 = CARTESIAN_POINT ( 'NONE',  ( -11.48171059495397373, 123.6851862821014549, -4.944772684328680334 ) ) ;
#10819 = CARTESIAN_POINT ( 'NONE',  ( 10.56230152254411081, 0.000000000000000000, -0.3374999987710014526 ) ) ;
#10820 = CARTESIAN_POINT ( 'NONE',  ( -41.29538769728821990, 211.8571965466039444, -6.469044688360768625 ) ) ;
#10821 = CYLINDRICAL_SURFACE ( 'NONE', #24614, 7.500000000000000000 ) ;
#10822 = CARTESIAN_POINT ( 'NONE',  ( 19.39230484541326049, 244.5075961894323200, -5.999999999999997335 ) ) ;
#10823 = CARTESIAN_POINT ( 'NONE',  ( 3.257655550457285720, 116.4976862821014549, -15.46528703574804986 ) ) ;
#10824 = EDGE_CURVE ( 'NONE', #14417, #17309, #8054, .T. ) ;
#10825 = CARTESIAN_POINT ( 'NONE',  ( 26.99999999999999645, 198.0125000000000739, -15.58845726811990495 ) ) ;
#10826 = CARTESIAN_POINT ( 'NONE',  ( -11.48171059495397373, 13.28518628210142971, -4.944772684328680334 ) ) ;
#10827 = CARTESIAN_POINT ( 'NONE',  ( 22.56230152254411436, 3.464101615137759271, -8.737500000000032685 ) ) ;
#10828 = ORIENTED_EDGE ( 'NONE', *, *, #6247, .T. ) ;
#10829 = CARTESIAN_POINT ( 'NONE',  ( 6.500000000000000000, 244.5000000000000000, 0.000000000000000000 ) ) ;
#10830 = CARTESIAN_POINT ( 'NONE',  ( -8.710071997420127943, 77.68518628210145494, -3.796722387233380402 ) ) ;
#10831 = CARTESIAN_POINT ( 'NONE',  ( 5.778771075727756162E-15, 196.7656250006145342, 31.45816453501075927 ) ) ;
#10832 = CARTESIAN_POINT ( 'NONE',  ( 24.70692427760507570, 0.000000000000000000, 161.2126178494294493 ) ) ;
#10833 = CARTESIAN_POINT ( 'NONE',  ( -27.24356964375000345, 197.6093750006145342, 0.000000000000000000 ) ) ;
#10834 = DIRECTION ( 'NONE',  ( -1.000000000000000000, -6.123233995736766036E-17, 0.000000000000000000 ) ) ;
#10835 = CARTESIAN_POINT ( 'NONE',  ( 10.56230152254411436, 3.464101615137752610, -6.674999998771008691 ) ) ;
#10836 = SHAPE_REPRESENTATION ( 'Cylinder', ( #17215 ), #33555 ) ;
#10837 = CARTESIAN_POINT ( 'NONE',  ( 1.715153634034445762, 64.27731371789853654, -9.534712964251895073 ) ) ;
#10838 = CARTESIAN_POINT ( 'NONE',  ( 23.99999999999999645, 5.196152422706631135, -9.599999999999997868 ) ) ;
#10839 = ORIENTED_EDGE ( 'NONE', *, *, #1006, .T. ) ;
#10840 = EDGE_CURVE ( 'NONE', #8243, #205, #24257, .T. ) ;
#10841 = CARTESIAN_POINT ( 'NONE',  ( 15.00000000000000000, 241.4687500012290684, -3.464101615137752166 ) ) ;
#10842 = CARTESIAN_POINT ( 'NONE',  ( 12.46528703574811558, 66.00231371789855928, -2.660918448318005947 ) ) ;
#10843 = CARTESIAN_POINT ( 'NONE',  ( 19.68408634441911431, 5.407089921784862696, -5.746874999385531702 ) ) ;
#10844 = CARTESIAN_POINT ( 'NONE',  ( 26.75643035624999655, -3.323476615752267715, -5.915624999385464378 ) ) ;
#10845 = CARTESIAN_POINT ( 'NONE',  ( -6.932735513424201912, 32.65231371789854364, 10.69584247140429412 ) ) ;
#10846 = ORIENTED_EDGE ( 'NONE', *, *, #3559, .T. ) ;
#10847 = UNCERTAINTY_MEASURE_WITH_UNIT (LENGTH_MEASURE( 1.000000000000000082E-05 ), #27171, 'distance_accuracy_value', 'NONE');
#10848 = CARTESIAN_POINT ( 'NONE',  ( 13.44051670066910908, 5.407089921784862696, -2.071874999385547866 ) ) ;
#10849 = FACE_OUTER_BOUND ( 'NONE', #16526, .T. ) ;
#10850 = CARTESIAN_POINT ( 'NONE',  ( 37.56329110859752518, 7.646167579472024665E-16, 167.6823559553839971 ) ) ;
#10851 = CARTESIAN_POINT ( 'NONE',  ( -48.41294563604515133, 214.6737587650350747, -4.842901733360249317 ) ) ;
#10852 = CARTESIAN_POINT ( 'NONE',  ( 10.49999999999999645, 252.0000000000000000, 2.500000000000013323 ) ) ;
#10853 =( NAMED_UNIT ( * ) SI_UNIT ( $, .STERADIAN. ) SOLID_ANGLE_UNIT ( ) );
#10854 = CARTESIAN_POINT ( 'NONE',  ( 19.56230152254411792, 5.196152422706637353, -2.850000000000019185 ) ) ;
#10855 = CARTESIAN_POINT ( 'NONE',  ( -7.228626920338836470, 63.12731371789855217, -10.49813415416005213 ) ) ;
#10856 = EDGE_CURVE ( 'NONE', #18997, #30939, #13256, .T. ) ;
#10857 = CARTESIAN_POINT ( 'NONE',  ( -34.96205436395489841, 213.2096571498974242, 3.378800118222489601 ) ) ;
#10858 = CARTESIAN_POINT ( 'NONE',  ( -49.80580436395490551, 216.5000000000000000, 0.1155267958017343610 ) ) ;
#10859 = CYLINDRICAL_SURFACE ( 'NONE', #975, 5.999999999999998224 ) ;
#10860 = CARTESIAN_POINT ( 'NONE',  ( -9.244191109966227060, 218.8665654034646479, -3.366944586054378519 ) ) ;
#10861 = CARTESIAN_POINT ( 'NONE',  ( -6.092822981423666739, 35.81481371789853796, -14.25334919248795096 ) ) ;
#10862 = CARTESIAN_POINT ( 'NONE',  ( -67.42038769728826253, 207.6069050685337913, 8.469044688360781947 ) ) ;
#10863 = CARTESIAN_POINT ( 'NONE',  ( 2.311890736173175753, 19.32268628210144712, 12.53471296425194836 ) ) ;
#10864 = CARTESIAN_POINT ( 'NONE',  ( 2.660918448318279950, 70.49768628210145494, -12.46528703574805697 ) ) ;
#10865 = EDGE_CURVE ( 'NONE', #1101, #17216, #6839, .T. ) ;
#10866 = CARTESIAN_POINT ( 'NONE',  ( -15.46528703574804986, 3.797686282101448096, -3.257655550457287497 ) ) ;
#10867 = CARTESIAN_POINT ( 'NONE',  ( 16.56230152254411436, -6.928203230275514990, -2.587500000000015454 ) ) ;
#10868 = CARTESIAN_POINT ( 'NONE',  ( 21.00000000000000355, 0.000000000000000000, 50.00000000000001421 ) ) ;
#10869 = ORIENTED_EDGE ( 'NONE', *, *, #18419, .T. ) ;
#10870 = CARTESIAN_POINT ( 'NONE',  ( 2.908627838312118019, 28.52268628210144286, 15.53471296425195369 ) ) ;
#10871 = CARTESIAN_POINT ( 'NONE',  ( 27.24356964375000700, 195.0406250006145399, 15.72908226750537075 ) ) ;
#10872 = CARTESIAN_POINT ( 'NONE',  ( -1.926257025242585782E-15, 198.8468750006145740, -31.45816453501075927 ) ) ;
#10873 = CARTESIAN_POINT ( 'NONE',  ( 23.99999999999999645, 247.5999999999999943, -5.196152422706631135 ) ) ;
#10874 = CARTESIAN_POINT ( 'NONE',  ( 27.65301994718372569, -5.196152422706638241, 160.4655057046423678 ) ) ;
#10875 = CARTESIAN_POINT ( 'NONE',  ( 22.56230152254410370, 0.000000000000000000, -10.00000000000000000 ) ) ;
#10876 = CARTESIAN_POINT ( 'NONE',  ( 13.49999999999999645, 196.3625000012290513, -23.38268590217984766 ) ) ;
#10877 = CARTESIAN_POINT ( 'NONE',  ( 15.24356964374999990, 248.0218750006145285, -3.323476615752268604 ) ) ;
#10878 = CARTESIAN_POINT ( 'NONE',  ( -6.594114490232462877, 115.7398137178985564, 6.840914352311949109 ) ) ;
#10879 = CARTESIAN_POINT ( 'NONE',  ( 26.75643035624999655, 242.8468750006145171, 3.323476615752267271 ) ) ;
#10880 = VERTEX_POINT ( 'NONE', #24623 ) ;
#10881 = CARTESIAN_POINT ( 'NONE',  ( -66.82663769728823411, 204.3130714775002730, 3.149950860017883603 ) ) ;
#10882 = FILL_AREA_STYLE ('',( #22455 ) ) ;
#10883 = CARTESIAN_POINT ( 'NONE',  ( 26.99999999999999645, 247.6187500012290741, -3.464101615137755275 ) ) ;
#10884 = CARTESIAN_POINT ( 'NONE',  ( -10.49813415416004858, 125.2273137178985820, 7.228626920338840023 ) ) ;
#10885 = CARTESIAN_POINT ( 'NONE',  ( 16.56230152254411081, 7.209453229046475009, -9.703124999385542182 ) ) ;
#10886 = CARTESIAN_POINT ( 'NONE',  ( 27.58480908411420529, 5.407089921784856479, 161.0831760960101349 ) ) ;
#10887 = CARTESIAN_POINT ( 'NONE',  ( 26.75643035624999655, 3.323476615752271712, -0.4406249993854897129 ) ) ;
#10888 = CARTESIAN_POINT ( 'NONE',  ( -27.00000000000000355, 195.9500000000000171, 0.000000000000000000 ) ) ;
#10889 = ORIENTED_EDGE ( 'NONE', *, *, #62, .F. ) ;
#10890 = ORIENTED_EDGE ( 'NONE', *, *, #24524, .T. ) ;
#10891 = VECTOR ( 'NONE', #20532, 1000.000000000000000 ) ;
#10892 = ORIENTED_EDGE ( 'NONE', *, *, #10287, .F. ) ;
#10893 = CARTESIAN_POINT ( 'NONE',  ( 21.00000000000000000, 6.928203230275506996, -4.556249998770971921 ) ) ;
#10894 = CARTESIAN_POINT ( 'NONE',  ( 26.75643035624999655, 7.049594010296217766E-16, -2.615624999385474325 ) ) ;
#10895 = CARTESIAN_POINT ( 'NONE',  ( 10.56230152254410903, 0.000000000000000000, -4.500000000000031974 ) ) ;
#10896 = CARTESIAN_POINT ( 'NONE',  ( 10.56230152254455490, -3.464101615138013734, -1.312500000000048850 ) ) ;
#10897 = CARTESIAN_POINT ( 'NONE',  ( 23.87821517812500005, 248.0968750006144887, 4.985214923628404016 ) ) ;
#10898 = CARTESIAN_POINT ( 'NONE',  ( -11.61527771782819940, 58.13518628210144357, 4.622313124798574258 ) ) ;
#10899 = CARTESIAN_POINT ( 'NONE',  ( -61.67336230271183695, 215.6869285224997270, 3.149950860017831200 ) ) ;
#10900 = CARTESIAN_POINT ( 'NONE',  ( 6.418300056333647419, 215.4681374788750361, 2.477503916095803227 ) ) ;
#10901 = CARTESIAN_POINT ( 'NONE',  ( -45.84002896937850124, 206.1606490808709111, 2.350049139982143931 ) ) ;
#10902 = FILL_AREA_STYLE_COLOUR ( '', #22059 ) ;
#10903 = AXIS2_PLACEMENT_3D ( 'NONE', #23942, #35863, #990 ) ;
#10904 = CARTESIAN_POINT ( 'NONE',  ( 37.06980319883564334, -3.464101615137751278, 164.8364115837626400 ) ) ;
#10905 = CARTESIAN_POINT ( 'NONE',  ( 2.660918448318002838, 114.3023137178985564, 12.46528703574811558 ) ) ;
#10906 = CARTESIAN_POINT ( 'NONE',  ( -39.31622103062156270, 211.6261429550005744, 6.530955311639227823 ) ) ;
#10907 = CARTESIAN_POINT ( 'NONE',  ( -40.50372103062156981, 218.5309553116391896, -2.162041339862839084 ) ) ;
#10908 = CARTESIAN_POINT ( 'NONE',  ( 26.75643035624999655, -3.323476615752267271, -1.415624999385507232 ) ) ;
#10909 = CARTESIAN_POINT ( 'NONE',  ( 27.24356964375000700, 195.4906250006145001, 15.72908226750537075 ) ) ;
#10910 = CARTESIAN_POINT ( 'NONE',  ( 15.46528703574811736, 102.8023137178985422, -3.257655550456947768 ) ) ;
#10911 = CARTESIAN_POINT ( 'NONE',  ( -31.39211230271182984, 203.5309553116391612, 1.857196546604092280 ) ) ;
#10912 = ORIENTED_EDGE ( 'NONE', *, *, #12928, .T. ) ;
#10913 = CARTESIAN_POINT ( 'NONE',  ( 22.60769515458672885, 242.0888461906613713, 5.999999999999997335 ) ) ;
#10914 = CARTESIAN_POINT ( 'NONE',  ( 0.1745138560725515708, 125.4101862821014635, -12.50000000000000355 ) ) ;
#10915 = CARTESIAN_POINT ( 'NONE',  ( -5.770363421893818234, 60.43518628210146204, -14.38691631536207005 ) ) ;
#10916 = FACE_OUTER_BOUND ( 'NONE', #18657, .T. ) ;
#10917 = CARTESIAN_POINT ( 'NONE',  ( 37.25279877505902704, 3.604726614523243278, 164.1334123434321270 ) ) ;
#10918 = VECTOR ( 'NONE', #35427, 1000.000000000000114 ) ;
#10919 = CARTESIAN_POINT ( 'NONE',  ( 13.04141134922759804, 82.57268628210144357, 8.927990412390657937 ) ) ;
#10920 = CARTESIAN_POINT ( 'NONE',  ( -46.24330436395489841, 210.1155267958017134, -6.500000000000000888 ) ) ;
#10921 = CARTESIAN_POINT ( 'NONE',  ( 22.80587116629411071, -3.604726614523235284, -7.153124999385556571 ) ) ;
#10922 = CARTESIAN_POINT ( 'NONE',  ( -8.152565276336710909, 21.04768628210144499, 5.233372021372435512 ) ) ;
#10923 = CARTESIAN_POINT ( 'NONE',  ( 36.59262550718515428, 7.347880794884125653E-16, 159.3822456104860237 ) ) ;
#10924 = CARTESIAN_POINT ( 'NONE',  ( -61.68080436395489841, 203.5000000000000000, -0.1155267958017335561 ) ) ;
#10925 = CARTESIAN_POINT ( 'NONE',  ( 20.99999999999999289, 249.2125000000000057, 5.999999999999999112 ) ) ;
#10926 = CARTESIAN_POINT ( 'NONE',  ( -12.50000000000000355, 58.71018628210145351, -0.1745138560725492671 ) ) ;
#10927 = CARTESIAN_POINT ( 'NONE',  ( -1.909035429704832693E-15, 197.6375000000000171, -31.17691453623979214 ) ) ;
#10928 = DIRECTION ( 'NONE',  ( 0.000000000000000000, -0.000000000000000000, 1.000000000000000000 ) ) ;
#10930 = CARTESIAN_POINT ( 'NONE',  ( 22.56230152254411792, 7.347880794884125653E-16, -2.025000000000027001 ) ) ;
#10929 = CARTESIAN_POINT ( 'NONE',  ( -0.1745138560725182642, 28.81018628210143717, 9.500000000000005329 ) ) ;
#10931 = CARTESIAN_POINT ( 'NONE',  ( 20.99999999999999645, 249.5218750006145285, 6.646953231504538984 ) ) ;
#10932 = ORIENTED_EDGE ( 'NONE', *, *, #30455, .F. ) ;
#10933 = CARTESIAN_POINT ( 'NONE',  ( 15.00000000000000000, 3.464101615137752166, -1.837499999999979927 ) ) ;
#10934 = CARTESIAN_POINT ( 'NONE',  ( 2.999999999999997335, 237.0000000000000000, 5.000000000000000000 ) ) ;
#10935 = AXIS2_PLACEMENT_3D ( 'NONE', #10343, #7320, #18521 ) ;
#10936 = CARTESIAN_POINT ( 'NONE',  ( 30.68654372136677466, 7.209453229046482114, 160.7177013682151596 ) ) ;
#10937 = CARTESIAN_POINT ( 'NONE',  ( 10.31873187879411091, 0.000000000000000000, -2.390624999385526639 ) ) ;
#10938 = CARTESIAN_POINT ( 'NONE',  ( 31.37779770603408380, -7.209453229046475009, 168.6187705674553285 ) ) ;
#10939 =( BOUNDED_CURVE ( )  B_SPLINE_CURVE ( 2, ( #19333, #7939, #2609, #19515, #22907, #31061, #5271, #13818, #5085 ),
 .UNSPECIFIED., .F., .F. ) 
 B_SPLINE_CURVE_WITH_KNOTS ( ( 3, 2, 2, 2, 3 ),
 ( 0.4456521739130434590, 0.4492753623188405765, 0.4565217391304347561, 0.4637681159420289911, 0.4673913043478261087 ),
 .UNSPECIFIED. ) 
 CURVE ( )  GEOMETRIC_REPRESENTATION_ITEM ( )  RATIONAL_B_SPLINE_CURVE ( ( 0.9330127018922191873, 0.9330127018922187432, 1.000000000000000000, 0.8660254037844387076, 1.000000000000000000, 0.8660254037844387076, 1.000000000000000000, 0.9330127018922188542, 0.9330127018922194093 ) ) 
 REPRESENTATION_ITEM ( '' )  );
#10940 = CARTESIAN_POINT ( 'NONE',  ( 23.99999999999999645, 244.4499999999999886, -5.196152422706631135 ) ) ;
#10941 = CARTESIAN_POINT ( 'NONE',  ( -27.00000000000000355, 196.5125000012290570, 0.000000000000000000 ) ) ;
#10942 = CARTESIAN_POINT ( 'NONE',  ( -2.311890736173176641, 79.12268628210145494, -12.53471296425194659 ) ) ;
#10943 = VERTEX_POINT ( 'NONE', #18953 ) ;
#10944 = ORIENTED_EDGE ( 'NONE', *, *, #19321, .T. ) ;
#10945 = CARTESIAN_POINT ( 'NONE',  ( -13.50000000000000533, 195.9875000012290229, -23.38268590217984411 ) ) ;
#10946 = CARTESIAN_POINT ( 'NONE',  ( -73.23181873377778572, 221.0662276635146384, 5.000000000000000000 ) ) ;
#10947 = CARTESIAN_POINT ( 'NONE',  ( 15.46528703574811736, 56.80231371789854933, -3.257655550456947768 ) ) ;
#10948 = CARTESIAN_POINT ( 'NONE',  ( 15.24356964374999990, 3.323476615752268604, -10.19062499938547184 ) ) ;
#10949 = CARTESIAN_POINT ( 'NONE',  ( 26.75643035624999655, 242.9218750006145626, -3.323476615752271712 ) ) ;
#10950 = CARTESIAN_POINT ( 'NONE',  ( -43.27455436395490551, 206.6211998817774997, 3.209657149897401585 ) ) ;
#10951 = CARTESIAN_POINT ( 'NONE',  ( -13.50000000000000533, 199.4750000000000227, -23.38268590217984411 ) ) ;
#10952 = CARTESIAN_POINT ( 'NONE',  ( -8.710071997420207879, 33.51481371789854791, 3.796722387233182339 ) ) ;
#10953 = CARTESIAN_POINT ( 'NONE',  ( 25.12527184268644476, 3.464101615137619383, 165.9943523990454821 ) ) ;
#10954 =( BOUNDED_CURVE ( )  B_SPLINE_CURVE ( 2, ( #28430, #20293, #14043, #17259, #28800, #2836, #14408, #8129, #11560 ),
 .UNSPECIFIED., .F., .F. ) 
 B_SPLINE_CURVE_WITH_KNOTS ( ( 3, 2, 2, 2, 3 ),
 ( 0.9239130434782608647, 0.9275362318840579823, 0.9347826086956522174, 0.9420289855072463414, 0.9456521739130434590 ),
 .UNSPECIFIED. ) 
 CURVE ( )  GEOMETRIC_REPRESENTATION_ITEM ( )  RATIONAL_B_SPLINE_CURVE ( ( 0.9330127018922194093, 0.9330127018922194093, 1.000000000000000000, 0.8660254037844387076, 1.000000000000000000, 0.8660254037844387076, 1.000000000000000000, 0.9330127018922194093, 0.9330127018922194093 ) ) 
 REPRESENTATION_ITEM ( '' )  );
#10955 = CARTESIAN_POINT ( 'NONE',  ( -8.710071997420207879, 88.71481371789855075, 3.796722387233182339 ) ) ;
#10956 = CARTESIAN_POINT ( 'NONE',  ( -27.24356964374999635, 198.0968750006145456, 15.72908226750539384 ) ) ;
#10957 = CARTESIAN_POINT ( 'NONE',  ( -15.46528703574811736, 144.2023137178985905, 3.257655550456946436 ) ) ;
#10958 = CARTESIAN_POINT ( 'NONE',  ( 12.46528703574805874, 63.59768628210145636, 2.660918448318279950 ) ) ;
#10959 = CARTESIAN_POINT ( 'NONE',  ( 10.56230152254410903, 0.000000000000000000, -8.437499998771025744 ) ) ;
#10960 = DIRECTION ( 'NONE',  ( 0.000000000000000000, 0.000000000000000000, -1.000000000000000000 ) ) ;
#10961 = CARTESIAN_POINT ( 'NONE',  ( 24.60236886974748316, -3.604726614523240613, 162.8121923168181695 ) ) ;
#10962 = CARTESIAN_POINT ( 'NONE',  ( 13.44051670066910908, 5.407089921784862696, -9.721874999385510918 ) ) ;
#10963 = CARTESIAN_POINT ( 'NONE',  ( 13.44051670066911441, -5.407089921784865361, -6.871874999385546801 ) ) ;
#10964 = DIRECTION ( 'NONE',  ( -0.5887012860850802110, 0.8083506638593008775, 0.000000000000000000 ) ) ;
#10965 = CARTESIAN_POINT ( 'NONE',  ( 26.99999999999999645, 247.1312500012290343, -7.347880794884117764E-16 ) ) ;
#10966 = CARTESIAN_POINT ( 'NONE',  ( -9.500000000000005329, 67.91018628210144925, -0.1745138560725176813 ) ) ;
#10967 = CARTESIAN_POINT ( 'NONE',  ( 0.000000000000000000, 200.0000000000000000, -27.00000000000000355 ) ) ;
#10968 = CARTESIAN_POINT ( 'NONE',  ( -12.50000000000000355, 113.9101862821014493, -0.1745138560725492671 ) ) ;
#10969 = CARTESIAN_POINT ( 'NONE',  ( 17.54540804174073187, 195.0000000000000000, -20.52215039046394907 ) ) ;
#10970 = DIRECTION ( 'NONE',  ( -0.000000000000000000, -1.000000000000000000, -0.000000000000000000 ) ) ;
#10972 = ORIENTED_EDGE ( 'NONE', *, *, #9183, .F. ) ;
#10971 = CIRCLE ( 'NONE', #29111, 5.999999999999999112 ) ;
#10973 = CIRCLE ( 'NONE', #30352, 27.00000000000000000 ) ;
#10974 = CARTESIAN_POINT ( 'NONE',  ( 30.71105627401454896, -7.209453229046475009, 160.9978811270534891 ) ) ;
#10975 = CARTESIAN_POINT ( 'NONE',  ( 18.12178482187500350, -4.985214923628407568, -6.365624999385477878 ) ) ;
#10976 = CARTESIAN_POINT ( 'NONE',  ( -27.24356964375000345, 198.4718750006145171, -15.72908226750537786 ) ) ;
#10977 = CARTESIAN_POINT ( 'NONE',  ( 34.32918868704696536, -5.407089921784861808, 166.5348599854521296 ) ) ;
#10978 = CARTESIAN_POINT ( 'NONE',  ( 28.22824784931821895, 5.196152422706636465, 167.0403907120479232 ) ) ;
#10979 = CARTESIAN_POINT ( 'NONE',  ( 15.00000000000000000, 239.6687500012290570, -3.464101615137752610 ) ) ;
#10980 = CARTESIAN_POINT ( 'NONE',  ( 18.12178482187500350, 240.0343750006145171, 4.985214923628407568 ) ) ;
#10981 = DIRECTION ( 'NONE',  ( 0.000000000000000000, 0.000000000000000000, 1.000000000000000000 ) ) ;
#10982 = CARTESIAN_POINT ( 'NONE',  ( 12.53471296425189330, 130.9773137178985678, 2.311890736173451977 ) ) ;
#10983 = CARTESIAN_POINT ( 'NONE',  ( -8.715434833791929847, 133.4601862821014606, -8.962234695871762469 ) ) ;
#10985 = VERTEX_POINT ( 'NONE', #18582 ) ;
#10984 = ORIENTED_EDGE ( 'NONE', *, *, #10071, .T. ) ;
#10986 = CARTESIAN_POINT ( 'NONE',  ( 15.24356964374999990, 243.8593750006145342, -3.323476615752268604 ) ) ;
#10987 = CARTESIAN_POINT ( 'NONE',  ( 17.00000000000000000, 4.898587196589406912E-16, 50.17464377163448574 ) ) ;
#10988 = CARTESIAN_POINT ( 'NONE',  ( 21.00000000000000000, -6.646953231504538984, -3.178124999385461003 ) ) ;
#10989 = CARTESIAN_POINT ( 'NONE',  ( -6.092822981423666739, 109.4148137178985536, -14.25334919248795096 ) ) ;
#10990 = CARTESIAN_POINT ( 'NONE',  ( 14.85533981743163245, -6.020045154339302762, -9.999999999999998224 ) ) ;
#10991 = EDGE_CURVE ( 'NONE', #30074, #14298, #3195, .T. ) ;
#10992 = CARTESIAN_POINT ( 'NONE',  ( 18.12178482187500350, -4.985214923628407568, -1.978124999385488803 ) ) ;
#10993 = CARTESIAN_POINT ( 'NONE',  ( 22.80587116629411071, 3.604726614523243278, -8.934374999385493510 ) ) ;
#10994 = CARTESIAN_POINT ( 'NONE',  ( -13.50000000000000533, 199.5875000012290457, -23.38268590217984411 ) ) ;
#10995 = AXIS2_PLACEMENT_3D ( 'NONE', #26958, #989, #22181 ) ;
#10996 = CARTESIAN_POINT ( 'NONE',  ( -0.1745138560725500443, 111.6101862821014521, 12.50000000000000355 ) ) ;
#10997 = CARTESIAN_POINT ( 'NONE',  ( 13.44051670066911264, 5.407089921784856479, -3.815624999385564209 ) ) ;
#10998 = CARTESIAN_POINT ( 'NONE',  ( -48.01711230271184405, 218.4690446883607535, -2.393094931466363651 ) ) ;
#10999 = CARTESIAN_POINT ( 'NONE',  ( 20.99999999999999645, 244.4593750006145285, 6.646953231504538984 ) ) ;
#11000 = AXIS2_PLACEMENT_3D ( 'NONE', #21011, #15500, #29703 ) ;
#11001 = CARTESIAN_POINT ( 'NONE',  ( 23.99999999999999645, 240.4000000000000057, -5.196152422706631135 ) ) ;
#11002 = CARTESIAN_POINT ( 'NONE',  ( -35.54836230271182984, 206.0451222850691977, -2.149950860017851184 ) ) ;
#11003 = CARTESIAN_POINT ( 'NONE',  ( -12.53471296425194836, 122.8226862821014720, 2.311890736173176641 ) ) ;
#11004 = CARTESIAN_POINT ( 'NONE',  ( 19.56230152254411792, -5.196152422706629359, -1.987499998771014020 ) ) ;
#11005 = CARTESIAN_POINT ( 'NONE',  ( -47.82663769728823411, 204.3130714775002730, 3.149950860017883603 ) ) ;
#11006 = CARTESIAN_POINT ( 'NONE',  ( -47.00000000000000711, 244.5000000000000000, 5.000000000000000000 ) ) ;
#11007 = CARTESIAN_POINT ( 'NONE',  ( 15.46528703574804986, 100.3976862821014606, 3.257655550457285720 ) ) ;
#11008 = ADVANCED_FACE ( 'NONE', ( #27276 ), #35613, .T. ) ;
#11009 = CARTESIAN_POINT ( 'NONE',  ( -12.50000000000000355, 12.71018628210143753, -0.1745138560725492671 ) ) ;
#11010 = CARTESIAN_POINT ( 'NONE',  ( 20.99999999999995026, 242.7437500012290741, -5.999999999999998224 ) ) ;
#11011 = CARTESIAN_POINT ( 'NONE',  ( -7.954856959092191815, 133.1726862821014663, -5.529263428287477744 ) ) ;
#11012 = CARTESIAN_POINT ( 'NONE',  ( 19.68408634441910721, -5.407089921784855591, -0.4406249993855471114 ) ) ;
#11013 = CARTESIAN_POINT ( 'NONE',  ( 20.99999999999997513, 245.8937500012290798, -5.999999999999999112 ) ) ;
#11014 = VERTEX_POINT ( 'NONE', #29935 ) ;
#11015 = CARTESIAN_POINT ( 'NONE',  ( -0.5000000000000047740, 244.5000000000000000, 0.000000000000000000 ) ) ;
#11016 = CARTESIAN_POINT ( 'NONE',  ( 8.710071997420127943, 63.88518628210145778, 3.796722387233375073 ) ) ;
#11017 = VECTOR ( 'NONE', #35577, 1000.000000000000000 ) ;
#11018 = CARTESIAN_POINT ( 'NONE',  ( 16.56230152254411081, 6.928203230275506996, -2.249999998771013310 ) ) ;
#11019 = CARTESIAN_POINT ( 'NONE',  ( 27.24356964374999635, 196.4656250006145228, -15.72908226750539029 ) ) ;
#11020 = DIRECTION ( 'NONE',  ( 0.000000000000000000, 0.000000000000000000, 1.000000000000000000 ) ) ;
#11021 = CARTESIAN_POINT ( 'NONE',  ( 15.02283181144952628, 7.347880794884122694E-16, 50.52293445648592751 ) ) ;
#11022 = CYLINDRICAL_SURFACE ( 'NONE', #8359, 27.00000000000000355 ) ;
#11023 = CARTESIAN_POINT ( 'NONE',  ( 2.999999999999997335, 244.5000000000000000, 2.500000000000000000 ) ) ;
#11024 = CARTESIAN_POINT ( 'NONE',  ( 8.843639120294245259, 48.46481371789856496, 3.474262827703527901 ) ) ;
#11025 = CARTESIAN_POINT ( 'NONE',  ( 21.00000000000000000, -6.928203230275506996, -8.887499999999988631 ) ) ;
#11026 = ORIENTED_EDGE ( 'NONE', *, *, #5250, .F. ) ;
#11027 = CARTESIAN_POINT ( 'NONE',  ( 15.00000000000000178, 241.0937500012290116, 3.464101615137757051 ) ) ;
#11028 = CARTESIAN_POINT ( 'NONE',  ( -10.69584247140429412, 62.55231371789855643, -6.932735513424201024 ) ) ;
#11029 = CARTESIAN_POINT ( 'NONE',  ( 13.44051670066910908, 5.407089921784862696, -6.571874999385523886 ) ) ;
#11030 = CARTESIAN_POINT ( 'NONE',  ( 21.00000000000000000, 6.646953231504538984, -8.015624999385487115 ) ) ;
#11031 = CARTESIAN_POINT ( 'NONE',  ( -12.50000000000000355, 34.08981371789854364, 0.1745138560722786503 ) ) ;
#11032 = B_SPLINE_CURVE_WITH_KNOTS ( 'NONE', 3,
 ( #19681, #29670, #32137, #18316, #20783, #23807, #9401, #6940, #4082, #35163, #9771, #3518 ),
 .UNSPECIFIED., .F., .F.,
 ( 4, 2, 2, 2, 2, 4 ),
 ( -2.000000094622903833E-05, 0.002989282327806173489, 0.005998564656558575368, 0.007503205820934752239, 0.009007846985310929977, 0.01201712931406334617 ),
 .UNSPECIFIED. ) ;
#11033 = ORIENTED_EDGE ( 'NONE', *, *, #24687, .F. ) ;
#11034 = CARTESIAN_POINT ( 'NONE',  ( 10.31873187879410736, -3.604726614523244610, -1.059374999385519933 ) ) ;
#11035 = CARTESIAN_POINT ( 'NONE',  ( -10.49813415415989581, 4.372686282101440725, -7.228626920339068285 ) ) ;
#11036 =( BOUNDED_CURVE ( )  B_SPLINE_CURVE ( 2, ( #37297, #7948, #17228, #2065, #11346, #22918, #34463, #25192, #28766 ),
 .UNSPECIFIED., .F., .T. ) 
 B_SPLINE_CURVE_WITH_KNOTS ( ( 3, 2, 2, 2, 3 ),
 ( 0.4791666666666666852, 0.4861111111111111049, 0.5000000000000000000, 0.5138888888888888395, 0.5208333333333333703 ),
 .UNSPECIFIED. ) 
 CURVE ( )  GEOMETRIC_REPRESENTATION_ITEM ( )  RATIONAL_B_SPLINE_CURVE ( ( 0.9330127018922194093, 0.9330127018922196314, 1.000000000000000000, 0.8660254037844387076, 1.000000000000000000, 0.8660254037844387076, 1.000000000000000000, 0.9330127018922187432, 0.9330127018922192983 ) ) 
 REPRESENTATION_ITEM ( '' )  );
#11037 = CARTESIAN_POINT ( 'NONE',  ( 25.17923094205850276, 3.604726614523240613, 169.4057559748129336 ) ) ;
#11038 = CARTESIAN_POINT ( 'NONE',  ( -47.02752896937850124, 213.3500491399821613, 5.571401726697954970 ) ) ;
#11039 = DIRECTION ( 'NONE',  ( -1.000000000000000000, 0.000000000000000000, -2.057406622567553763E-16 ) ) ;
#11040 = CARTESIAN_POINT ( 'NONE',  ( -7.946041369334237991, 195.0000000000000000, 26.05901981062767092 ) ) ;
#11041 = CARTESIAN_POINT ( 'NONE',  ( -32.98288769728823411, 205.5309553116392465, -1.321298161741839117 ) ) ;
#11042 = CARTESIAN_POINT ( 'NONE',  ( -44.26413769728823411, 213.1499508600178672, 5.686928522499718142 ) ) ;
#11043 = ORIENTED_EDGE ( 'NONE', *, *, #1288, .F. ) ;
#11044 = CARTESIAN_POINT ( 'NONE',  ( -13.49999999999998401, 197.9375000012290400, 23.38268590217985476 ) ) ;
#11045 = CARTESIAN_POINT ( 'NONE',  ( 18.00000000000000000, 5.196152422706630247, -1.368749998770957266 ) ) ;
#11046 = CARTESIAN_POINT ( 'NONE',  ( 13.04141134922778988, 37.82731371789854080, -8.927990412390371944 ) ) ;
#11047 = CARTESIAN_POINT ( 'NONE',  ( -31.78794563604516910, 203.8621396198271043, 6.307003348498029460 ) ) ;
#11048 = PRODUCT_DEFINITION_SHAPE ( 'NONE', 'NONE',  #37512 ) ;
#11049 = CARTESIAN_POINT ( 'NONE',  ( -4.622313124798576922, 5.235186282101428112, -11.61527771782819762 ) ) ;
#11050 = CARTESIAN_POINT ( 'NONE',  ( -8.962234695871760692, 57.56018628210145494, 8.715434833791933400 ) ) ;
#11051 = CARTESIAN_POINT ( 'NONE',  ( 0.1745138560725837118, 5.810186282101448718, -15.50000000000000533 ) ) ;
#11052 = CARTESIAN_POINT ( 'NONE',  ( 22.56230152254411792, 7.347880794884125653E-16, -2.475000000000060485 ) ) ;
#11053 =( BOUNDED_CURVE ( )  B_SPLINE_CURVE ( 2, ( #8373, #26349, #17463, #3042, #16907, #3230, #6067 ),
 .UNSPECIFIED., .F., .F. ) 
 B_SPLINE_CURVE_WITH_KNOTS ( ( 3, 2, 2, 3 ),
 ( 0.4999999999999990008, 0.5072463768115932359, 0.5144927536231874710, 0.5217391304347817060 ),
 .UNSPECIFIED. ) 
 CURVE ( )  GEOMETRIC_REPRESENTATION_ITEM ( )  RATIONAL_B_SPLINE_CURVE ( ( 1.000000000000018430, 0.8660254037844202779, 1.000000000000000000, 0.8660254037844387076, 1.000000000000000000, 0.8660254037844551389, 0.9999999999999835687 ) ) 
 REPRESENTATION_ITEM ( '' )  );
#11054 = CARTESIAN_POINT ( 'NONE',  ( 18.00000000000000000, 247.7312500012290570, -5.196152422706630247 ) ) ;
#11055 = VERTEX_POINT ( 'NONE', #35990 ) ;
#11056 = CARTESIAN_POINT ( 'NONE',  ( 13.23911966647218996, 7.247686282101430066, -8.632099005475504683 ) ) ;
#11057 = CARTESIAN_POINT ( 'NONE',  ( 27.24356964375000345, 195.0781250006145342, -3.336375036156643733E-15 ) ) ;
#11058 = CARTESIAN_POINT ( 'NONE',  ( -27.24356964375000345, 198.5093750006145399, 0.000000000000000000 ) ) ;
#11059 = CARTESIAN_POINT ( 'NONE',  ( 0.000000000000000000, 2.000000000000000000, 0.000000000000000000 ) ) ;
#11060 = CARTESIAN_POINT ( 'NONE',  ( 28.27727295472088542, 5.196152422706630247, 167.6007502309489041 ) ) ;
#11061 = CARTESIAN_POINT ( 'NONE',  ( 20.99999999999999645, 185.0294372515228645, -5.999999999999999112 ) ) ;
#11062 = CARTESIAN_POINT ( 'NONE',  ( 27.00000000000000355, 196.2875000012290343, -3.306546357697854128E-15 ) ) ;
#11063 = ADVANCED_FACE ( 'NONE', ( #3963 ), #1305, .F. ) ;
#11064 = CARTESIAN_POINT ( 'NONE',  ( 23.87821517812499650, 248.3593750006145342, -4.985214923628404904 ) ) ;
#11065 = CARTESIAN_POINT ( 'NONE',  ( 8.843639120294245259, 112.8648137178985564, 3.474262827703527901 ) ) ;
#11066 = CARTESIAN_POINT ( 'NONE',  ( 20.99999999999999645, 242.7718750006145854, 6.646953231504538984 ) ) ;
#11067 = ORIENTED_EDGE ( 'NONE', *, *, #15675, .F. ) ;
#11068 = DIRECTION ( 'NONE',  ( 1.000000000000000000, 0.000000000000000000, 2.057406622567553516E-16 ) ) ;
#11069 = CARTESIAN_POINT ( 'NONE',  ( -4.694659320240884604E-14, 197.0750000012290570, 27.00000000000000000 ) ) ;
#11070 = CARTESIAN_POINT ( 'NONE',  ( 15.00000000000000000, 248.6687500012290286, -3.464101615137752166 ) ) ;
#11071 = CARTESIAN_POINT ( 'NONE',  ( 4.622313124798831829, 110.5648137178985593, -11.61527771782809282 ) ) ;
#11072 = CARTESIAN_POINT ( 'NONE',  ( 19.68408634441910721, -5.407089921784855591, -9.890624999385533300 ) ) ;
#11073 = CARTESIAN_POINT ( 'NONE',  ( 33.90267027097563357, -5.407089921784855591, 161.6597321816656176 ) ) ;
#11074 = LINE ( 'NONE', #13928, #25639 ) ;
#11075 = CARTESIAN_POINT ( 'NONE',  ( 13.49999999999999645, 196.2500000000000000, -23.38268590217984766 ) ) ;
#11076 = AXIS2_PLACEMENT_3D ( 'NONE', #33553, #2453, #16876 ) ;
#11077 = EDGE_LOOP ( 'NONE', ( #2715, #27117, #21100, #11131 ) ) ;
#11078 = VERTEX_POINT ( 'NONE', #12873 ) ;
#11079 = EDGE_LOOP ( 'NONE', ( #11289, #14101 ) ) ;
#11080 = CARTESIAN_POINT ( 'NONE',  ( 21.00000000000000000, 6.928203230275506996, -4.106249998770976184 ) ) ;
#11081 = CARTESIAN_POINT ( 'NONE',  ( 18.12178482187499640, 4.985214923628404904, -2.915624999385468819 ) ) ;
#11082 = CARTESIAN_POINT ( 'NONE',  ( -77.00000000000002842, 210.0000000000000000, -5.000000000000001776 ) ) ;
#11083 = CARTESIAN_POINT ( 'NONE',  ( 37.37375885156122024, -3.464101615137610057, 168.3106405921332680 ) ) ;
#11084 = CARTESIAN_POINT ( 'NONE',  ( 18.12178482187499640, 4.985214923628404904, -10.11562499938548143 ) ) ;
#11085 = CARTESIAN_POINT ( 'NONE',  ( 6.932735513423970097, 55.54768628210144499, 10.69584247140445044 ) ) ;
#11086 = ADVANCED_FACE ( 'NONE', ( #36357 ), #10025, .F. ) ;
#11087 = EDGE_CURVE ( 'NONE', #28262, #26234, #30692, .T. ) ;
#11088 = CARTESIAN_POINT ( 'NONE',  ( -66.81919563604517975, 216.5000000000000000, -0.1155267958017906493 ) ) ;
#11089 = CARTESIAN_POINT ( 'NONE',  ( 15.00964601948014732, 225.9742772813838769, -0.3926987779609585338 ) ) ;
#11090 = CARTESIAN_POINT ( 'NONE',  ( -36.53794563604517265, 206.7903428501025758, 3.378800118222471838 ) ) ;
#11091 = CARTESIAN_POINT ( 'NONE',  ( 1.069080835302379631E-14, 196.9624999999999773, 27.00000000000000000 ) ) ;
#11092 = STYLED_ITEM ( 'NONE', ( #2132 ), #27327 ) ;
#11093 = CARTESIAN_POINT ( 'NONE',  ( 25.02068495149662297, 0.000000000000000000, 164.7989187625597367 ) ) ;
#11094 = CARTESIAN_POINT ( 'NONE',  ( 8.962234695871567070, 113.4398137178985593, 8.715434833792127023 ) ) ;
#11095 = CARTESIAN_POINT ( 'NONE',  ( -34.56622103062155560, 211.6261429550005744, 6.530955311639227823 ) ) ;
#11096 = CARTESIAN_POINT ( 'NONE',  ( -50.59747103062156981, 214.3500491399821044, -7.303452534266878793 ) ) ;
#11097 = EDGE_CURVE ( 'NONE', #941, #9824, #31740, .T. ) ;
#11098 = CARTESIAN_POINT ( 'NONE',  ( 23.87821517812500005, -4.985214923628404016, -5.053124999385483207 ) ) ;
#11099 = CARTESIAN_POINT ( 'NONE',  ( -13.62178482187500528, 195.2281250006145399, -23.59362340125807123 ) ) ;
#11100 = CARTESIAN_POINT ( 'NONE',  ( 13.23911966647199812, 103.9523137178985763, 8.632099005475788900 ) ) ;
#11101 = CARTESIAN_POINT ( 'NONE',  ( -35.74627896937850124, 203.4690446883607535, -1.626142955000504209 ) ) ;
#11102 = ORIENTED_EDGE ( 'NONE', *, *, #16190, .F. ) ;
#11103 = CARTESIAN_POINT ( 'NONE',  ( -80.75120197997713944, 224.5663476446710831, 7.500000000000000000 ) ) ;
#11104 = CARTESIAN_POINT ( 'NONE',  ( 4.622313124798573369, 120.2351862821014663, 11.61527771782819940 ) ) ;
#11105 = CARTESIAN_POINT ( 'NONE',  ( 6.092822981423978490, 70.78518628210143504, -14.25334919248782306 ) ) ;
#11106 = CARTESIAN_POINT ( 'NONE',  ( 22.56230152254500965, -3.464101615137234358, -0.7124999999999952482 ) ) ;
#11107 = CARTESIAN_POINT ( 'NONE',  ( 37.13187018199665346, 7.646167579472024665E-16, 162.7511921998298590 ) ) ;
#11108 = CARTESIAN_POINT ( 'NONE',  ( -8.632099005475501130, 78.54768628210145209, -13.23911966647218996 ) ) ;
#11109 = CARTESIAN_POINT ( 'NONE',  ( 16.56230152254411081, -7.209453229046475009, -5.878124999385531346 ) ) ;
#11110 = CARTESIAN_POINT ( 'NONE',  ( 2.064181346179272847, 24.49768628210144072, -9.465287035748065847 ) ) ;
#11111 = LINE ( 'NONE', #17178, #1931 ) ;
#11112 = CARTESIAN_POINT ( 'NONE',  ( -61.87872103062154849, 203.4690446883607535, 1.626142955000567936 ) ) ;
#11113 = CARTESIAN_POINT ( 'NONE',  ( 12.50000000000000355, 54.11018628210144499, 0.1745138560725507937 ) ) ;
#11114 = CARTESIAN_POINT ( 'NONE',  ( -26.99999999999998934, 197.3375000000000057, 15.58845726811991561 ) ) ;
#11115 = CARTESIAN_POINT ( 'NONE',  ( -29.50000000000000711, 237.0000000000000000, -2.499999999999994671 ) ) ;
#11117 = CARTESIAN_POINT ( 'NONE',  ( 19.68408634441910721, 5.407089921784862696, -2.596874999385518024 ) ) ;
#11116 = CARTESIAN_POINT ( 'NONE',  ( -9.534712964251941258, 21.62268628210143717, 1.715153634034234154 ) ) ;
#11118 = CARTESIAN_POINT ( 'NONE',  ( 23.87821517812499650, 249.7093750006145285, -4.985214923628404904 ) ) ;
#11119 = ORIENTED_EDGE ( 'NONE', *, *, #17590, .T. ) ;
#11120 = CARTESIAN_POINT ( 'NONE',  ( 18.00000000000000355, -5.196152422706632912, -3.525000000000000355 ) ) ;
#11121 = MECHANICAL_DESIGN_GEOMETRIC_PRESENTATION_REPRESENTATION (  '', ( #16564 ), #32292 ) ;
#11122 = DIRECTION ( 'NONE',  ( 0.08715574274765150453, 0.000000000000000000, 0.9961946980917461003 ) ) ;
#11123 = CARTESIAN_POINT ( 'NONE',  ( 27.61912665782109499, 5.407089921784862696, 161.4754277583837734 ) ) ;
#11124 = CARTESIAN_POINT ( 'NONE',  ( 10.31873187879411091, 3.604726614523236616, -1.078124999385534410 ) ) ;
#11125 = CARTESIAN_POINT ( 'NONE',  ( 28.25155051613373658, 5.407089921784856479, 168.7040655364119743 ) ) ;
#11126 = CARTESIAN_POINT ( 'NONE',  ( 26.99999999999999645, 243.0249999999999773, -7.347880794884117764E-16 ) ) ;
#11127 = CARTESIAN_POINT ( 'NONE',  ( -7.234628195640289583, 198.5575961894323029, -27.00000000000001421 ) ) ;
#11128 = VECTOR ( 'NONE', #12791, 1000.000000000000000 ) ;
#11129 = CARTESIAN_POINT ( 'NONE',  ( -8.962234695871760692, 66.76018628210145778, 8.715434833791933400 ) ) ;
#11130 = ORIENTED_EDGE ( 'NONE', *, *, #4037, .T. ) ;
#11131 = ORIENTED_EDGE ( 'NONE', *, *, #16784, .T. ) ;
#11132 = CARTESIAN_POINT ( 'NONE',  ( 13.50000000000001421, 194.8625000012290513, 23.38268590217984055 ) ) ;
#11133 = CARTESIAN_POINT ( 'NONE',  ( 27.76741185964712244, 5.196152422706630247, 161.7730112471121799 ) ) ;
#11134 = CARTESIAN_POINT ( 'NONE',  ( -8.632099005475794229, 41.85231371789854649, 13.23911966647199812 ) ) ;
#11135 = EDGE_CURVE ( 'NONE', #15372, #33833, #6232, .T. ) ;
#11136 = CARTESIAN_POINT ( 'NONE',  ( 15.24356964375000167, -3.323476615752272600, -7.865624999385466332 ) ) ;
#11137 = CARTESIAN_POINT ( 'NONE',  ( 18.12178482187500350, 241.8343750006145285, 4.985214923628407568 ) ) ;
#11138 = CARTESIAN_POINT ( 'NONE',  ( -48.42038769728824832, 208.6787018382581778, 4.469044688360752637 ) ) ;
#11139 = CARTESIAN_POINT ( 'NONE',  ( 37.34761212884377812, 7.347880794884117764E-16, 168.0117821839301087 ) ) ;
#11140 = CARTESIAN_POINT ( 'NONE',  ( 27.65834674205753529, 5.407089921784862696, 161.9237153725250664 ) ) ;
#11141 = CARTESIAN_POINT ( 'NONE',  ( -6.594114490232462877, 32.93981371789854506, 6.840914352311949109 ) ) ;
#11142 = CARTESIAN_POINT ( 'NONE',  ( 25.12854018303972126, 0.000000000000000000, 166.0317097002238995 ) ) ;
#11143 = CARTESIAN_POINT ( 'NONE',  ( 1.715153634034445762, 91.87731371789854506, -9.534712964251895073 ) ) ;
#11144 = CARTESIAN_POINT ( 'NONE',  ( -13.62178482187500528, 197.5343750006145456, -23.59362340125807123 ) ) ;
#11145 = VECTOR ( 'NONE', #1603, 1000.000000000000000 ) ;
#11146 = CARTESIAN_POINT ( 'NONE',  ( 6.092822981423662299, 141.6148137178985849, 14.25334919248795096 ) ) ;
#11147 = VECTOR ( 'NONE', #22284, 1000.000000000000000 ) ;
#11148 = CARTESIAN_POINT ( 'NONE',  ( -12.53471296425194836, 67.62268628210145494, 2.311890736173176641 ) ) ;
#11149 = CARTESIAN_POINT ( 'NONE',  ( 10.56230152254410903, 0.000000000000000000, -9.787499998771043153 ) ) ;
#11150 = VECTOR ( 'NONE', #3106, 1000.000000000000000 ) ;
#11151 = DIRECTION ( 'NONE',  ( 1.000000000000000000, 0.000000000000000000, 0.000000000000000000 ) ) ;
#11152 = CARTESIAN_POINT ( 'NONE',  ( 33.71964321120555752, 5.407089921784857367, 159.5677233156729642 ) ) ;
#11153 = CARTESIAN_POINT ( 'NONE',  ( 31.18414854017020232, 6.928203230275506996, 166.4053504732449369 ) ) ;
#11154 = CARTESIAN_POINT ( 'NONE',  ( 13.44051670066911264, -5.407089921784865361, -8.221874999385537564 ) ) ;
#11155 = LINE ( 'NONE', #11706, #30639 ) ;
#11156 = CARTESIAN_POINT ( 'NONE',  ( -3.796722387233375073, 84.58518628210146062, 8.710071997420127943 ) ) ;
#11157 = CYLINDRICAL_SURFACE ( 'NONE', #22531, 2.649999999999999467 ) ;
#11158 = CARTESIAN_POINT ( 'NONE',  ( -6.932735513423968321, 106.1476862821014606, -10.69584247140445221 ) ) ;
#11159 = CARTESIAN_POINT ( 'NONE',  ( 7.234628195640363302, 195.0299038117966575, -26.99999999999996803 ) ) ;
#11160 = CARTESIAN_POINT ( 'NONE',  ( 26.99999999999999645, 248.4812500012290570, -7.347880794884117764E-16 ) ) ;
#11161 = ORIENTED_EDGE ( 'NONE', *, *, #34486, .F. ) ;
#11162 = CARTESIAN_POINT ( 'NONE',  ( 33.90267027097563357, -5.407089921784855591, 161.6597321816656176 ) ) ;
#11163 = CARTESIAN_POINT ( 'NONE',  ( 26.75643035624999655, 3.323476615752271712, -7.078124999385466687 ) ) ;
#11164 = CARTESIAN_POINT ( 'NONE',  ( -4.500000000000001776, 227.8255434699758837, 2.500000000000000000 ) ) ;
#11165 = CARTESIAN_POINT ( 'NONE',  ( 37.40967911200478824, 3.604726614523243278, 165.9265627999972992 ) ) ;
#11166 = CARTESIAN_POINT ( 'NONE',  ( 31.15473347688575956, -6.928203230275514990, 166.0691347614145741 ) ) ;
#11167 = CARTESIAN_POINT ( 'NONE',  ( 10.56230152254405574, 3.464101615137725521, -4.087500000000053646 ) ) ;
#11168 = CARTESIAN_POINT ( 'NONE',  ( 18.12178482187499640, 241.6843750006145513, -4.985214923628404904 ) ) ;
#11169 = CARTESIAN_POINT ( 'NONE',  ( 27.24356964375000700, 199.5406250006145967, 15.72908226750537075 ) ) ;
#11170 = CARTESIAN_POINT ( 'NONE',  ( -2.311890736173448424, 124.0773137178985621, 12.53471296425189330 ) ) ;
#11171 = CARTESIAN_POINT ( 'NONE',  ( -4.944772684328673229, 139.7851862821014493, 11.48171059495397728 ) ) ;
#11173 = ORIENTED_EDGE ( 'NONE', *, *, #19236, .F. ) ;
#11172 = ORIENTED_EDGE ( 'NONE', *, *, #7834, .T. ) ;
#11174 = CARTESIAN_POINT ( 'NONE',  ( 23.87821517812499650, 241.0468750006145058, -4.985214923628404904 ) ) ;
#11175 = CARTESIAN_POINT ( 'NONE',  ( -12.46528703574811558, 15.40231371789854720, 2.660918448318004170 ) ) ;
#11176 = CARTESIAN_POINT ( 'NONE',  ( -13.04141134922778456, 97.62731371789854506, 8.927990412390377273 ) ) ;
#11177 = CARTESIAN_POINT ( 'NONE',  ( 2.660918448318279950, 98.09768628210146346, -12.46528703574805697 ) ) ;
#11178 = CARTESIAN_POINT ( 'NONE',  ( 15.24356964375000167, -3.323476615752272600, -2.465624999385486404 ) ) ;
#11179 = CARTESIAN_POINT ( 'NONE',  ( 22.80587116629412137, 7.646167579472024665E-16, -8.971874999385509142 ) ) ;
#11180 = CARTESIAN_POINT ( 'NONE',  ( 26.99999999999999645, 198.5750000012290286, -15.58845726811990495 ) ) ;
#11181 = CARTESIAN_POINT ( 'NONE',  ( -0.1745138560725500443, 120.8101862821014691, 12.50000000000000355 ) ) ;
#11182 = CARTESIAN_POINT ( 'NONE',  ( 19.68408634441910721, -5.407089921784855591, -3.140624999385555061 ) ) ;
#11183 = CARTESIAN_POINT ( 'NONE',  ( -38.31919563604515844, 218.5000000000000000, -0.1155267958018185298 ) ) ;
#11184 = CARTESIAN_POINT ( 'NONE',  ( 26.75643035624999655, 243.2593750006145115, -3.323476615752271268 ) ) ;
#11185 = CARTESIAN_POINT ( 'NONE',  ( -37.72544563604516554, 213.3788001182224718, 3.209657149897419348 ) ) ;
#11186 = CARTESIAN_POINT ( 'NONE',  ( 2.311890736173175753, 120.5226862821014606, 12.53471296425194836 ) ) ;
#11187 = CARTESIAN_POINT ( 'NONE',  ( 10.56230152254411436, -3.464101615137757051, -3.449999998771012599 ) ) ;
#11188 = CARTESIAN_POINT ( 'NONE',  ( -49.21205436395490551, 214.6737587650352168, 4.842901733360204908 ) ) ;
#11189 = FACE_OUTER_BOUND ( 'NONE', #8545, .T. ) ;
#11190 = DIRECTION ( 'NONE',  ( -1.000000000000000000, 0.000000000000000000, -0.000000000000000000 ) ) ;
#11191 = CARTESIAN_POINT ( 'NONE',  ( -15.50000000000000533, 104.7101862821014606, -0.1745138560725808530 ) ) ;
#11192 = CARTESIAN_POINT ( 'NONE',  ( -10.69584247140444866, 11.84768628210144925, 6.932735513423972762 ) ) ;
#11194 = CARTESIAN_POINT ( 'NONE',  ( 19.39230484541326049, 241.4138461906613884, -5.999999999999997335 ) ) ;
#11193 = AXIS2_PLACEMENT_3D ( 'NONE', #8151, #19533, #9729 ) ;
#11195 = CARTESIAN_POINT ( 'NONE',  ( -6.594114490232312775, 133.4601862821014606, -6.840914352312096547 ) ) ;
#11196 = ADVANCED_FACE ( 'NONE', ( #8132 ), #37102, .F. ) ;
#11197 = CARTESIAN_POINT ( 'NONE',  ( 19.68408634441911076, -5.407089921784855591, -1.340624999385559013 ) ) ;
#11198 = DIRECTION ( 'NONE',  ( 0.000000000000000000, 0.000000000000000000, 1.000000000000000000 ) ) ;
#11199 = ORIENTED_EDGE ( 'NONE', *, *, #23085, .T. ) ;
#11200 = CARTESIAN_POINT ( 'NONE',  ( 25.18740179294109183, 0.000000000000000000, 169.4991492277590339 ) ) ;
#11201 = CARTESIAN_POINT ( 'NONE',  ( 9.534712964251941258, 63.02268628210144641, -1.715153634034235708 ) ) ;
#11202 = FACE_OUTER_BOUND ( 'NONE', #622, .T. ) ;
#11203 = CARTESIAN_POINT ( 'NONE',  ( 23.99999999999999645, 241.3000000000000114, -5.196152422706631135 ) ) ;
#11204 = CARTESIAN_POINT ( 'NONE',  ( 2.999999999999997335, 252.0000000000000000, -5.000000000000000000 ) ) ;
#11205 = CARTESIAN_POINT ( 'NONE',  ( -27.24356964374999635, 196.7468750006145797, 15.72908226750539384 ) ) ;
#11206 = CARTESIAN_POINT ( 'NONE',  ( 26.99999999999999645, 246.1750000000000114, -7.347880794884117764E-16 ) ) ;
#11207 = DIRECTION ( 'NONE',  ( 0.000000000000000000, -1.000000000000000000, 0.000000000000000000 ) ) ;
#11208 = CARTESIAN_POINT ( 'NONE',  ( -3.474262827703527901, 32.36481371789854933, 8.843639120294245259 ) ) ;
#11209 = CARTESIAN_POINT ( 'NONE',  ( 15.00000000000000178, -3.464101615137757051, -9.412499999999978328 ) ) ;
#11210 = EDGE_LOOP ( 'NONE', ( #8462, #32222, #13790, #13367 ) ) ;
#11211 =( BOUNDED_CURVE ( )  B_SPLINE_CURVE ( 2, ( #11701, #8313, #34453, #31427, #31607, #25736, #22906, #20249, #23088 ),
 .UNSPECIFIED., .F., .F. ) 
 B_SPLINE_CURVE_WITH_KNOTS ( ( 3, 2, 2, 2, 3 ),
 ( 0.9021739130434782705, 0.9057971014492753881, 0.9130434782608695121, 0.9202898550724637472, 0.9239130434782608647 ),
 .UNSPECIFIED. ) 
 CURVE ( )  GEOMETRIC_REPRESENTATION_ITEM ( )  RATIONAL_B_SPLINE_CURVE ( ( 0.9330127018922194093, 0.9330127018922194093, 1.000000000000000000, 0.8660254037844387076, 1.000000000000000000, 0.8660254037844387076, 1.000000000000000000, 0.9330127018922194093, 0.9330127018922194093 ) ) 
 REPRESENTATION_ITEM ( '' )  );
#11212 = CARTESIAN_POINT ( 'NONE',  ( 15.00000000000000000, 240.6062500012290286, 0.000000000000000000 ) ) ;
#11213 = CARTESIAN_POINT ( 'NONE',  ( 6.932735513424201024, 55.65231371789855785, -10.69584247140429412 ) ) ;
#11214 = CARTESIAN_POINT ( 'NONE',  ( 10.31873187879410736, -3.604726614523244610, -8.259374999385515892 ) ) ;
#11215 = CARTESIAN_POINT ( 'NONE',  ( 23.87821517812499650, 4.985214923628404904, -9.853124999385482141 ) ) ;
#11216 = CARTESIAN_POINT ( 'NONE',  ( 10.69584247140429589, 21.15231371789855430, 6.932735513424201024 ) ) ;
#11217 = EDGE_CURVE ( 'NONE', #22420, #32427, #6581, .T. ) ;
#11218 = ORIENTED_EDGE ( 'NONE', *, *, #28378, .F. ) ;
#11219 = CARTESIAN_POINT ( 'NONE',  ( 22.80587116629411781, 7.646167579472024665E-16, -1.321874999385519445 ) ) ;
#11220 = CARTESIAN_POINT ( 'NONE',  ( 8.962234695871762469, 6.960186282101432198, -8.715434833791931624 ) ) ;
#11221 = CARTESIAN_POINT ( 'NONE',  ( 24.90469035240339934, 3.604726614523240613, 166.2677426758239108 ) ) ;
#11222 = EDGE_CURVE ( 'NONE', #4778, #13411, #32608, .T. ) ;
#11223 = VECTOR ( 'NONE', #3788, 1000.000000000000000 ) ;
#11224 = CARTESIAN_POINT ( 'NONE',  ( -38.71502896937850124, 215.5714017266979567, -3.350049139982168800 ) ) ;
#11225 = CARTESIAN_POINT ( 'NONE',  ( 10.56230152254410903, 3.464101615137752610, -0.3749999987710042615 ) ) ;
#11226 = CARTESIAN_POINT ( 'NONE',  ( 15.00000000000000000, 0.000000000000000000, -6.243749998770947940 ) ) ;
#11227 = CARTESIAN_POINT ( 'NONE',  ( -33.37872103062156981, 205.4690446883607535, 1.090244570138264368 ) ) ;
#11228 = CARTESIAN_POINT ( 'NONE',  ( -50.39955436395490551, 214.8429017333601792, -4.673758765035196383 ) ) ;
#11229 = CARTESIAN_POINT ( 'NONE',  ( 34.54326498017087488, 5.407089921784857367, 168.9817632126399758 ) ) ;
#11230 = ORIENTED_EDGE ( 'NONE', *, *, #4506, .F. ) ;
#11231 = DIRECTION ( 'NONE',  ( 0.08715574274765150453, 0.000000000000000000, 0.9961946980917461003 ) ) ;
#11232 = DIRECTION ( 'NONE',  ( 0.000000000000000000, 0.000000000000000000, 1.000000000000000000 ) ) ;
#11233 = CARTESIAN_POINT ( 'NONE',  ( 6.092822981423662299, 22.01481371789855501, 14.25334919248795096 ) ) ;
#11234 = CARTESIAN_POINT ( 'NONE',  ( -37.72544563604516554, 216.3070033484980854, 6.137860380172893926 ) ) ;
#11235 = CARTESIAN_POINT ( 'NONE',  ( 4.622313124798573369, 9.835186282101449962, 11.61527771782819940 ) ) ;
#11236 = CARTESIAN_POINT ( 'NONE',  ( -2.660918448318275509, 56.69768628210145067, 12.46528703574805874 ) ) ;
#11237 = CARTESIAN_POINT ( 'NONE',  ( 16.56230152254411436, -6.928203230275514990, -5.737500000000049560 ) ) ;
#11238 = FACE_BOUND ( 'NONE', #18843, .T. ) ;
#11239 = EDGE_LOOP ( 'NONE', ( #3223, #33454, #26638, #2949 ) ) ;
#11240 = CARTESIAN_POINT ( 'NONE',  ( 15.50000000000000533, 17.31018628210144428, 0.1745138560725827404 ) ) ;
#11241 = LINE ( 'NONE', #13346, #29024 ) ;
#11242 = EDGE_CURVE ( 'NONE', #16861, #25852, #35610, .T. ) ;
#11243 = CARTESIAN_POINT ( 'NONE',  ( -1.926257025242585782E-15, 197.4968750006145513, -31.45816453501075927 ) ) ;
#11244 = CARTESIAN_POINT ( 'NONE',  ( -13.50000000000000533, 199.0250000000000057, -23.38268590217984411 ) ) ;
#11245 = CARTESIAN_POINT ( 'NONE',  ( 15.24356964374999990, 0.000000000000000000, -0.2531249993854844949 ) ) ;
#11246 = CARTESIAN_POINT ( 'NONE',  ( 1.120210788295102201E-13, 195.8375000000000057, -27.00000000000000711 ) ) ;
#11247 = CYLINDRICAL_SURFACE ( 'NONE', #32675, 27.00000000000000000 ) ;
#11248 = VECTOR ( 'NONE', #5875, 1000.000000000000000 ) ;
#11249 = APPLICATION_CONTEXT ( 'automotive_design' ) ;
#11250 = CARTESIAN_POINT ( 'NONE',  ( 23.87821517812499650, 244.3093750006145228, -4.985214923628404904 ) ) ;
#11251 = CARTESIAN_POINT ( 'NONE',  ( -2.064181346179062349, 118.9023137178985650, -9.465287035748106703 ) ) ;
#11252 = CARTESIAN_POINT ( 'NONE',  ( 26.75643035624999655, 241.1218750006145228, -3.323476615752271268 ) ) ;
#11253 = ORIENTED_EDGE ( 'NONE', *, *, #6629, .F. ) ;
#11254 = CARTESIAN_POINT ( 'NONE',  ( -69.99330436395490551, 210.1155267958017134, -6.500000000000000888 ) ) ;
#11255 = CARTESIAN_POINT ( 'NONE',  ( -13.50000000000000533, 195.8750000000000284, -23.38268590217984411 ) ) ;
#11256 = CARTESIAN_POINT ( 'NONE',  ( 24.00000000000000000, 248.8562500012290570, 5.196152422706629359 ) ) ;
#11257 = EDGE_LOOP ( 'NONE', ( #6678, #84, #2808, #28550 ) ) ;
#11258 = CARTESIAN_POINT ( 'NONE',  ( 8.962234695871567070, 122.6398137178985621, 8.715434833792127023 ) ) ;
#11259 = ADVANCED_FACE ( 'NONE', ( #4895 ), #16850, .T. ) ;
#11260 = CARTESIAN_POINT ( 'NONE',  ( 19.68408634441910721, -5.407089921784855591, -8.540624999385542537 ) ) ;
#11261 = CARTESIAN_POINT ( 'NONE',  ( 24.56314878551103575, -3.604726614523240613, 162.3639047026768765 ) ) ;
#11262 =( BOUNDED_CURVE ( )  B_SPLINE_CURVE ( 2, ( #32450, #28852, #3077, #17128, #26196, #14277, #2886, #14838, #11428 ),
 .UNSPECIFIED., .F., .F. ) 
 B_SPLINE_CURVE_WITH_KNOTS ( ( 3, 2, 2, 2, 3 ),
 ( 0.8541666666666667407, 0.8611111111111111605, 0.8750000000000000000, 0.8888888888888888395, 0.8958333333333333703 ),
 .UNSPECIFIED. ) 
 CURVE ( )  GEOMETRIC_REPRESENTATION_ITEM ( )  RATIONAL_B_SPLINE_CURVE ( ( 0.9330127018922192983, 0.9330127018922198534, 1.000000000000000000, 0.8660254037844387076, 1.000000000000000000, 0.8660254037844387076, 1.000000000000000000, 0.9330127018922187432, 0.9330127018922192983 ) ) 
 REPRESENTATION_ITEM ( '' )  );
#11263 = CYLINDRICAL_SURFACE ( 'NONE', #8108, 5.999999999999994671 ) ;
#11264 = CARTESIAN_POINT ( 'NONE',  ( 27.00000000000000355, 196.1750000000000114, -3.306546357697854128E-15 ) ) ;
#11265 = ORIENTED_EDGE ( 'NONE', *, *, #34880, .T. ) ;
#11266 = ORIENTED_EDGE ( 'NONE', *, *, #746, .T. ) ;
#11267 = ORIENTED_EDGE ( 'NONE', *, *, #26246, .F. ) ;
#11268 = CARTESIAN_POINT ( 'NONE',  ( 24.00000000000000000, -5.196152422706629359, -6.543749998770942433 ) ) ;
#11269 = CARTESIAN_POINT ( 'NONE',  ( 23.87821517812499650, 4.985214923628404904, -1.640624999385470462 ) ) ;
#11270 = CARTESIAN_POINT ( 'NONE',  ( 24.62848410913218800, 0.000000000000000000, 160.3160426211468348 ) ) ;
#11271 = CARTESIAN_POINT ( 'NONE',  ( 34.38190641693269356, -5.196152422706635576, 168.5347505191977859 ) ) ;
#11272 = CARTESIAN_POINT ( 'NONE',  ( 23.87821517812500005, 248.9968750006145228, 4.985214923628404016 ) ) ;
#11273 = AXIS2_PLACEMENT_3D ( 'NONE', #4423, #27739, #7652 ) ;
#11274 = EDGE_CURVE ( 'NONE', #8594, #36846, #5352, .T. ) ;
#11275 = CARTESIAN_POINT ( 'NONE',  ( -11.61527771782819940, 67.33518628210144641, 4.622313124798574258 ) ) ;
#11276 = CARTESIAN_POINT ( 'NONE',  ( -64.24627896937849414, 203.4690446883607535, -1.626142955000504209 ) ) ;
#11277 = CARTESIAN_POINT ( 'NONE',  ( 14.97710761593488904, 216.0228923840610662, 0.2612666680233010630 ) ) ;
#11278 = CARTESIAN_POINT ( 'NONE',  ( -44.45461230271183695, 208.6787018382582346, -4.469044688360757966 ) ) ;
#11279 = CARTESIAN_POINT ( 'NONE',  ( 31.00765816110621031, -6.928203230275506996, 164.3880562096091182 ) ) ;
#11280 = CARTESIAN_POINT ( 'NONE',  ( -11.48171059495408208, 97.91481371789856780, 4.944772684328421875 ) ) ;
#11281 = CARTESIAN_POINT ( 'NONE',  ( -33.37872103062156981, 203.4690446883607535, 1.626142955000567936 ) ) ;
#11282 = CARTESIAN_POINT ( 'NONE',  ( -48.81622103062156981, 212.1620413398628671, 8.530955311639223382 ) ) ;
#11283 = VECTOR ( 'NONE', #24224, 1000.000000000000114 ) ;
#11284 =( BOUNDED_CURVE ( )  B_SPLINE_CURVE ( 2, ( #3068, #31325, #11045, #16931, #34719, #20338, #28473 ),
 .UNSPECIFIED., .F., .F. ) 
 B_SPLINE_CURVE_WITH_KNOTS ( ( 3, 2, 2, 3 ),
 ( 0.08695652173913158423, 0.09420289855072500051, 0.1014492753623184029, 0.1086956521739118053 ),
 .UNSPECIFIED. ) 
 CURVE ( )  GEOMETRIC_REPRESENTATION_ITEM ( )  RATIONAL_B_SPLINE_CURVE ( ( 0.9999999999999786837, 0.8660254037844600239, 1.000000000000000000, 0.8660254037844387076, 1.000000000000000000, 0.8660254037844615782, 0.9999999999999771294 ) ) 
 REPRESENTATION_ITEM ( '' )  );
#11285 = CARTESIAN_POINT ( 'NONE',  ( 26.75643035624999655, 3.323476615752271268, -4.040624999385488358 ) ) ;
#11286 = CARTESIAN_POINT ( 'NONE',  ( 15.00000000000000000, 0.000000000000000000, -1.799999999999996048 ) ) ;
#11287 = CARTESIAN_POINT ( 'NONE',  ( -14.25334919248795096, 79.51481371789856212, 6.092822981423662299 ) ) ;
#11288 = CARTESIAN_POINT ( 'NONE',  ( -35.54836230271183695, 204.3130714775002446, -3.149950860017828091 ) ) ;
#11289 = ORIENTED_EDGE ( 'NONE', *, *, #25622, .T. ) ;
#11290 = CARTESIAN_POINT ( 'NONE',  ( 23.99999999999999645, 242.2562500012290627, -5.196152422706631135 ) ) ;
#11291 = CARTESIAN_POINT ( 'NONE',  ( -7.228626920339069173, 112.4726862821014493, 10.49813415415989581 ) ) ;
#11292 = CARTESIAN_POINT ( 'NONE',  ( -3.257655550457281723, 65.89768628210143220, 15.46528703574804986 ) ) ;
#11293 = CARTESIAN_POINT ( 'NONE',  ( -54.50000000000000711, 237.0000000000000000, -2.500000000000000000 ) ) ;
#11294 = CARTESIAN_POINT ( 'NONE',  ( 27.78908035617901717, -5.407089921784865361, 163.4180074196626720 ) ) ;
#11295 = CARTESIAN_POINT ( 'NONE',  ( 11.08355503943142750, 62.16018628210144925, -10.83675517735155225 ) ) ;
#11296 = ADVANCED_FACE ( 'NONE', ( #31428 ), #5449, .T. ) ;
#11297 = CARTESIAN_POINT ( 'NONE',  ( 16.56230152254411081, 7.209453229046475009, -7.453124999385500438 ) ) ;
#11298 = CARTESIAN_POINT ( 'NONE',  ( 20.99999999999999645, 185.0294372515228645, 0.000000000000000000 ) ) ;
#11299 = CARTESIAN_POINT ( 'NONE',  ( -57.32663769728823411, 204.3130714775002730, 3.149950860017883603 ) ) ;
#11300 = CARTESIAN_POINT ( 'NONE',  ( 21.00000000000000000, 243.4187500012290002, 5.999999999999998224 ) ) ;
#11301 = CARTESIAN_POINT ( 'NONE',  ( -12.50000000000000355, 31.11018628210143788, -0.1745138560725492671 ) ) ;
#11302 = CARTESIAN_POINT ( 'NONE',  ( -27.00000000000000355, 197.7500000000000000, 0.000000000000000000 ) ) ;
#11303 = CARTESIAN_POINT ( 'NONE',  ( 15.00000000000000355, 7.347880794884112834E-16, -8.000000000000000000 ) ) ;
#11304 = CARTESIAN_POINT ( 'NONE',  ( -0.1745138560725182642, 19.61018628210144144, 9.500000000000005329 ) ) ;
#11305 = CARTESIAN_POINT ( 'NONE',  ( 20.99999999999999645, 249.7468750006145797, -6.646953231504538984 ) ) ;
#11306 = ORIENTED_EDGE ( 'NONE', *, *, #27014, .F. ) ;
#11307 = CARTESIAN_POINT ( 'NONE',  ( 15.00000000000000000, 3.464101615137752166, -4.537499999999986322 ) ) ;
#11308 = DIRECTION ( 'NONE',  ( -1.000000000000000000, 0.000000000000000000, 1.636531581110199847E-16 ) ) ;
#11309 = CARTESIAN_POINT ( 'NONE',  ( 36.81810950810510974, 7.646167579472024665E-16, 159.1648912866995715 ) ) ;
#11310 = CARTESIAN_POINT ( 'NONE',  ( 19.68408634441910721, -5.407089921784855591, -2.690624999385549110 ) ) ;
#11311 = CARTESIAN_POINT ( 'NONE',  ( 28.21233043189729273, 5.407089921784856479, 168.2557779222707097 ) ) ;
#11312 = CARTESIAN_POINT ( 'NONE',  ( 15.00000000000000178, 242.8375000000000057, 3.464101615137757051 ) ) ;
#11313 = CARTESIAN_POINT ( 'NONE',  ( -26.99999999999999645, 198.6875000000000284, 15.58845726811991561 ) ) ;
#11314 = CARTESIAN_POINT ( 'NONE',  ( -6.932735513423968321, 69.34768628210144925, -10.69584247140445221 ) ) ;
#11315 = ORIENTED_EDGE ( 'NONE', *, *, #6818, .F. ) ;
#11316 = ORIENTED_EDGE ( 'NONE', *, *, #25932, .F. ) ;
#11317 = CARTESIAN_POINT ( 'NONE',  ( 38.04237167757726468, 114.1383727779939647, -0.4999999999999965583 ) ) ;
#11318 = CARTESIAN_POINT ( 'NONE',  ( -26.99999999999998934, 197.0000000012290400, 15.58845726811991561 ) ) ;
#11319 = CARTESIAN_POINT ( 'NONE',  ( 0.000000000000000000, 200.0000000000000000, 0.000000000000000000 ) ) ;
#11320 = CARTESIAN_POINT ( 'NONE',  ( 15.50000000000000533, 38.68981371789855217, -0.1745138560722452326 ) ) ;
#11321 = CARTESIAN_POINT ( 'NONE',  ( 26.75643035624999655, 3.323476615752271712, -8.090624999385481075 ) ) ;
#11322 = CARTESIAN_POINT ( 'NONE',  ( 15.24356964374999990, 243.5218750006145569, -3.323476615752268604 ) ) ;
#11323 = CARTESIAN_POINT ( 'NONE',  ( -43.47247103062156981, 207.6499508600178387, 3.839350919129076445 ) ) ;
#11324 = VECTOR ( 'NONE', #21602, 1000.000000000000000 ) ;
#11325 = CARTESIAN_POINT ( 'NONE',  ( 21.00000000000000000, 242.9687500012290684, 5.999999999999998224 ) ) ;
#11326 = CARTESIAN_POINT ( 'NONE',  ( 24.55497793462844669, 0.000000000000000000, 162.2705114497308045 ) ) ;
#11327 = CARTESIAN_POINT ( 'NONE',  ( -8.152565276336593669, 16.55231371789855643, -5.233372021372610483 ) ) ;
#11328 = DIRECTION ( 'NONE',  ( -0.000000000000000000, -1.000000000000000000, -0.000000000000000000 ) ) ;
#11329 = FILL_AREA_STYLE ('',( #25730 ) ) ;
#11330 = CARTESIAN_POINT ( 'NONE',  ( 27.00344680842688661, 195.0000000000000000, -2.333320423711915392 ) ) ;
#11331 = CARTESIAN_POINT ( 'NONE',  ( 27.24356964375000700, 195.9968750006145513, 15.72908226750537075 ) ) ;
#11332 = CARTESIAN_POINT ( 'NONE',  ( 10.69584247140429589, 11.95231371789853902, 6.932735513424201024 ) ) ;
#11333 = VERTEX_POINT ( 'NONE', #28570 ) ;
#11334 = EDGE_CURVE ( 'NONE', #18637, #25480, #10939, .T. ) ;
#11335 = CARTESIAN_POINT ( 'NONE',  ( 4.944772684328679446, 61.58518628210145351, -11.48171059495397373 ) ) ;
#11336 = CARTESIAN_POINT ( 'NONE',  ( 31.30180879287953388, 6.928203230275506996, 167.7502133156687876 ) ) ;
#11337 = CYLINDRICAL_SURFACE ( 'NONE', #16283, 27.00000000000000355 ) ;
#11338 = CARTESIAN_POINT ( 'NONE',  ( 36.86223210287109708, 7.646167579472015790E-16, 159.6692148526084907 ) ) ;
#11339 = CARTESIAN_POINT ( 'NONE',  ( 15.00000000000000000, 0.000000000000000000, -3.543749998770939769 ) ) ;
#11340 = CARTESIAN_POINT ( 'NONE',  ( 10.31873187879411091, 3.604726614523240613, -8.784374999385505589 ) ) ;
#11341 = SURFACE_STYLE_USAGE ( .BOTH. , #17036 ) ;
#11342 = CARTESIAN_POINT ( 'NONE',  ( -9.465287035748065847, 77.39768628210144641, -2.064181346179273735 ) ) ;
#11343 = CARTESIAN_POINT ( 'NONE',  ( 19.56230152254411081, -5.196152422706629359, -1.087499998771029874 ) ) ;
#11344 = ADVANCED_FACE ( 'NONE', ( #2239 ), #11337, .T. ) ;
#11345 = CARTESIAN_POINT ( 'NONE',  ( 6.932735513423970097, 119.9476862821014578, 10.69584247140445044 ) ) ;
#11346 = CARTESIAN_POINT ( 'NONE',  ( -27.00000000000000355, 197.3000000000000114, 0.000000000000000000 ) ) ;
#11347 = CYLINDRICAL_SURFACE ( 'NONE', #25872, 5.999999999999998224 ) ;
#11348 = ORIENTED_EDGE ( 'NONE', *, *, #4965, .T. ) ;
#11349 = CARTESIAN_POINT ( 'NONE',  ( 37.01911243981686539, 7.646167579472015790E-16, 161.4623653091736628 ) ) ;
#11350 = CARTESIAN_POINT ( 'NONE',  ( 26.75643035624999655, 7.049594010296217766E-16, -7.565624999385455851 ) ) ;
#11351 = CIRCLE ( 'NONE', #2253, 2.649999999999990585 ) ;
#11352 = CARTESIAN_POINT ( 'NONE',  ( -3.253724281355068545E-15, 196.2874999999999659, -27.00000000000000000 ) ) ;
#11353 = CARTESIAN_POINT ( 'NONE',  ( 31.25523494279520165, -7.209453229046482114, 167.2178717732638233 ) ) ;
#11354 = CARTESIAN_POINT ( 'NONE',  ( 25.12527184268668634, 3.464101615137757051, 165.9943523990454537 ) ) ;
#11355 = DIRECTION ( 'NONE',  ( 0.000000000000000000, 0.000000000000000000, 1.000000000000000000 ) ) ;
#11356 = CARTESIAN_POINT ( 'NONE',  ( 23.87821517812500005, 240.1093750006145342, 4.985214923628404016 ) ) ;
#11357 = CARTESIAN_POINT ( 'NONE',  ( 13.62178482187501416, 198.1531250006145228, 23.59362340125806767 ) ) ;
#11358 = CARTESIAN_POINT ( 'NONE',  ( -4.944772684328424539, 127.8148137178985735, -11.48171059495408031 ) ) ;
#11359 = CARTESIAN_POINT ( 'NONE',  ( 10.49813415415989581, 128.5726862821014720, 7.228626920339069173 ) ) ;
#11361 = ORIENTED_EDGE ( 'NONE', *, *, #11334, .T. ) ;
#11360 = ORIENTED_EDGE ( 'NONE', *, *, #29019, .T. ) ;
#11362 = CARTESIAN_POINT ( 'NONE',  ( 5.778771075727756162E-15, 198.1156250006145285, 31.45816453501075927 ) ) ;
#11363 = CARTESIAN_POINT ( 'NONE',  ( 23.87821517812500005, 242.6968750006145115, 4.985214923628404016 ) ) ;
#11364 = CARTESIAN_POINT ( 'NONE',  ( 10.56230152254410726, 0.000000000000000000, -3.150000000000041656 ) ) ;
#11365 = CARTESIAN_POINT ( 'NONE',  ( 10.83675517735179206, 92.73981371789854222, -11.08355503943118769 ) ) ;
#11366 = CARTESIAN_POINT ( 'NONE',  ( 7.228626920339068285, 89.47268628210144925, -10.49813415415989581 ) ) ;
#11367 = CARTESIAN_POINT ( 'NONE',  ( 23.87821517812500005, -4.985214923628404016, -1.003124999385485161 ) ) ;
#11368 = CARTESIAN_POINT ( 'NONE',  ( 26.99999999999999645, 197.2250000012290059, -15.58845726811990495 ) ) ;
#11369 = CARTESIAN_POINT ( 'NONE',  ( -4.944772684328673229, 112.1851862821014549, 11.48171059495397728 ) ) ;
#11370 = CARTESIAN_POINT ( 'NONE',  ( 10.31873187879411091, 0.000000000000000000, -2.840624999385532590 ) ) ;
#11371 = CARTESIAN_POINT ( 'NONE',  ( 15.24356964374999990, 244.7968750006145058, 0.000000000000000000 ) ) ;
#11372 = AXIS2_PLACEMENT_3D ( 'NONE', #27366, #12777, #30024 ) ;
#11373 = CARTESIAN_POINT ( 'NONE',  ( 24.00000000000000000, 246.6062500012290570, 5.196152422706629359 ) ) ;
#11374 = CARTESIAN_POINT ( 'NONE',  ( -7.228626920339069173, 112.4726862821014493, 10.49813415415989581 ) ) ;
#11375 = CARTESIAN_POINT ( 'NONE',  ( 10.56230152254411436, -3.464101615137757051, -3.899999998771008336 ) ) ;
#11376 = CARTESIAN_POINT ( 'NONE',  ( -39.31622103062156270, 211.6261429550005744, 6.530955311639227823 ) ) ;
#11377 = DIRECTION ( 'NONE',  ( -1.000000000000000000, 0.000000000000000000, -0.000000000000000000 ) ) ;
#11378 = AXIS2_PLACEMENT_3D ( 'NONE', #28816, #34512, #20119 ) ;
#11379 = CARTESIAN_POINT ( 'NONE',  ( -13.04141134922759804, 105.5726862821014294, -8.927990412390657937 ) ) ;
#11380 = CARTESIAN_POINT ( 'NONE',  ( 12.53471296425194659, 17.02268628210144996, -2.311890736173178418 ) ) ;
#11381 = CARTESIAN_POINT ( 'NONE',  ( 3.306546357697854128E-15, 0.000000000000000000, 27.00000000000000355 ) ) ;
#11382 = CARTESIAN_POINT ( 'NONE',  ( 20.99999999999999289, 241.3937500012289945, -5.999999999999997335 ) ) ;
#11383 = CARTESIAN_POINT ( 'NONE',  ( 3.474262827703335166, 138.6351862821014720, 8.843639120294326972 ) ) ;
#11384 = CARTESIAN_POINT ( 'NONE',  ( -74.35000000000002274, 210.0000000000000000, -2.499999999999998668 ) ) ;
#11385 = EDGE_LOOP ( 'NONE', ( #8265, #8645, #26661, #24287 ) ) ;
#11386 = CARTESIAN_POINT ( 'NONE',  ( 31.37779770603408380, -7.209453229046475009, 168.6187705674553285 ) ) ;
#11387 = CARTESIAN_POINT ( 'NONE',  ( 5.233372021372432847, 64.74768628210144072, 8.152565276336710909 ) ) ;
#11388 = CARTESIAN_POINT ( 'NONE',  ( 26.75643035624999655, 7.049594010296217766E-16, -0.3656249993854721048 ) ) ;
#11389 = FACE_OUTER_BOUND ( 'NONE', #8557, .T. ) ;
#11390 = DIRECTION ( 'NONE',  ( 1.000000000000000000, 0.000000000000000000, 0.000000000000000000 ) ) ;
#11391 = CARTESIAN_POINT ( 'NONE',  ( -13.62178482187500528, 195.2843750006145456, -23.59362340125807123 ) ) ;
#11392 = CARTESIAN_POINT ( 'NONE',  ( 22.60769515458672174, 246.0825961894323370, 6.000000000000004441 ) ) ;
#11393 = CARTESIAN_POINT ( 'NONE',  ( 3.306546357697853733E-15, 210.0000000000000284, 27.00000000000000000 ) ) ;
#11394 = EDGE_CURVE ( 'NONE', #24643, #483, #25737, .T. ) ;
#11395 = CARTESIAN_POINT ( 'NONE',  ( 5.529263428287300108, 30.92731371789853867, 7.954856959092309943 ) ) ;
#11396 = CARTESIAN_POINT ( 'NONE',  ( 13.62178482187499640, 199.7093750006145285, -23.59362340125807123 ) ) ;
#11397 = AXIS2_PLACEMENT_3D ( 'NONE', #23983, #3876, #15638 ) ;
#11398 = VERTEX_POINT ( 'NONE', #8496 ) ;
#11399 = VERTEX_POINT ( 'NONE', #31609 ) ;
#11400 = CARTESIAN_POINT ( 'NONE',  ( 15.24356964374999990, 248.8093750006144944, -3.323476615752268604 ) ) ;
#11401 = CARTESIAN_POINT ( 'NONE',  ( 8.715434833792128799, 37.53981371789855359, -8.962234695871567070 ) ) ;
#11402 = CARTESIAN_POINT ( 'NONE',  ( 13.44051670066911264, -5.407089921784865361, -8.221874999385537564 ) ) ;
#11403 = CARTESIAN_POINT ( 'NONE',  ( 18.12178482187499640, 4.985214923628404904, -0.2156249993854608693 ) ) ;
#11404 = CARTESIAN_POINT ( 'NONE',  ( 6.932735513424201024, 18.85231371789855714, -10.69584247140429412 ) ) ;
#11405 = ORIENTED_EDGE ( 'NONE', *, *, #30351, .T. ) ;
#11406 = AXIS2_PLACEMENT_3D ( 'NONE', #36898, #28192, #10760 ) ;
#11407 = CARTESIAN_POINT ( 'NONE',  ( 19.68408634441912142, -5.407089921784861808, -1.846874999385544891 ) ) ;
#11408 = CARTESIAN_POINT ( 'NONE',  ( 24.62848410913218800, 0.000000000000000000, 160.3160426211468348 ) ) ;
#11409 = EDGE_CURVE ( 'NONE', #5512, #25530, #29068, .T. ) ;
#11410 = CARTESIAN_POINT ( 'NONE',  ( 28.14206111430700474, -5.407089921784865361, 167.4525959469342524 ) ) ;
#11411 = EDGE_CURVE ( 'NONE', #10569, #253, #36603, .T. ) ;
#11412 = CARTESIAN_POINT ( 'NONE',  ( -37.32961230271182274, 211.8571965466040297, 6.469044688360755302 ) ) ;
#11413 = PRESENTATION_STYLE_ASSIGNMENT (( #20138 ) ) ;
#11414 = CARTESIAN_POINT ( 'NONE',  ( -20.75254460673100709, 194.9999999999999716, 17.57977308427575025 ) ) ;
#11415 = CARTESIAN_POINT ( 'NONE',  ( -57.31919563604516554, 214.5000000000000284, -0.1155267958017627827 ) ) ;
#11416 = CARTESIAN_POINT ( 'NONE',  ( -42.87872103062156981, 203.4690446883607535, 1.626142955000567936 ) ) ;
#11417 = CARTESIAN_POINT ( 'NONE',  ( 34.49097153452227360, -5.407089921784855591, 168.3840463937848995 ) ) ;
#11418 = VERTEX_POINT ( 'NONE', #20250 ) ;
#11419 = VECTOR ( 'NONE', #17967, 1000.000000000000000 ) ;
#11420 = CARTESIAN_POINT ( 'NONE',  ( -27.00000000000000355, 197.8250000012290570, -15.58845726811989429 ) ) ;
#11421 = CARTESIAN_POINT ( 'NONE',  ( 26.99999999999952038, -3.464101615138027057, -7.012500000000017941 ) ) ;
#11422 = CARTESIAN_POINT ( 'NONE',  ( 0.1745138560722461762, 13.38981371789854613, 15.50000000000000533 ) ) ;
#11423 = CARTESIAN_POINT ( 'NONE',  ( -30.99627896937850480, 201.4690446883607251, -2.162041339862721845 ) ) ;
#11424 = CARTESIAN_POINT ( 'NONE',  ( -2.660918448318275509, 10.69768628210143646, 12.46528703574805874 ) ) ;
#11425 = CARTESIAN_POINT ( 'NONE',  ( 10.69584247140445221, 53.24768628210144072, -6.932735513423970097 ) ) ;
#11426 = CARTESIAN_POINT ( 'NONE',  ( 10.56230152254410903, -3.464101615137761048, -4.462500000000024336 ) ) ;
#11427 = ORIENTED_EDGE ( 'NONE', *, *, #19120, .F. ) ;
#11428 = CARTESIAN_POINT ( 'NONE',  ( -1.045839947578415010E-13, 195.1625000000000512, 27.00000000000000355 ) ) ;
#11429 = CARTESIAN_POINT ( 'NONE',  ( -13.62178482187498396, 195.8843750006145399, 23.59362340125808188 ) ) ;
#11430 = CARTESIAN_POINT ( 'NONE',  ( 10.56230152254416588, 3.464101615137787693, -6.337500000000034106 ) ) ;
#11431 = CARTESIAN_POINT ( 'NONE',  ( 37.22014685496823461, 7.347880794884125653E-16, 166.5548474367465985 ) ) ;
#11432 = CARTESIAN_POINT ( 'NONE',  ( 36.72009078106068358, 7.347880794884117764E-16, 160.8391803576695622 ) ) ;
#11433 = EDGE_CURVE ( 'NONE', #26085, #2436, #9427, .T. ) ;
#11434 = DIRECTION ( 'NONE',  ( -1.000000000000000000, 0.000000000000000000, -0.000000000000000000 ) ) ;
#11435 = CARTESIAN_POINT ( 'NONE',  ( 18.12178482187499640, 246.1843750006145228, -4.985214923628404904 ) ) ;
#11436 = CARTESIAN_POINT ( 'NONE',  ( 5.233372021372610483, 92.45231371789854791, -8.152565276336593669 ) ) ;
#11437 = CARTESIAN_POINT ( 'NONE',  ( 26.75643035624999655, 242.9218750006145626, -3.323476615752271268 ) ) ;
#11438 = ORIENTED_EDGE ( 'NONE', *, *, #27064, .T. ) ;
#11439 = CARTESIAN_POINT ( 'NONE',  ( -50.20163769728823411, 215.6869285224996986, -3.149950860017881382 ) ) ;
#11440 = FACE_OUTER_BOUND ( 'NONE', #29567, .T. ) ;
#11441 = CARTESIAN_POINT ( 'NONE',  ( 24.00000000000000000, 245.2562500012290627, 5.196152422706629359 ) ) ;
#11442 = ORIENTED_EDGE ( 'NONE', *, *, #28150, .F. ) ;
#11443 = CARTESIAN_POINT ( 'NONE',  ( -4.944772684328424539, 109.4148137178985536, -11.48171059495408031 ) ) ;
#11444 = CARTESIAN_POINT ( 'NONE',  ( 16.56230152254411436, -7.209453229046482114, -1.434374999385489735 ) ) ;
#11445 = CARTESIAN_POINT ( 'NONE',  ( 24.47817193633207822, 3.604726614523236616, 161.3926148720374556 ) ) ;
#11446 = CARTESIAN_POINT ( 'NONE',  ( 21.00000000000000000, 6.646953231504538984, -1.715624999385482852 ) ) ;
#11447 = CARTESIAN_POINT ( 'NONE',  ( 11.61527771782809637, 57.66481371789855359, 4.622313124798827388 ) ) ;
#11448 = CARTESIAN_POINT ( 'NONE',  ( -27.24356964375000345, 199.8593750006145342, 0.000000000000000000 ) ) ;
#11449 = ORIENTED_EDGE ( 'NONE', *, *, #22130, .F. ) ;
#11450 = ORIENTED_EDGE ( 'NONE', *, *, #1759, .T. ) ;
#11451 = ORIENTED_EDGE ( 'NONE', *, *, #3669, .T. ) ;
#11452 = CARTESIAN_POINT ( 'NONE',  ( 26.99999999999999645, -3.464101615137751278, -6.956249998770937637 ) ) ;
#11453 = CARTESIAN_POINT ( 'NONE',  ( 18.12178482187499640, 4.985214923628404904, -3.815624999385480720 ) ) ;
#11454 = CYLINDRICAL_SURFACE ( 'NONE', #1565, 27.00000000000000355 ) ;
#11455 = CARTESIAN_POINT ( 'NONE',  ( 21.00000000000000000, 245.8093750006144944, 6.646953231504538984 ) ) ;
#11456 = CARTESIAN_POINT ( 'NONE',  ( 10.49813415415989581, 54.97268628210144925, 7.228626920339068285 ) ) ;
#11457 = EDGE_CURVE ( 'NONE', #12783, #1351, #20440, .T. ) ;
#11458 = CARTESIAN_POINT ( 'NONE',  ( -48.21502896937850124, 215.5714017266979567, -3.350049139982168800 ) ) ;
#11459 = CYLINDRICAL_SURFACE ( 'NONE', #23874, 6.000000000000001776 ) ;
#11460 = CARTESIAN_POINT ( 'NONE',  ( -41.28794563604517265, 206.7903428501025758, 3.378800118222471838 ) ) ;
#11461 =( NAMED_UNIT ( * ) PLANE_ANGLE_UNIT ( ) SI_UNIT ( $, .RADIAN. ) );
#11462 = CARTESIAN_POINT ( 'NONE',  ( 24.90302469878729141, 0.000000000000000000, 163.4540559201358576 ) ) ;
#11463 = CARTESIAN_POINT ( 'NONE',  ( -4.622313124798826500, 105.9648137178985650, 11.61527771782809637 ) ) ;
#11464 = CARTESIAN_POINT ( 'NONE',  ( -59.10788769728823411, 214.4690446883608104, 1.321298161741840893 ) ) ;
#11465 = CARTESIAN_POINT ( 'NONE',  ( -46.04538769728823411, 212.3930949314662371, -8.469044688360781947 ) ) ;
#11466 = CARTESIAN_POINT ( 'NONE',  ( 15.24356964375000167, -3.323476615752272600, -4.265624999385501326 ) ) ;
#11467 = CARTESIAN_POINT ( 'NONE',  ( 22.56230152254434529, -3.464101615137613610, -4.199999998771044574 ) ) ;
#11468 = CARTESIAN_POINT ( 'NONE',  ( 15.50000000000000533, 75.48981371789854222, -0.1745138560722452326 ) ) ;
#11469 = CARTESIAN_POINT ( 'NONE',  ( -38.51711230271183695, 216.4690446883607535, -1.857196546604089393 ) ) ;
#11470 = VERTEX_POINT ( 'NONE', #26664 ) ;
#11471 = CARTESIAN_POINT ( 'NONE',  ( 25.13834520420595098, 0.000000000000000000, 166.1437816049835874 ) ) ;
#11472 = CARTESIAN_POINT ( 'NONE',  ( -2.660918448318275509, 111.8976862821014606, 12.46528703574805874 ) ) ;
#11473 = CARTESIAN_POINT ( 'NONE',  ( -0.1745138560725817967, 47.21018628210144641, 15.50000000000000533 ) ) ;
#11474 = FACE_OUTER_BOUND ( 'NONE', #9205, .T. ) ;
#11475 = CARTESIAN_POINT ( 'NONE',  ( 24.67263818733777470, 0.000000000000000000, 163.6153742921546836 ) ) ;
#11476 = CARTESIAN_POINT ( 'NONE',  ( -15.46528703574804986, 58.99768628210144783, -3.257655550457287497 ) ) ;
#11477 = EDGE_CURVE ( 'NONE', #10799, #31903, #13375, .T. ) ;
#11478 = CARTESIAN_POINT ( 'NONE',  ( 22.80587116629411071, 7.646167579472015790E-16, -8.915624999385585170 ) ) ;
#11479 =( BOUNDED_CURVE ( )  B_SPLINE_CURVE ( 2, ( #18886, #1423, #12804, #35918, #15469 ),
 .UNSPECIFIED., .F., .F. ) 
 B_SPLINE_CURVE_WITH_KNOTS ( ( 3, 2, 3 ),
 ( 0.9565217391304360328, 0.9637681159420292687, 0.9662082944262200268 ),
 .UNSPECIFIED. ) 
 CURVE ( )  GEOMETRIC_REPRESENTATION_ITEM ( )  RATIONAL_B_SPLINE_CURVE ( ( 0.9999999999999774625, 0.8660254037844612451, 1.000000000000000000, 0.9548847740583508159, 0.9401541683247176540 ) ) 
 REPRESENTATION_ITEM ( '' )  );
#11480 = DIRECTION ( 'NONE',  ( -0.000000000000000000, -1.000000000000000000, -0.000000000000000000 ) ) ;
#11481 = CARTESIAN_POINT ( 'NONE',  ( -47.62872103062154849, 203.4690446883607535, 1.626142955000567936 ) ) ;
#11482 = CARTESIAN_POINT ( 'NONE',  ( 14.54431717697174875, 5.695505633664034839, -9.999999999999998224 ) ) ;
#11483 = CARTESIAN_POINT ( 'NONE',  ( -10.69584247140444866, 48.64768628210144641, 6.932735513423972762 ) ) ;
#11484 = CARTESIAN_POINT ( 'NONE',  ( -13.50000000000000533, 196.7750000000000057, -23.38268590217984411 ) ) ;
#11485 = CARTESIAN_POINT ( 'NONE',  ( -13.50000000000000533, 197.7875000012290627, -23.38268590217984411 ) ) ;
#11486 = CARTESIAN_POINT ( 'NONE',  ( 8.843639120294328748, 16.73518628210143788, -3.474262827703334722 ) ) ;
#11487 = CARTESIAN_POINT ( 'NONE',  ( 18.12178482187500350, 248.5843750006145285, 4.985214923628407568 ) ) ;
#11488 = ORIENTED_EDGE ( 'NONE', *, *, #19918, .T. ) ;
#11489 = CARTESIAN_POINT ( 'NONE',  ( 21.00000000000000000, 6.928203230275506996, -5.062500000000007994 ) ) ;
#11490 = DIRECTION ( 'NONE',  ( -0.000000000000000000, -0.000000000000000000, -1.000000000000000000 ) ) ;
#11491 = CARTESIAN_POINT ( 'NONE',  ( 27.51453976652391376, -5.407089921784865361, 160.2799941206736776 ) ) ;
#11492 = CARTESIAN_POINT ( 'NONE',  ( 19.68408634441910365, 5.407089921784857367, -3.440624999385522020 ) ) ;
#11493 = CARTESIAN_POINT ( 'NONE',  ( 25.22662187717753568, 0.000000000000000000, 169.9474368419002985 ) ) ;
#11494 = CARTESIAN_POINT ( 'NONE',  ( 26.99999999999999645, 241.2249999999999943, -7.347880794884117764E-16 ) ) ;
#11495 = CARTESIAN_POINT ( 'NONE',  ( 21.00000000000000355, 0.000000000000000000, 50.00000000000001421 ) ) ;
#11496 = CARTESIAN_POINT ( 'NONE',  ( 10.49813415415989581, 64.17268628210145209, 7.228626920339069173 ) ) ;
#11497 = ORIENTED_EDGE ( 'NONE', *, *, #4965, .F. ) ;
#11498 = ORIENTED_EDGE ( 'NONE', *, *, #10244, .F. ) ;
#11499 = CARTESIAN_POINT ( 'NONE',  ( 36.60243052835136268, 7.347880794884117764E-16, 159.4943175152456831 ) ) ;
#11500 = CARTESIAN_POINT ( 'NONE',  ( 27.00000000000000355, 195.8375000012290457, -3.306546357697854128E-15 ) ) ;
#11501 = CYLINDRICAL_SURFACE ( 'NONE', #28340, 27.00000000000000355 ) ;
#11502 = VECTOR ( 'NONE', #29211, 1000.000000000000000 ) ;
#11503 = CARTESIAN_POINT ( 'NONE',  ( -14.38691631536193860, 34.66481371789854649, -5.770363421894132649 ) ) ;
#11504 = CARTESIAN_POINT ( 'NONE',  ( 37.02077809343345649, -3.464101615137479495, 164.2760520648616875 ) ) ;
#11505 =( BOUNDED_CURVE ( )  B_SPLINE_CURVE ( 2, ( #30841, #37255, #22692, #5238, #1837, #37069, #13598, #2205, #5050 ),
 .UNSPECIFIED., .F., .F. ) 
 B_SPLINE_CURVE_WITH_KNOTS ( ( 3, 2, 2, 2, 3 ),
 ( 0.3541666666666666852, 0.3611111111111111049, 0.3750000000000000000, 0.3888888888888888951, 0.3958333333333333703 ),
 .UNSPECIFIED. ) 
 CURVE ( )  GEOMETRIC_REPRESENTATION_ITEM ( )  RATIONAL_B_SPLINE_CURVE ( ( 0.9330127018922194093, 0.9330127018922196314, 1.000000000000000000, 0.8660254037844387076, 1.000000000000000000, 0.8660254037844387076, 1.000000000000000000, 0.9330127018922190762, 0.9330127018922194093 ) ) 
 REPRESENTATION_ITEM ( '' )  );
#11506 = CARTESIAN_POINT ( 'NONE',  ( -42.68080436395489841, 205.4999999999999716, -0.1155267958017894420 ) ) ;
#11507 = CARTESIAN_POINT ( 'NONE',  ( 18.00000000000000000, 242.7812500012290400, -5.196152422706630247 ) ) ;
#11508 = CARTESIAN_POINT ( 'NONE',  ( 30.70615376348499836, -7.209453229046482114, 160.9418451752858346 ) ) ;
#11509 = CARTESIAN_POINT ( 'NONE',  ( -9.465287035748106703, 24.60231371789854649, 2.064181346179061460 ) ) ;
#11510 = CARTESIAN_POINT ( 'NONE',  ( 19.68408634441910721, -5.407089921784855591, -9.890624999385533300 ) ) ;
#11511 = AXIS2_PLACEMENT_3D ( 'NONE', #25828, #14459, #26014 ) ;
#11512 = CARTESIAN_POINT ( 'NONE',  ( 12.48663586349064403, 194.9999999999999716, 24.21355016816918493 ) ) ;
#11513 = CARTESIAN_POINT ( 'NONE',  ( -27.24356964374999635, 196.2968750006145342, 15.72908226750539384 ) ) ;
#11514 = CARTESIAN_POINT ( 'NONE',  ( 0.1745138560722461762, 123.7898137178985678, 15.50000000000000533 ) ) ;
#11515 = EDGE_CURVE ( 'NONE', #9547, #18985, #23089, .T. ) ;
#11516 = VERTEX_POINT ( 'NONE', #26106 ) ;
#11517 = CARTESIAN_POINT ( 'NONE',  ( 8.715434833791931624, 36.86018628210144499, 8.962234695871760692 ) ) ;
#11518 = FACE_OUTER_BOUND ( 'NONE', #23809, .T. ) ;
#11519 = DIRECTION ( 'NONE',  ( 0.000000000000000000, 1.000000000000000000, 0.000000000000000000 ) ) ;
#11520 = CARTESIAN_POINT ( 'NONE',  ( 25.18576762276457259, -3.604726614523244610, 169.4804705771697968 ) ) ;
#11521 = CARTESIAN_POINT ( 'NONE',  ( 26.99999999999999645, 7.347880794884117764E-16, -2.418749998770952647 ) ) ;
#11522 = CARTESIAN_POINT ( 'NONE',  ( 10.31873187879411091, 3.604726614523240613, -9.234374999385533300 ) ) ;
#11523 = CARTESIAN_POINT ( 'NONE',  ( 7.234628195640295800, 197.0950961906613941, 27.00000000000001066 ) ) ;
#11524 = AXIS2_PLACEMENT_3D ( 'NONE', #32416, #6460, #15556 ) ;
#11525 = CARTESIAN_POINT ( 'NONE',  ( 1.715153634034233487, 83.72268628210143504, 9.534712964251941258 ) ) ;
#11526 = CARTESIAN_POINT ( 'NONE',  ( 10.56230152254410903, 0.000000000000000000, -1.237499998771041110 ) ) ;
#11527 = DIRECTION ( 'NONE',  ( 0.000000000000000000, -1.000000000000000000, 0.000000000000000000 ) ) ;
#11528 = CARTESIAN_POINT ( 'NONE',  ( 4.622313124798573369, 92.63518628210145778, 11.61527771782819940 ) ) ;
#11529 = DIRECTION ( 'NONE',  ( 0.000000000000000000, 0.000000000000000000, 1.000000000000000000 ) ) ;
#11530 = VERTEX_POINT ( 'NONE', #8679 ) ;
#11531 = CARTESIAN_POINT ( 'NONE',  ( 33.87652354815133293, 5.407089921784857367, 161.3608737722381079 ) ) ;
#11532 = CARTESIAN_POINT ( 'NONE',  ( 23.87821517812499650, 4.985214923628404904, -7.490624999385464555 ) ) ;
#11533 = CARTESIAN_POINT ( 'NONE',  ( -13.62178482187498396, 195.4343750006145228, 23.59362340125808188 ) ) ;
#11534 = CARTESIAN_POINT ( 'NONE',  ( 37.44563085588819717, 7.646167579472024665E-16, 166.3374931129601464 ) ) ;
#11535 = CARTESIAN_POINT ( 'NONE',  ( 37.06653485837549766, 3.464101615137759271, 164.7990542813598722 ) ) ;
#11536 = CARTESIAN_POINT ( 'NONE',  ( 18.00000000000000000, 5.196152422706630247, -0.07499999999999173994 ) ) ;
#11537 = CARTESIAN_POINT ( 'NONE',  ( 26.75643035624999655, 240.2218750006145171, -3.323476615752271712 ) ) ;
#11538 = CARTESIAN_POINT ( 'NONE',  ( -13.62178482187500528, 198.3781250006145171, -23.59362340125807123 ) ) ;
#11539 = CARTESIAN_POINT ( 'NONE',  ( 12.46528703574811558, 121.2023137178985621, -2.660918448318005503 ) ) ;
#11540 = CARTESIAN_POINT ( 'NONE',  ( 12.46528703574805874, 127.9976862821014549, 2.660918448318279950 ) ) ;
#11542 = VERTEX_POINT ( 'NONE', #11888 ) ;
#11541 = ORIENTED_EDGE ( 'NONE', *, *, #9657, .F. ) ;
#11543 = CARTESIAN_POINT ( 'NONE',  ( -13.62178482187498396, 197.1781250006145569, 23.59362340125808188 ) ) ;
#11544 = CARTESIAN_POINT ( 'NONE',  ( 26.75643035624999655, 242.3218750006145399, -7.049594010296217766E-16 ) ) ;
#11545 = CARTESIAN_POINT ( 'NONE',  ( 10.56230152254300947, -3.464101615137121115, -2.099999998771007181 ) ) ;
#11546 = CARTESIAN_POINT ( 'NONE',  ( -0.1745138560722442889, 100.7898137178985536, -15.50000000000000533 ) ) ;
#11547 = CARTESIAN_POINT ( 'NONE',  ( 23.87821517812499650, 4.985214923628404904, -1.753124999385485827 ) ) ;
#11548 = CARTESIAN_POINT ( 'NONE',  ( -13.49999999999998401, 196.1375000012290286, 23.38268590217985476 ) ) ;
#11549 = EDGE_CURVE ( 'NONE', #23800, #16763, #22939, .T. ) ;
#11550 = CARTESIAN_POINT ( 'NONE',  ( 0.1745138560723095977, 77.78981371789853938, 9.500000000000005329 ) ) ;
#11551 = CARTESIAN_POINT ( 'NONE',  ( 22.80587116629410716, -3.604726614523235284, -2.203124999385539962 ) ) ;
#11552 = EDGE_CURVE ( 'NONE', #12668, #8594, #27770, .T. ) ;
#11553 = CARTESIAN_POINT ( 'NONE',  ( 15.24356964375000167, 242.1343750006145683, 3.323476615752272600 ) ) ;
#11554 = CARTESIAN_POINT ( 'NONE',  ( -8.715434833792127023, 42.13981371789854791, 8.962234695871568846 ) ) ;
#11555 = DIRECTION ( 'NONE',  ( 1.000000000000000000, 0.000000000000000000, 0.000000000000000000 ) ) ;
#11556 = CARTESIAN_POINT ( 'NONE',  ( -10.49813415415989581, 96.37268628210145494, -7.228626920339068285 ) ) ;
#11557 = CARTESIAN_POINT ( 'NONE',  ( 13.56230152254411259, -5.196152422706632912, -2.962499998771017662 ) ) ;
#11558 = EDGE_CURVE ( 'NONE', #34009, #23156, #36778, .T. ) ;
#11559 = CARTESIAN_POINT ( 'NONE',  ( -34.76413769728823411, 213.1499508600178672, 5.686928522499718142 ) ) ;
#11560 = CARTESIAN_POINT ( 'NONE',  ( 21.00000000000000000, 239.8187500012290059, 5.999999999999998224 ) ) ;
#11561 = VECTOR ( 'NONE', #3207, 1000.000000000000000 ) ;
#11562 = CARTESIAN_POINT ( 'NONE',  ( 1.069080835302379631E-14, 198.8750000012290400, 27.00000000000000000 ) ) ;
#11563 = CARTESIAN_POINT ( 'NONE',  ( 13.23911966647218996, 108.4476862821014294, -8.632099005475504683 ) ) ;
#11564 = CARTESIAN_POINT ( 'NONE',  ( 10.49813415415989581, 8.972686282101433264, 7.228626920339069173 ) ) ;
#11565 = CARTESIAN_POINT ( 'NONE',  ( -27.12178482187499995, 199.9296875003072671, 0.000000000000000000 ) ) ;
#11566 = DIRECTION ( 'NONE',  ( 0.000000000000000000, 0.000000000000000000, 1.000000000000000000 ) ) ;
#11567 = CARTESIAN_POINT ( 'NONE',  ( 9.500000000000005329, 127.7101862821014606, 0.1745138560725188748 ) ) ;
#11568 = CARTESIAN_POINT ( 'NONE',  ( 27.00000000000007816, 3.464101615137709533, -4.631249998770966769 ) ) ;
#11569 = CARTESIAN_POINT ( 'NONE',  ( 26.75643035624999655, 243.2218750006145171, -7.049594010296217766E-16 ) ) ;
#11570 = VERTEX_POINT ( 'NONE', #23456 ) ;
#11571 = CARTESIAN_POINT ( 'NONE',  ( -5.233372021372430183, 69.34768628210143504, -8.152565276336710909 ) ) ;
#11572 = CARTESIAN_POINT ( 'NONE',  ( 21.00000000000000000, 6.646953231504538984, -0.7031249993854685743 ) ) ;
#11573 = CARTESIAN_POINT ( 'NONE',  ( 15.00000000000047606, 3.464101615138028389, -4.987500000000019362 ) ) ;
#11574 = DIRECTION ( 'NONE',  ( -0.000000000000000000, -0.000000000000000000, 1.000000000000000000 ) ) ;
#11575 = CARTESIAN_POINT ( 'NONE',  ( 20.99999999999999289, 243.5874999999999488, -5.999999999999997335 ) ) ;
#11576 = CARTESIAN_POINT ( 'NONE',  ( 20.99999999999999645, 185.0294372515228645, 5.999999999999999112 ) ) ;
#11577 = CARTESIAN_POINT ( 'NONE',  ( 34.23809944139907202, 5.196152422706637353, 166.8910292673464539 ) ) ;
#11578 = CARTESIAN_POINT ( 'NONE',  ( -5.233372021372612259, 32.65231371789855075, 8.152565276336593669 ) ) ;
#11579 = CARTESIAN_POINT ( 'NONE',  ( -27.24356964374999279, 199.4468750006145399, 15.72908226750539384 ) ) ;
#11580 = VERTEX_POINT ( 'NONE', #15113 ) ;
#11581 = VERTEX_POINT ( 'NONE', #694 ) ;
#11582 = CARTESIAN_POINT ( 'NONE',  ( 21.00000000000000000, 249.4093750006145171, 6.646953231504538984 ) ) ;
#11583 = CARTESIAN_POINT ( 'NONE',  ( -12.50000000000000355, 52.48981371789855643, 0.1745138560722786503 ) ) ;
#11584 = CARTESIAN_POINT ( 'NONE',  ( 22.80587116629412492, -3.604726614523238837, -7.659374999385500260 ) ) ;
#11585 = CARTESIAN_POINT ( 'NONE',  ( 26.75643035624999655, -3.323476615752267715, -8.615624999385470772 ) ) ;
#11586 = CARTESIAN_POINT ( 'NONE',  ( 14.38691631536194393, 140.4648137178985507, 5.770363421894124656 ) ) ;
#11587 = ORIENTED_EDGE ( 'NONE', *, *, #16417, .F. ) ;
#11588 = CARTESIAN_POINT ( 'NONE',  ( 19.68408634441911786, -5.407089921784861808, -4.096874999385518912 ) ) ;
#11589 = CARTESIAN_POINT ( 'NONE',  ( -27.24356964374999635, 198.9406250006145171, 15.72908226750539384 ) ) ;
#11590 = CARTESIAN_POINT ( 'NONE',  ( 37.40641077165175687, 7.646167579472024665E-16, 165.8892054988188534 ) ) ;
#11591 = CARTESIAN_POINT ( 'NONE',  ( -61.87127896937851546, 218.5309553116392465, 2.162041339862725842 ) ) ;
#11592 = CARTESIAN_POINT ( 'NONE',  ( 20.99999999999999645, 249.4093750006145171, 6.646953231504538984 ) ) ;
#11593 = FILL_AREA_STYLE_COLOUR ( '', #25636 ) ;
#11594 = CARTESIAN_POINT ( 'NONE',  ( -26.95863322649103111, 194.9999999999998863, -2.574242593721492334 ) ) ;
#11595 = CARTESIAN_POINT ( 'NONE',  ( -54.94419563604517265, 205.4999999999999716, 0.1155267958017633378 ) ) ;
#11596 = CARTESIAN_POINT ( 'NONE',  ( -50.59747103062156270, 213.3500491399821328, -5.571401726697985168 ) ) ;
#11597 = CARTESIAN_POINT ( 'NONE',  ( 34.45175145028584041, -5.407089921784855591, 167.9357587796436064 ) ) ;
#11598 = ORIENTED_EDGE ( 'NONE', *, *, #20298, .F. ) ;
#11599 = CARTESIAN_POINT ( 'NONE',  ( 9.184850993605147944E-16, 148.0000000000000000, -7.500000000000000000 ) ) ;
#11600 = CARTESIAN_POINT ( 'NONE',  ( 27.00000000000013500, 3.464101615137676227, -0.5812499987709733862 ) ) ;
#11601 = CARTESIAN_POINT ( 'NONE',  ( 15.50000000000000533, 29.48981371789855288, -0.1745138560722452326 ) ) ;
#11602 = CARTESIAN_POINT ( 'NONE',  ( -55.34747103062157692, 214.3500491399821044, -7.303452534266878793 ) ) ;
#11603 = CARTESIAN_POINT ( 'NONE',  ( 12.53471296425194836, 7.822686282101448896, -2.311890736173178418 ) ) ;
#11604 = CARTESIAN_POINT ( 'NONE',  ( -11.61527771782819940, 48.93518628210144783, 4.622313124798574258 ) ) ;
#11605 = CARTESIAN_POINT ( 'NONE',  ( 22.56230152254411792, 7.347880794884125653E-16, -5.175000000000040679 ) ) ;
#11606 = ORIENTED_EDGE ( 'NONE', *, *, #1948, .T. ) ;
#11607 = CARTESIAN_POINT ( 'NONE',  ( -38.52455436395489841, 205.1570982666397640, 4.673758765035199048 ) ) ;
#11608 = AXIS2_PLACEMENT_3D ( 'NONE', #5970, #17550, #31389 ) ;
#11609 = CARTESIAN_POINT ( 'NONE',  ( -81.00000000000002842, 206.0000000000000000, -2.499999999999998668 ) ) ;
#11610 = CARTESIAN_POINT ( 'NONE',  ( 5.778771075727756162E-15, 195.9218750006145342, 31.45816453501075927 ) ) ;
#11611 = DIRECTION ( 'NONE',  ( 0.08715574274765143514, 0.000000000000000000, 0.9961946980917462113 ) ) ;
#11612 = CARTESIAN_POINT ( 'NONE',  ( 27.00000000000001421, 196.2500000012290116, 15.58845726811988897 ) ) ;
#11613 = CARTESIAN_POINT ( 'NONE',  ( -3.253724281355068545E-15, 197.6374999999999602, -27.00000000000000000 ) ) ;
#11614 = CARTESIAN_POINT ( 'NONE',  ( 26.99999999999999645, 246.1937500012290343, 3.464101615137751278 ) ) ;
#11615 = CARTESIAN_POINT ( 'NONE',  ( 15.24356964374999990, 245.7718750006145001, -3.323476615752268604 ) ) ;
#11616 = CARTESIAN_POINT ( 'NONE',  ( -3.474262827703527901, 96.76481371789854791, 8.843639120294245259 ) ) ;
#11617 = CARTESIAN_POINT ( 'NONE',  ( 15.00000000000000355, 7.347880794884112834E-16, -8.000000000000000000 ) ) ;
#11618 = ORIENTED_EDGE ( 'NONE', *, *, #25453, .T. ) ;
#11619 = CARTESIAN_POINT ( 'NONE',  ( -60.09747103062156981, 213.3500491399821328, -5.571401726697985168 ) ) ;
#11620 = CARTESIAN_POINT ( 'NONE',  ( -3.253724281355068545E-15, 197.3000000012290229, -27.00000000000000000 ) ) ;
#11621 = CARTESIAN_POINT ( 'NONE',  ( 15.00000000000000000, 246.8687500012290457, -3.464101615137752166 ) ) ;
#11622 = ORIENTED_EDGE ( 'NONE', *, *, #30740, .F. ) ;
#11623 = CARTESIAN_POINT ( 'NONE',  ( 8.962234695871567070, 95.03981371789856780, 8.715434833792127023 ) ) ;
#11624 = CARTESIAN_POINT ( 'NONE',  ( 22.80587116629411781, 7.646167579472024665E-16, -1.321874999385519445 ) ) ;
#11625 = CARTESIAN_POINT ( 'NONE',  ( 13.50000000000001421, 198.0125000012290286, 23.38268590217984055 ) ) ;
#11626 = CARTESIAN_POINT ( 'NONE',  ( 21.00000000000000000, -6.646953231504538984, -1.940624999385496929 ) ) ;
#11627 = CARTESIAN_POINT ( 'NONE',  ( -2.660918448318004614, 63.70231371789855501, -12.46528703574811558 ) ) ;
#11628 = CARTESIAN_POINT ( 'NONE',  ( 13.50000000000001421, 195.6500000000000057, 23.38268590217984055 ) ) ;
#11629 = ORIENTED_EDGE ( 'NONE', *, *, #18769, .F. ) ;
#11630 = ORIENTED_EDGE ( 'NONE', *, *, #11687, .F. ) ;
#11631 = VERTEX_POINT ( 'NONE', #28758 ) ;
#11632 = CARTESIAN_POINT ( 'NONE',  ( 18.00000000000000355, -5.196152422706632912, -7.968749998770952025 ) ) ;
#11633 = CARTESIAN_POINT ( 'NONE',  ( 26.75643035624999655, 7.049594010296217766E-16, -3.965624999385464200 ) ) ;
#11634 = CARTESIAN_POINT ( 'NONE',  ( 16.56230152254411081, 6.928203230275506996, -6.299999998771006915 ) ) ;
#11635 = CARTESIAN_POINT ( 'NONE',  ( 23.87821517812500005, 247.6468750006145285, 4.985214923628404016 ) ) ;
#11636 = CARTESIAN_POINT ( 'NONE',  ( 8.715434833791931624, 46.06018628210144072, 8.962234695871760692 ) ) ;
#11637 = CARTESIAN_POINT ( 'NONE',  ( -51.97544563604517265, 214.8429017333602360, 4.673758765035156415 ) ) ;
#11638 = CARTESIAN_POINT ( 'NONE',  ( 17.99309595496827541, 218.0184107867384000, -5.206989594057217730 ) ) ;
#11639 = CARTESIAN_POINT ( 'NONE',  ( -48.41294563604517265, 213.2096571498974527, -3.378800118222469617 ) ) ;
#11640 = CARTESIAN_POINT ( 'NONE',  ( 36.71682244070765933, -3.464101615137751278, 160.8018230564910880 ) ) ;
#11641 = CARTESIAN_POINT ( 'NONE',  ( -2.311890736173448424, 105.6773137178985564, 12.53471296425189330 ) ) ;
#11642 = CARTESIAN_POINT ( 'NONE',  ( -58.51413769728822700, 212.1499508600178387, 3.954877714930865817 ) ) ;
#11643 = CARTESIAN_POINT ( 'NONE',  ( -39.51413769728823411, 214.1499508600179240, 7.418979330068584233 ) ) ;
#11644 = CARTESIAN_POINT ( 'NONE',  ( 15.24356964374999990, 3.323476615752268604, -3.890624999385467575 ) ) ;
#11645 = CARTESIAN_POINT ( 'NONE',  ( 23.99999999999999645, 5.196152422706631135, -0.5999999999999894307 ) ) ;
#11646 = CARTESIAN_POINT ( 'NONE',  ( -13.04141134922778456, 79.22731371789853938, 8.927990412390377273 ) ) ;
#11647 = CARTESIAN_POINT ( 'NONE',  ( -60.28794563604517975, 203.8621396198271043, 6.307003348498029460 ) ) ;
#11648 = ORIENTED_EDGE ( 'NONE', *, *, #33263, .F. ) ;
#11649 = DIRECTION ( 'NONE',  ( -0.000000000000000000, -1.000000000000000000, -0.000000000000000000 ) ) ;
#11650 = CARTESIAN_POINT ( 'NONE',  ( 12.46528703574805874, 109.5976862821014493, 2.660918448318279950 ) ) ;
#11651 = CARTESIAN_POINT ( 'NONE',  ( -3.257655550457281723, 47.49768628210145494, 15.46528703574804986 ) ) ;
#11652 = CARTESIAN_POINT ( 'NONE',  ( 20.99999999999999645, 0.000000000000000000, -8.000000000000000000 ) ) ;
#11653 = CARTESIAN_POINT ( 'NONE',  ( 30.84342405831255007, 7.209453229046482114, 162.5108518247803318 ) ) ;
#11654 = CARTESIAN_POINT ( 'NONE',  ( -2.908627838312119351, 69.92268628210143788, -15.53471296425195369 ) ) ;
#11655 = CARTESIAN_POINT ( 'NONE',  ( 13.62178482187501416, 199.0531250006145285, 23.59362340125806767 ) ) ;
#11656 = CARTESIAN_POINT ( 'NONE',  ( 16.56230152254411081, 7.209453229046475009, -8.353124999385522997 ) ) ;
#11657 = CYLINDRICAL_SURFACE ( 'NONE', #37013, 5.999999999999994671 ) ;
#11658 = CARTESIAN_POINT ( 'NONE',  ( -52.97247103062156981, 206.6499508600178672, 5.571401726697986057 ) ) ;
#11659 = AXIS2_PLACEMENT_3D ( 'NONE', #1802, #30245, #7314 ) ;
#11660 = EDGE_CURVE ( 'NONE', #35488, #10943, #2797, .T. ) ;
#11661 = CARTESIAN_POINT ( 'NONE',  ( 10.36878992021261148, -0.004136371210273081730, -9.999999999999998224 ) ) ;
#11662 = CARTESIAN_POINT ( 'NONE',  ( -4.622313124798576922, 42.03518628210144215, -11.61527771782819762 ) ) ;
#11663 = CARTESIAN_POINT ( 'NONE',  ( 13.62178482187501416, 199.5593750006145513, 23.59362340125806767 ) ) ;
#11664 = CARTESIAN_POINT ( 'NONE',  ( 25.00000000000004263, 0.000000000000000000, 49.82535622836640954 ) ) ;
#11665 = CARTESIAN_POINT ( 'NONE',  ( -9.534712964251941258, 12.42268628210144144, 1.715153634034234154 ) ) ;
#11666 = CARTESIAN_POINT ( 'NONE',  ( 26.75643035624999655, 248.3218750006145399, -3.323476615752271268 ) ) ;
#11667 = ORIENTED_EDGE ( 'NONE', *, *, #9857, .F. ) ;
#11668 = CARTESIAN_POINT ( 'NONE',  ( 18.00000000000000000, 5.196152422706630247, -5.475000000000007638 ) ) ;
#11670 = CARTESIAN_POINT ( 'NONE',  ( 2.999999999999997335, 244.5000000000000000, 1.000000000000000000 ) ) ;
#11669 = PRODUCT_DEFINITION_SHAPE ( 'NONE', 'NONE',  #37504 ) ;
#11671 = CARTESIAN_POINT ( 'NONE',  ( 13.49999999999999645, 197.5999999999999943, -23.38268590217984766 ) ) ;
#11672 = CARTESIAN_POINT ( 'NONE',  ( 10.31873187879410914, 0.000000000000000000, -5.540624999385540761 ) ) ;
#11673 = CARTESIAN_POINT ( 'NONE',  ( 25.07300988058480229, -3.604726614523240613, 168.1916436865136291 ) ) ;
#11674 = CARTESIAN_POINT ( 'NONE',  ( 21.00000000000000000, 240.2125000000000057, 6.928203230275506996 ) ) ;
#11675 = CARTESIAN_POINT ( 'NONE',  ( 1.120210788295102201E-13, 196.4000000012290741, -27.00000000000000711 ) ) ;
#11676 = ADVANCED_FACE ( 'NONE', ( #10173 ), #29889, .T. ) ;
#11677 = CIRCLE ( 'NONE', #16621, 3.500000000000002220 ) ;
#11678 = CARTESIAN_POINT ( 'NONE',  ( -0.1745138560725500443, 65.61018628210145209, 12.50000000000000355 ) ) ;
#11679 = ORIENTED_EDGE ( 'NONE', *, *, #33263, .T. ) ;
#11680 = ORIENTED_EDGE ( 'NONE', *, *, #15193, .T. ) ;
#11681 = CARTESIAN_POINT ( 'NONE',  ( 33.60730975337005333, -5.196152422706629359, 159.6810701411317552 ) ) ;
#11682 = CARTESIAN_POINT ( 'NONE',  ( -13.50000000000000533, 195.0875000012290457, -23.38268590217984411 ) ) ;
#11683 = CARTESIAN_POINT ( 'NONE',  ( 0.000000000000000000, 200.0000000000000000, -27.00000000000000355 ) ) ;
#11684 = CARTESIAN_POINT ( 'NONE',  ( 18.12178482187499640, 4.985214923628404904, -5.615624999385476990 ) ) ;
#11685 = CARTESIAN_POINT ( 'NONE',  ( -3.257655550456946880, 36.10231371789854649, -15.46528703574811736 ) ) ;
#11686 = LINE ( 'NONE', #23439, #7915 ) ;
#11687 = EDGE_CURVE ( 'NONE', #190, #8211, #1741, .T. ) ;
#11688 = CARTESIAN_POINT ( 'NONE',  ( 15.24356964375000167, 241.3468750006145456, 3.323476615752272600 ) ) ;
#11689 = CARTESIAN_POINT ( 'NONE',  ( -49.40997103062157692, 213.8393509191290889, 2.350049139982164359 ) ) ;
#11690 = EDGE_CURVE ( 'NONE', #14163, #1071, #25954, .T. ) ;
#11691 = CARTESIAN_POINT ( 'NONE',  ( 24.43731768191911513, 0.000000000000000000, 160.9256486073069539 ) ) ;
#11692 = CARTESIAN_POINT ( 'NONE',  ( 0.1745138560723095977, 22.58981371789854364, 9.500000000000005329 ) ) ;
#11693 = CARTESIAN_POINT ( 'NONE',  ( -56.93080436395490551, 203.5000000000000000, -0.1155267958017335561 ) ) ;
#11694 = CARTESIAN_POINT ( 'NONE',  ( 0.000000000000000000, 0.000000000000000000, 5.000000000000000000 ) ) ;
#11695 = CARTESIAN_POINT ( 'NONE',  ( 52.59268362704444399, 124.7349959275252615, -2.500000000000000000 ) ) ;
#11696 = CARTESIAN_POINT ( 'NONE',  ( 13.62178482187501416, 195.5093750006145399, 23.59362340125806767 ) ) ;
#11697 = CARTESIAN_POINT ( 'NONE',  ( 14.38691631536194393, 131.2648137178985621, 5.770363421894124656 ) ) ;
#11698 = EDGE_LOOP ( 'NONE', ( #11770, #12025, #9170, #298 ) ) ;
#11699 =( BOUNDED_CURVE ( )  B_SPLINE_CURVE ( 2, ( #35840, #9513, #1532, #4002, #21276, #18431, #15198 ),
 .UNSPECIFIED., .F., .F. ) 
 B_SPLINE_CURVE_WITH_KNOTS ( ( 3, 2, 2, 3 ),
 ( 0.8913043478260908037, 0.8985507246376851498, 0.9057971014492794959, 0.9130434782608737310 ),
 .UNSPECIFIED. ) 
 CURVE ( )  GEOMETRIC_REPRESENTATION_ITEM ( )  RATIONAL_B_SPLINE_CURVE ( ( 0.9999999999999281686, 0.8660254037845105390, 1.000000000000000000, 0.8660254037844387076, 1.000000000000000000, 0.8660254037843606589, 1.000000000000077938 ) ) 
 REPRESENTATION_ITEM ( '' )  );
#11700 = CARTESIAN_POINT ( 'NONE',  ( 11.48171059495397728, 54.68518628210144783, 4.944772684328674117 ) ) ;
#11701 = CARTESIAN_POINT ( 'NONE',  ( 21.00000000000000000, 240.6624999999999943, 5.999999999999998224 ) ) ;
#11702 = CARTESIAN_POINT ( 'NONE',  ( 25.47963170482115913, 3.634172111495134416, -8.000000000000000000 ) ) ;
#11703 = CARTESIAN_POINT ( 'NONE',  ( 31.37289519550453321, -7.209453229046482114, 168.5627346156876740 ) ) ;
#11704 = CARTESIAN_POINT ( 'NONE',  ( 18.00000000000000000, 5.196152422706630247, -2.718749998770947585 ) ) ;
#11705 = CARTESIAN_POINT ( 'NONE',  ( 22.80587116629411781, -3.604726614523238837, -8.109374999385527971 ) ) ;
#11706 = CARTESIAN_POINT ( 'NONE',  ( -43.77105176259354380, 253.6555389399068190, -0.4999999999999995559 ) ) ;
#11707 = CARTESIAN_POINT ( 'NONE',  ( 3.474262827703335166, 55.83518628210145351, 8.843639120294326972 ) ) ;
#11708 = CARTESIAN_POINT ( 'NONE',  ( 13.56230152254411614, -5.196152422706632912, -1.162499998771021614 ) ) ;
#11709 = CARTESIAN_POINT ( 'NONE',  ( 20.99999999999995381, 244.7125000000000057, 5.999999999999998224 ) ) ;
#11710 = CARTESIAN_POINT ( 'NONE',  ( 12.53471296425194836, 99.82268628210144357, -2.311890736173178418 ) ) ;
#11711 = CARTESIAN_POINT ( 'NONE',  ( 1.069080835302379631E-14, 199.6625000000000227, 27.00000000000000000 ) ) ;
#11712 = DIRECTION ( 'NONE',  ( -0.000000000000000000, -1.000000000000000000, -0.000000000000000000 ) ) ;
#11713 = ORIENTED_EDGE ( 'NONE', *, *, #1726, .F. ) ;
#11714 = CARTESIAN_POINT ( 'NONE',  ( 24.55661210480496592, 3.604726614523236616, 162.2891901003200132 ) ) ;
#11715 = CARTESIAN_POINT ( 'NONE',  ( 15.24356964374999990, 0.000000000000000000, -8.240624999385465443 ) ) ;
#11717 = EDGE_CURVE ( 'NONE', #3008, #7787, #18912, .T. ) ;
#11716 = DIRECTION ( 'NONE',  ( -0.000000000000000000, 1.000000000000000000, -0.000000000000000000 ) ) ;
#11718 = CARTESIAN_POINT ( 'NONE',  ( 24.98639886122932197, 0.000000000000000000, 167.2016752052849426 ) ) ;
#11719 = CARTESIAN_POINT ( 'NONE',  ( 37.26263527955770627, 3.464101615137759271, 167.0404923520662805 ) ) ;
#11720 = CYLINDRICAL_SURFACE ( 'NONE', #32586, 5.999999999999994671 ) ;
#11721 = CARTESIAN_POINT ( 'NONE',  ( 15.00000000000000000, 247.2999999999999829, 0.000000000000000000 ) ) ;
#11722 = CARTESIAN_POINT ( 'NONE',  ( -27.24356964374999279, 199.3906250006145342, 15.72908226750539384 ) ) ;
#11723 = EDGE_CURVE ( 'NONE', #4359, #7912, #13024, .T. ) ;
#11724 =( BOUNDED_CURVE ( )  B_SPLINE_CURVE ( 2, ( #22649, #16590, #36661, #5008, #10699, #27765, #28134, #22090, #34195 ),
 .UNSPECIFIED., .F., .F. ) 
 B_SPLINE_CURVE_WITH_KNOTS ( ( 3, 2, 2, 2, 3 ),
 ( 0.8369565217391303769, 0.8405797101449274944, 0.8478260869565217295, 0.8550724637681159646, 0.8586956521739130821 ),
 .UNSPECIFIED. ) 
 CURVE ( )  GEOMETRIC_REPRESENTATION_ITEM ( )  RATIONAL_B_SPLINE_CURVE ( ( 0.9330127018922192983, 0.9330127018922182991, 1.000000000000000000, 0.8660254037844387076, 1.000000000000000000, 0.8660254037844387076, 1.000000000000000000, 0.9330127018922194093, 0.9330127018922194093 ) ) 
 REPRESENTATION_ITEM ( '' )  );
#11725 = CARTESIAN_POINT ( 'NONE',  ( 2.311890736173452865, 128.6773137178985564, -12.53471296425189152 ) ) ;
#11726 = CARTESIAN_POINT ( 'NONE',  ( 2.311890736173175753, 120.5226862821014606, 12.53471296425194659 ) ) ;
#11728 = EDGE_LOOP ( 'NONE', ( #25389, #12386, #17332, #36940 ) ) ;
#11727 = ORIENTED_EDGE ( 'NONE', *, *, #2771, .F. ) ;
#11729 = CARTESIAN_POINT ( 'NONE',  ( -27.24356964374999635, 197.1406250006145058, 15.72908226750539384 ) ) ;
#11730 = CARTESIAN_POINT ( 'NONE',  ( 15.24356964374999990, 242.5093750006144830, -3.323476615752268604 ) ) ;
#11731 = EDGE_CURVE ( 'NONE', #30158, #31903, #24580, .T. ) ;
#11732 = CARTESIAN_POINT ( 'NONE',  ( -13.04141134922778456, 88.42731371789855643, 8.927990412390377273 ) ) ;
#11733 = CARTESIAN_POINT ( 'NONE',  ( 18.12178482187500350, -4.985214923628407568, -3.328124999385479121 ) ) ;
#11734 = CARTESIAN_POINT ( 'NONE',  ( 15.24356964374999990, 248.4718750006145171, -3.323476615752268604 ) ) ;
#11735 = COLOUR_RGB ( '',0.8941176470588234615, 0.8941176470588234615, 0.8941176470588234615 ) ;
#11736 = EDGE_CURVE ( 'NONE', #21332, #17896, #21191, .T. ) ;
#11737 = CARTESIAN_POINT ( 'NONE',  ( -13.49999999999998401, 197.0375000012290627, 23.38268590217985476 ) ) ;
#11738 = CARTESIAN_POINT ( 'NONE',  ( 6.594114490232462877, 83.53981371789856780, -6.840914352311949109 ) ) ;
#11739 = CARTESIAN_POINT ( 'NONE',  ( 22.80587116629411071, -3.604726614523235284, -4.903124999385514826 ) ) ;
#11740 = VECTOR ( 'NONE', #29669, 1000.000000000000000 ) ;
#11741 = CARTESIAN_POINT ( 'NONE',  ( 15.24356964375000167, 241.2343750006145058, 3.323476615752272600 ) ) ;
#11742 = CARTESIAN_POINT ( 'NONE',  ( 11.48171059495408208, 56.51481371789855501, -4.944772684328420986 ) ) ;
#11743 = CARTESIAN_POINT ( 'NONE',  ( 20.99999999999997868, 246.5687500012290343, 5.999999999999999112 ) ) ;
#11744 = CARTESIAN_POINT ( 'NONE',  ( -12.46528703574805697, 95.79768628210143788, -2.660918448318280838 ) ) ;
#11745 = CARTESIAN_POINT ( 'NONE',  ( 19.56230152254411792, -5.196152422706629359, -3.337499998771031873 ) ) ;
#11746 = CARTESIAN_POINT ( 'NONE',  ( -37.13913769728823411, 206.8500491399821044, -5.686928522499717253 ) ) ;
#11747 = CARTESIAN_POINT ( 'NONE',  ( -10.69584247140444866, 140.6476862821014890, 6.932735513423972762 ) ) ;
#11748 = CARTESIAN_POINT ( 'NONE',  ( 0.000000000000000000, 2.000000000000000000, 0.000000000000000000 ) ) ;
#11749 = CARTESIAN_POINT ( 'NONE',  ( 15.46528703574804986, 109.5976862821014493, 3.257655550457285720 ) ) ;
#11750 = CARTESIAN_POINT ( 'NONE',  ( 0.1745138560725515708, 15.01018628210143468, -12.50000000000000355 ) ) ;
#11751 = CARTESIAN_POINT ( 'NONE',  ( 24.97165984609394940, 0.000000000000000000, 164.2385592436587558 ) ) ;
#11752 = CYLINDRICAL_SURFACE ( 'NONE', #33891, 5.999999999999998224 ) ;
#11753 = CARTESIAN_POINT ( 'NONE',  ( 1.715153634034233487, 129.7226862821014208, 9.534712964251941258 ) ) ;
#11754 = CARTESIAN_POINT ( 'NONE',  ( 36.83775103377001869, 7.347880794884117764E-16, 162.1840432000934129 ) ) ;
#11755 = CARTESIAN_POINT ( 'NONE',  ( 18.12178482187500350, 243.0718750006145399, 4.985214923628407568 ) ) ;
#11756 = ORIENTED_EDGE ( 'NONE', *, *, #15622, .T. ) ;
#11757 = CARTESIAN_POINT ( 'NONE',  ( 25.22335353682449721, 3.604726614523236616, 169.9100795407219096 ) ) ;
#11758 = AXIS2_PLACEMENT_3D ( 'NONE', #14330, #19479, #25884 ) ;
#11759 = CARTESIAN_POINT ( 'NONE',  ( -7.954856959092191815, 59.57268628210145067, -5.529263428287477744 ) ) ;
#11760 =( BOUNDED_CURVE ( )  B_SPLINE_CURVE ( 2, ( #25328, #36877, #22498, #5234, #16810, #280, #11846 ),
 .UNSPECIFIED., .F., .F. ) 
 B_SPLINE_CURVE_WITH_KNOTS ( ( 3, 2, 2, 3 ),
 ( 0.8043478260869549867, 0.8115942028985493328, 0.8188405797101435679, 0.8260869565217379140 ),
 .UNSPECIFIED. ) 
 CURVE ( )  GEOMETRIC_REPRESENTATION_ITEM ( )  RATIONAL_B_SPLINE_CURVE ( ( 1.000000000000028644, 0.8660254037844099528, 1.000000000000000000, 0.8660254037844387076, 1.000000000000000000, 0.8660254037844612451, 0.9999999999999774625 ) ) 
 REPRESENTATION_ITEM ( '' )  );
#11761 = AXIS2_PLACEMENT_3D ( 'NONE', #37461, #8487, #17959 ) ;
#11762 = CARTESIAN_POINT ( 'NONE',  ( 20.99999999999999645, 0.000000000000000000, -8.000000000000000000 ) ) ;
#11763 = ADVANCED_FACE ( 'NONE', ( #27417 ), #36132, .T. ) ;
#11764 = CARTESIAN_POINT ( 'NONE',  ( 26.99999999999999645, 241.2624999999999886, -3.464101615137755275 ) ) ;
#11765 = CARTESIAN_POINT ( 'NONE',  ( -13.62178482187500528, 196.6343750006145399, -23.59362340125807123 ) ) ;
#11766 = CYLINDRICAL_SURFACE ( 'NONE', #34372, 2.499999999999997335 ) ;
#11767 = CARTESIAN_POINT ( 'NONE',  ( 28.26746793355466281, 5.196152422706636465, 167.4886783261892162 ) ) ;
#11768 = CARTESIAN_POINT ( 'NONE',  ( -1.715153634034442431, 41.27731371789855075, 9.534712964251900402 ) ) ;
#11769 = CARTESIAN_POINT ( 'NONE',  ( 28.16288104225748512, -5.196152422706638241, 166.2932446884790920 ) ) ;
#11770 = ORIENTED_EDGE ( 'NONE', *, *, #6322, .F. ) ;
#11771 = VERTEX_POINT ( 'NONE', #30464 ) ;
#11772 = CARTESIAN_POINT ( 'NONE',  ( 15.00000000000000000, 240.1187500012290172, -3.464101615137752166 ) ) ;
#11773 = CARTESIAN_POINT ( 'NONE',  ( 12.53471296425189330, 38.97731371789854649, 2.311890736173451533 ) ) ;
#11774 = CARTESIAN_POINT ( 'NONE',  ( 16.56230152254411436, -7.209453229046482114, -7.734374999385493332 ) ) ;
#11775 = CARTESIAN_POINT ( 'NONE',  ( 20.00041297495057080, 5.668978411116884608, -10.25260147226209995 ) ) ;
#11776 = CARTESIAN_POINT ( 'NONE',  ( 10.69584247140429589, 11.95231371789853902, 6.932735513424201024 ) ) ;
#11777 = VERTEX_POINT ( 'NONE', #30077 ) ;
#11778 = CARTESIAN_POINT ( 'NONE',  ( 19.68408634441910721, 5.407089921784862696, -4.396874999385541827 ) ) ;
#11779 = CARTESIAN_POINT ( 'NONE',  ( -1.926257025242585782E-15, 197.8906250006145342, -31.45816453501075927 ) ) ;
#11780 = CARTESIAN_POINT ( 'NONE',  ( 28.12898775289485442, 5.407089921784862696, 167.3031667422204691 ) ) ;
#11781 = CARTESIAN_POINT ( 'NONE',  ( -62.26711230271183695, 218.4690446883607535, -2.393094931466363651 ) ) ;
#11782 = CARTESIAN_POINT ( 'NONE',  ( 18.12178482187499640, 248.3218750006145115, -4.985214923628404904 ) ) ;
#11783 = CARTESIAN_POINT ( 'NONE',  ( -24.63748681676955954, 195.0000000000001137, -11.14284646165792481 ) ) ;
#11784 = CARTESIAN_POINT ( 'NONE',  ( -58.90252896937851546, 207.6499508600178387, -3.839350919129087547 ) ) ;
#11785 = CARTESIAN_POINT ( 'NONE',  ( -37.73288769728821279, 203.5309553116391612, -1.857196546604028775 ) ) ;
#11786 = CARTESIAN_POINT ( 'NONE',  ( 37.64663378759995283, 7.646167579472015790E-16, 168.6349671354342092 ) ) ;
#11787 = VERTEX_POINT ( 'NONE', #885 ) ;
#11788 = CARTESIAN_POINT ( 'NONE',  ( -28.92959262791929476, 202.2584803510073641, 2.084043131378895186 ) ) ;
#11789 = CARTESIAN_POINT ( 'NONE',  ( -14.38691631536193860, 16.26481371789853370, -5.770363421894132649 ) ) ;
#11790 = CARTESIAN_POINT ( 'NONE',  ( -64.25372103062157692, 218.5309553116391896, -2.162041339862839084 ) ) ;
#11791 = CARTESIAN_POINT ( 'NONE',  ( -8.715434833791929847, 13.86018628210145032, -8.962234695871762469 ) ) ;
#11792 = ADVANCED_FACE ( 'NONE', ( #18342 ), #4483, .F. ) ;
#11793 = CARTESIAN_POINT ( 'NONE',  ( -7.228626920339069173, 57.27268628210144641, 10.49813415415989581 ) ) ;
#11794 = CARTESIAN_POINT ( 'NONE',  ( 22.56230152254411436, 3.464101615137759271, -3.787500000000046718 ) ) ;
#11795 = EDGE_LOOP ( 'NONE', ( #35466, #7229, #18055, #35121 ) ) ;
#11796 = CARTESIAN_POINT ( 'NONE',  ( -36.54538769728823411, 211.8571965466040012, -6.469044688360769513 ) ) ;
#11797 = CARTESIAN_POINT ( 'NONE',  ( 1.120210788295102201E-13, 195.5000000012290400, -27.00000000000000711 ) ) ;
#11798 = CARTESIAN_POINT ( 'NONE',  ( 6.594114490232313663, 18.46018628210144286, 6.840914352312096547 ) ) ;
#11799 = CARTESIAN_POINT ( 'NONE',  ( 5.778771075727756162E-15, 195.0218750006145569, 31.45816453501075927 ) ) ;
#11800 = CARTESIAN_POINT ( 'NONE',  ( 34.27405118538959528, -5.196152422706629359, 167.3019595815335947 ) ) ;
#11801 = CARTESIAN_POINT ( 'NONE',  ( 14.99999999999965539, 3.464101615137553658, -4.031249998770945808 ) ) ;
#11802 = EDGE_CURVE ( 'NONE', #11864, #15590, #3920, .T. ) ;
#11803 = CARTESIAN_POINT ( 'NONE',  ( 37.19400013225076407, 3.464101615137916035, 166.2559890285434392 ) ) ;
#11804 = CARTESIAN_POINT ( 'NONE',  ( 23.87821517812500005, 244.6093750006145342, 4.985214923628404016 ) ) ;
#11805 = CARTESIAN_POINT ( 'NONE',  ( 5.529263428287300108, 95.32731371789854791, 7.954856959092309943 ) ) ;
#11806 = CARTESIAN_POINT ( 'NONE',  ( 20.99999999999999645, 240.2968750006145342, -6.646953231504538984 ) ) ;
#11807 = VERTEX_POINT ( 'NONE', #15684 ) ;
#11808 = CARTESIAN_POINT ( 'NONE',  ( -55.14955436395487709, 214.8429017333601792, -4.673758765035196383 ) ) ;
#11809 = CARTESIAN_POINT ( 'NONE',  ( 18.00000000000000355, 245.6312500012290343, 5.196152422706632912 ) ) ;
#11810 = CARTESIAN_POINT ( 'NONE',  ( -12.46528703574811558, 98.20231371789856212, 2.660918448318004170 ) ) ;
#11811 = CARTESIAN_POINT ( 'NONE',  ( 22.80587116629412492, 3.604726614523243278, -1.284374999385501814 ) ) ;
#11812 = CARTESIAN_POINT ( 'NONE',  ( 19.39230484541324984, 246.9424038105676118, 5.999999999999991118 ) ) ;
#11813 = CARTESIAN_POINT ( 'NONE',  ( 26.75643035624999655, 7.049594010296217766E-16, -2.728124999385489247 ) ) ;
#11814 = CARTESIAN_POINT ( 'NONE',  ( 4.944772684328420986, 68.01481371789854791, 11.48171059495408208 ) ) ;
#11815 = CARTESIAN_POINT ( 'NONE',  ( -27.24356964374999990, 197.5718750006145399, -15.72908226750537786 ) ) ;
#11816 = EDGE_LOOP ( 'NONE', ( #15750, #25316, #14668, #21821, #9589, #21843 ) ) ;
#11817 = VECTOR ( 'NONE', #33679, 1000.000000000000000 ) ;
#11818 = VERTEX_POINT ( 'NONE', #1075 ) ;
#11819 = VERTEX_POINT ( 'NONE', #26856 ) ;
#11820 = CARTESIAN_POINT ( 'NONE',  ( 18.12178482187500350, -4.985214923628407568, -5.015624999385459581 ) ) ;
#11821 = CARTESIAN_POINT ( 'NONE',  ( -27.00000000000000355, 195.4625000000000057, -15.58845726811989429 ) ) ;
#11822 = CARTESIAN_POINT ( 'NONE',  ( 23.87821517812499650, 247.7968750006145058, -4.985214923628404904 ) ) ;
#11823 = CARTESIAN_POINT ( 'NONE',  ( -6.932735513423968321, 32.54768628210144499, -10.69584247140445221 ) ) ;
#11824 = CARTESIAN_POINT ( 'NONE',  ( -53.16294563604516554, 214.6737587650350747, -4.842901733360248429 ) ) ;
#11825 = CARTESIAN_POINT ( 'NONE',  ( 13.90958069845121869, 212.6589072380886023, -5.392997762646073667 ) ) ;
#11826 = CARTESIAN_POINT ( 'NONE',  ( -35.15252896937850124, 207.6499508600178387, -3.839350919129087547 ) ) ;
#11827 = CARTESIAN_POINT ( 'NONE',  ( 24.89975635843425650, 3.464101615137752166, 163.4166986189574402 ) ) ;
#11828 = CARTESIAN_POINT ( 'NONE',  ( 10.69584247140429589, 94.75231371789854506, 6.932735513424201024 ) ) ;
#11829 = CARTESIAN_POINT ( 'NONE',  ( -62.27455436395490551, 206.6211998817774997, 3.209657149897401585 ) ) ;
#11830 = CARTESIAN_POINT ( 'NONE',  ( -66.62872103062152007, 203.4690446883607535, 1.626142955000567936 ) ) ;
#11831 = CARTESIAN_POINT ( 'NONE',  ( 26.75643035624999655, 3.323476615752271268, -5.390624999385473792 ) ) ;
#11832 = CARTESIAN_POINT ( 'NONE',  ( 13.56230152254411614, -5.196152422706638241, -5.325000000000079226 ) ) ;
#11833 = CARTESIAN_POINT ( 'NONE',  ( 14.38691631536194393, 76.06481371789855928, 5.770363421894124656 ) ) ;
#11834 = CARTESIAN_POINT ( 'NONE',  ( -62.86086230271182984, 214.1499508600178387, -7.418979330068641964 ) ) ;
#11835 = AXIS2_PLACEMENT_3D ( 'NONE', #13973, #11122, #24273 ) ;
#11836 = VERTEX_POINT ( 'NONE', #10361 ) ;
#11837 = DIRECTION ( 'NONE',  ( 0.000000000000000000, 1.000000000000000000, 0.000000000000000000 ) ) ;
#11838 = CARTESIAN_POINT ( 'NONE',  ( 8.715434833791931624, 101.2601862821014578, 8.962234695871760692 ) ) ;
#11839 = CARTESIAN_POINT ( 'NONE',  ( 8.927990412390657937, 52.67268628210144499, -13.04141134922759804 ) ) ;
#11840 = VECTOR ( 'NONE', #34683, 1000.000000000000000 ) ;
#11841 = CARTESIAN_POINT ( 'NONE',  ( 15.00000000000000000, 0.000000000000000000, -5.793749998770941545 ) ) ;
#11842 = CYLINDRICAL_SURFACE ( 'NONE', #10716, 5.999999999999999112 ) ;
#11843 = CARTESIAN_POINT ( 'NONE',  ( -6.092822981423970496, 66.18518628210145494, 14.25334919248782661 ) ) ;
#11844 = FACE_OUTER_BOUND ( 'NONE', #22783, .T. ) ;
#11845 = CARTESIAN_POINT ( 'NONE',  ( 22.80587116629411071, 3.604726614523238837, -9.328124999385510208 ) ) ;
#11846 = CARTESIAN_POINT ( 'NONE',  ( 24.70692427760507570, 0.000000000000000000, 161.2126178494294493 ) ) ;
#11847 = CARTESIAN_POINT ( 'NONE',  ( -47.23288769728823411, 203.5309553116391612, -1.857196546604028775 ) ) ;
#11848 = CARTESIAN_POINT ( 'NONE',  ( 12.03223749450566160, 4.087220715173740082, -9.999999999999998224 ) ) ;
#11849 = CARTESIAN_POINT ( 'NONE',  ( 4.944772684328679446, 43.18518628210144072, -11.48171059495397373 ) ) ;
#11850 = CARTESIAN_POINT ( 'NONE',  ( 26.99999999999999645, 196.2125000000000057, -15.58845726811990495 ) ) ;
#11851 = CARTESIAN_POINT ( 'NONE',  ( 1.069080835302379631E-14, 197.9750000012290343, 27.00000000000000000 ) ) ;
#11852 = CARTESIAN_POINT ( 'NONE',  ( -2.064181346179269738, 10.69768628210143646, 9.465287035748067623 ) ) ;
#11853 = CARTESIAN_POINT ( 'NONE',  ( 15.24356964375000167, 245.8468750006145171, 3.323476615752272600 ) ) ;
#11854 = ORIENTED_EDGE ( 'NONE', *, *, #18430, .T. ) ;
#11855 = CARTESIAN_POINT ( 'NONE',  ( 26.99999999999999645, 7.347880794884117764E-16, -3.824999999999994849 ) ) ;
#11856 = CARTESIAN_POINT ( 'NONE',  ( 28.20210112649392542, -5.196152422706638241, 166.7415323026203851 ) ) ;
#11857 = DIRECTION ( 'NONE',  ( -0.9925324990730152175, 0.1219804832088933616, 0.000000000000000000 ) ) ;
#11858 = CARTESIAN_POINT ( 'NONE',  ( 10.31873187879411091, 3.604726614523236616, -3.328124999385545291 ) ) ;
#11859 = CARTESIAN_POINT ( 'NONE',  ( 24.99130137175887612, 0.000000000000000000, 167.2577111570525972 ) ) ;
#11860 = CARTESIAN_POINT ( 'NONE',  ( 15.00000000000000000, 241.4499999999999886, 0.000000000000000000 ) ) ;
#11861 = CARTESIAN_POINT ( 'NONE',  ( -1.909035429704832693E-15, 198.9875000000000114, -31.17691453623979214 ) ) ;
#11862 = CARTESIAN_POINT ( 'NONE',  ( -2.660918448318275509, 65.89768628210146062, 12.46528703574805874 ) ) ;
#11863 = EDGE_LOOP ( 'NONE', ( #19937, #26774, #36032, #6116 ) ) ;
#11864 = VERTEX_POINT ( 'NONE', #27235 ) ;
#11865 = DIRECTION ( 'NONE',  ( -0.000000000000000000, 1.000000000000000000, -0.000000000000000000 ) ) ;
#11866 = CARTESIAN_POINT ( 'NONE',  ( 26.99999999999999645, 246.5874999999999773, 3.464101615137751278 ) ) ;
#11867 = CARTESIAN_POINT ( 'NONE',  ( 21.00000000000000355, 0.000000000000000000, 50.00000000000001421 ) ) ;
#11868 = CARTESIAN_POINT ( 'NONE',  ( 21.00000000000000000, 6.646953231504538984, -6.103124999385481253 ) ) ;
#11869 = CARTESIAN_POINT ( 'NONE',  ( -3.257655550456946880, 45.30231371789854933, -15.46528703574811736 ) ) ;
#11870 = CARTESIAN_POINT ( 'NONE',  ( 26.99999999999999645, 249.3624999999999829, -3.464101615137755275 ) ) ;
#11871 = CARTESIAN_POINT ( 'NONE',  ( 15.24356964374999990, 241.2718750006145569, -3.323476615752268604 ) ) ;
#11872 = B_SPLINE_CURVE_WITH_KNOTS ( 'NONE', 3,
 ( #97, #12036, #8827, #35149, #23235, #9011, #9201, #11661, #17552, #20399, #20769, #23794, #34597, #20581, #20207, #11848, #14698, #32313, #26069, #11482, #34783, #28907 ),
 .UNSPECIFIED., .F., .F.,
 ( 4, 2, 2, 2, 2, 2, 2, 2, 2, 2, 4 ),
 ( 0.000000000000000000, 0.001510400339957781394, 0.002265600509936672741, 0.003020800679915564089, 0.004531201019873346350, 0.005286401189852237698, 0.006041601359831129912, 0.007552001699788915209, 0.009062402039746699639, 0.01057280237970448580, 0.01208320271966227023 ),
 .UNSPECIFIED. ) ;
#11873 = CARTESIAN_POINT ( 'NONE',  ( -61.27752896937849414, 212.3500491399821613, 3.839350919129088435 ) ) ;
#11874 = FACE_OUTER_BOUND ( 'NONE', #25613, .T. ) ;
#11875 = CARTESIAN_POINT ( 'NONE',  ( 37.30512370425429935, -3.464101615137751278, 167.5261372686103982 ) ) ;
#11876 = CARTESIAN_POINT ( 'NONE',  ( 9.465287035748106703, 20.00231371789855217, -2.064181346179063237 ) ) ;
#11877 = CARTESIAN_POINT ( 'NONE',  ( -65.04538769728824832, 211.8571965466039444, -6.469044688360768625 ) ) ;
#11878 = ADVANCED_FACE ( 'NONE', ( #24209, #4112 ), #6970, .T. ) ;
#11879 = CARTESIAN_POINT ( 'NONE',  ( -43.26711230271184405, 218.4690446883607535, -2.393094931466363651 ) ) ;
#11880 = APPLICATION_PROTOCOL_DEFINITION ( 'draft international standard', 'automotive_design', 1998, #25034 ) ;
#11881 = CARTESIAN_POINT ( 'NONE',  ( 10.56230152254403443, 3.464101615137706425, -4.424999998771029119 ) ) ;
#11882 = CARTESIAN_POINT ( 'NONE',  ( 27.24356964375000700, 195.5468750006145342, 15.72908226750537075 ) ) ;
#11883 = CARTESIAN_POINT ( 'NONE',  ( -15.50000000000000533, 126.0898137178985650, 0.1745138560722471477 ) ) ;
#11884 = CARTESIAN_POINT ( 'NONE',  ( -52.96502896937850124, 215.5714017266979567, -3.350049139982168800 ) ) ;
#11885 = ORIENTED_EDGE ( 'NONE', *, *, #128, .T. ) ;
#11886 = CARTESIAN_POINT ( 'NONE',  ( 2.660918448318279950, 52.09768628210144215, -12.46528703574805697 ) ) ;
#11887 = CARTESIAN_POINT ( 'NONE',  ( 37.33780710767756972, 7.347880794884125653E-16, 167.8997102791704492 ) ) ;
#11888 = CARTESIAN_POINT ( 'NONE',  ( 22.56230152254412147, 7.347880794884125653E-16, -8.775000000000032330 ) ) ;
#11889 = CARTESIAN_POINT ( 'NONE',  ( 24.40300010821222898, 0.000000000000000000, 160.5333969449332869 ) ) ;
#11890 = CARTESIAN_POINT ( 'NONE',  ( 21.00000000000000000, -6.928203230275506996, -1.631249998770951004 ) ) ;
#11891 = CARTESIAN_POINT ( 'NONE',  ( 19.68408634441912142, -5.407089921784861808, -8.146874999385516958 ) ) ;
#11892 = CARTESIAN_POINT ( 'NONE',  ( -67.42038769728823411, 208.1428034533959703, 6.469044688360771289 ) ) ;
#11893 = CARTESIAN_POINT ( 'NONE',  ( 22.80587116629411071, -3.604726614523235284, -1.303124999385484095 ) ) ;
#11894 = CARTESIAN_POINT ( 'NONE',  ( 9.534712964251941258, 63.02268628210144641, -1.715153634034235708 ) ) ;
#11895 = CARTESIAN_POINT ( 'NONE',  ( 10.49999999999999645, 244.5000000000000000, 5.000000000000000000 ) ) ;
#11896 = CARTESIAN_POINT ( 'NONE',  ( 26.99999999999999645, 245.6875000000000000, 3.464101615137751278 ) ) ;
#11897 = EDGE_CURVE ( 'NONE', #14950, #25042, #32959, .T. ) ;
#11898 = CARTESIAN_POINT ( 'NONE',  ( 2.311890736173175753, 92.92268628210145209, 12.53471296425194836 ) ) ;
#11899 = FACE_OUTER_BOUND ( 'NONE', #36746, .T. ) ;
#11900 = B_SPLINE_CURVE_WITH_KNOTS ( 'NONE', 3,
 ( #33164, #10414, #27664, #21801, #33353, #4903, #16297, #12694, #7762, #30700, #24266, #15735, #18962, #27285, #27845, #35810, #36554, #19342, #30516, #1316 ),
 .UNSPECIFIED., .F., .F.,
 ( 4, 2, 2, 2, 2, 2, 2, 2, 2, 4 ),
 ( 0.000000000000000000, 0.002984115787595702056, 0.005968231575191402377, 0.008952347362787101831, 0.01044440525658495156, 0.01119043420348387642, 0.01156344867693333799, 0.01174995591365806703, 0.01184320953202043329, 0.01193646315038279955 ),
 .UNSPECIFIED. ) ;
#11901 = ORIENTED_EDGE ( 'NONE', *, *, #12401, .T. ) ;
#11902 = CARTESIAN_POINT ( 'NONE',  ( 36.86550044322413555, 3.604726614523238837, 159.7065721537869365 ) ) ;
#11903 = CARTESIAN_POINT ( 'NONE',  ( 26.75643035624999655, -3.323476615752267715, -7.603124999385488358 ) ) ;
#11904 = CARTESIAN_POINT ( 'NONE',  ( 27.24356964374999279, 195.6218750006145228, -15.72908226750539207 ) ) ;
#11905 = CARTESIAN_POINT ( 'NONE',  ( 27.98518077736123288, -5.407089921784865361, 165.6594454903691087 ) ) ;
#11906 = CARTESIAN_POINT ( 'NONE',  ( 30.97824309782176044, 6.928203230275514990, 164.0518404977788407 ) ) ;
#11907 = DIRECTION ( 'NONE',  ( -1.000000000000000000, 0.000000000000000000, 0.000000000000000000 ) ) ;
#11908 = CARTESIAN_POINT ( 'NONE',  ( 21.00000000000000000, 247.4125000000000227, 6.928203230275506996 ) ) ;
#11909 = CARTESIAN_POINT ( 'NONE',  ( 27.24356964375000700, 198.1906250006145740, 15.72908226750537075 ) ) ;
#11910 = ADVANCED_FACE ( 'NONE', ( #31017 ), #5403, .F. ) ;
#11911 = CARTESIAN_POINT ( 'NONE',  ( 4.622313124798831829, 119.7648137178985763, -11.61527771782809282 ) ) ;
#11912 = CARTESIAN_POINT ( 'NONE',  ( -4.622313124798576922, 115.6351862821014578, -11.61527771782819762 ) ) ;
#11914 = ORIENTED_EDGE ( 'NONE', *, *, #2844, .F. ) ;
#11913 = EDGE_LOOP ( 'NONE', ( #17620, #33273, #10086, #35719 ) ) ;
#11915 = CARTESIAN_POINT ( 'NONE',  ( 13.62178482187499640, 195.1531250006145513, -23.59362340125807123 ) ) ;
#11916 = CARTESIAN_POINT ( 'NONE',  ( 21.00000000000000000, 243.3343750006145285, -6.646953231504538984 ) ) ;
#11917 = AXIS2_PLACEMENT_3D ( 'NONE', #29729, #30116, #15908 ) ;
#11918 = CARTESIAN_POINT ( 'NONE',  ( 8.927990412390371944, 86.12731371789853085, 13.04141134922778811 ) ) ;
#11919 = CARTESIAN_POINT ( 'NONE',  ( 23.87821517812499650, 4.985214923628404904, -3.103124999385475924 ) ) ;
#11920 = CARTESIAN_POINT ( 'NONE',  ( 15.24356964374999990, 246.7093750006145569, 0.000000000000000000 ) ) ;
#11921 = CARTESIAN_POINT ( 'NONE',  ( -1.909035429704832693E-15, 196.4000000012290457, -31.17691453623979214 ) ) ;
#11922 = CARTESIAN_POINT ( 'NONE',  ( 6.840914352311949109, 76.63981371789854791, 6.594114490232462877 ) ) ;
#11923 = CARTESIAN_POINT ( 'NONE',  ( 10.31873187879411091, 0.000000000000000000, -4.640624999385528859 ) ) ;
#11924 =( BOUNDED_SURFACE ( )  B_SPLINE_SURFACE ( 1, 2, ( 
 ( #6916, #36081, #9566, #33062, #12595, #35704, #18487, #26995, #32679, #7107, #18676, #4244, #27369, #24531, #1399, #7287, #6722, #18860, #29836, #12215, #23787, #9754, #35326, #3872, #15445, #24160, #13342, #25084, #8219, #24899, #19419, #36450, #28298, #33430, #27746, #1775, #2144, #10490, #25273, #22069, #33620, #7471, #5173, #16381, #16196, #22628, #16750, #36825, #10678, #10308, #1958, #4803, #2336, #25457, #19049, #30601, #22257, #28114, #19605, #13724, #13907, #22440, #7661, #19238, #36639, #30780, #11052, #4618, #16568, #10867, #37009, #8030, #21879, #13529, #27927, #33809, #7846, #30968, #4985, #24712, #33987, #31153, #34175, #19794, #31330, #5358, #16936, #1588, #13157, #36264, #31514, #8403, #25826, #23180, #3073, #29220, #231, #34913, #19971, #415, #25640, #11794, #8958, #14455, #31885, #5538, #5915, #22809, #2699, #26011, #35097, #14275, #8771, #37374, #17683, #34358, #17125, #28662, #29029, #11426, #14643, #22993, #34543, #8582, #32071, #5726, #20152, #11980, #6099, #26193, #40, #37194, #28849, #31700, #3263, #14835, #17308, #2883, #11605, #17494, #20529, #23363, #26380, #23553, #34727, #20343, #9146, #20713, #32256, #6299, #28479, #2520, #14088, #11237, #598, #29794, #3641, #12362, #29605, #26569, #18062, #3448, #15589, #6677, #4016, #23932, #12167, #26760, #15405, #35279, #791, #15211, #20906, #9338, #35474, #29985, #6490, #15781, #32446, #10085, #9893, #3826, #23741, #27142, #24494, #9525, #26949, #979, #21097, #32637, #24121, #6868, #12555, #18250, #35664, #21477, #9713, #21288, #1169, #24309, #36041, #18636, #7067, #17871, #18443, #30176, #15019, #32823, #12741, #35852, #33016, #4204, #27331, #1361, #12932, #21655, #33208, #29416, #10267, #30926, #13685, #16338, #15969, #7619, #10452, #22399, #31112, #24672, #13118, #27887, #33767, #25233, #7807, #10827, #28072, #7435, #4580, #4764, #30562, #16713, #36225, #22216, #19383, #7989, #36782, #27521, #19195, #16156, #1733, #19004, #1546, #27705, #30366, #4943, #33581, #16525, #13302, #21842, #24860, #1917, #33395, #36408, #22028, #30743, #13485, #25041, #2106, #36597, #5132 ),
 ( #10637, #33948, #19563, #28260, #2292, #13867, #25416, #36969, #11012, #22586, #7248, #18822, #4389, #3555, #15308, #35381, #23842, #34131, #23652, #9431, #19754, #5498, #14932, #23461, #29324, #21009, #37155, #17971, #35015, #20629, #3362, #11893, #11197, #20817, #15117, #26479, #9244, #32543, #6398, #26668, #25600, #6585, #31293, #29514, #698, #32172, #510, #22770, #12078, #28436, #8364, #6209, #3735, #19934, #35195, #31474, #18160, #2477, #34318, #17081, #32359, #28620, #12270, #2657, #14234, #14050, #29701, #9058, #26292, #26860, #890, #12461, #8180, #5321, #328, #16897, #17781, #27421, #7344, #21569, #21753, #18917, #4299, #36136, #30274, #18346, #3924, #1455, #35759, #15878, #30082, #4116, #21940, #29894, #36318, #13028, #15498, #27053, #33114, #30468, #24584, #15689, #1079, #35575, #27240, #33485, #27614, #7159, #18732, #10365, #10177, #12649, #7530, #30654, #1263, #12834, #33304, #27802, #4489, #19103, #16066, #13217, #1645, #24401, #21196, #24766, #35949, #4669, #9988, #32922, #16252, #1829, #24030, #9619, #32734, #24214, #6771, #9804, #21382, #6974, #18543, #4858, #13960, #5232, #22125, #31568, #8453, #25509, #2198, #5590, #10551, #37062, #30834, #11109, #13778, #22496, #25326, #22685, #28718, #17177, #31387, #34229, #19295, #16989, #7902, #34043, #13399, #36875, #36695, #22865, #16437, #2386, #28529, #24948, #2572, #8089, #34415, #37248, #8272, #20022, #16626, #7713, #36506, #27984, #19475, #14142, #2014, #10921, #13591, #25696, #33673, #19845, #5407, #25141, #10735, #11297, #22308, #19663, #33860, #31204, #31022, #5044, #28168, #16807, #28349, #20396, #6158, #6539, #32122, #15070, #3312, #29466, #12033, #3127, #37429, #26431, #29085, #34965, #31937, #11656, #23601, #14884, #17732, #20960, #29273, #2940, #9008, #465, #28904, #6351, #23049, #31753, #35146, #9198, #11478, #32492, #35330, #20766, #14694, #18112, #34593, #32310, #20204, #17921, #26244, #11845, #279, #3501, #2755, #14327, #26620, #650, #8636, #12220, #34780, #23415, #25881, #20578, #26066, #23791, #5783, #9385, #17363, #14510, #94, #23232, #8823, #5969, #17549 ) ),
 .UNSPECIFIED., .F., .F., .F. ) 
 B_SPLINE_SURFACE_WITH_KNOTS ( ( 2, 2 ),
 ( 3, 2, 2, 2, 2, 2, 2, 2, 2, 2, 2, 2, 2, 2, 2, 2, 2, 2, 2, 2, 2, 2, 2, 2, 2, 2, 2, 2, 2, 2, 2, 2, 2, 2, 2, 2, 2, 2, 2, 2, 2, 2, 2, 2, 2, 2, 2, 2, 2, 2, 2, 2, 2, 2, 2, 2, 2, 2, 2, 2, 2, 2, 2, 2, 2, 2, 2, 2, 2, 2, 2, 2, 2, 2, 2, 2, 2, 2, 2, 2, 2, 2, 2, 2, 2, 2, 2, 2, 2, 2, 2, 2, 2, 2, 2, 2, 2, 2, 2, 2, 2, 2, 2, 2, 2, 2, 2, 2, 2, 2, 2, 2, 2, 2, 2, 2, 2, 2, 2, 2, 2, 2, 2, 2, 2, 2, 2, 2, 2, 2, 2, 2, 2, 2, 3 ),
 ( 0.000000000000000000, 1.000000000000000000 ),
 ( 0.000000000000000000, 0.007246376811594202987, 0.01449275362318840597, 0.02173913043478260809, 0.02898550724637681195, 0.03623188405797101580, 0.04347826086956521618, 0.05072463768115942351, 0.05797101449275362389, 0.06521739130434782428, 0.07246376811594203160, 0.07971014492753622505, 0.08695652173913043237, 0.09420289855072463969, 0.1014492753623188470, 0.1086956521739130405, 0.1159420289855072478, 0.1231884057971014551, 0.1304347826086956486, 0.1376811594202898559, 0.1449275362318840632, 0.1521739130434782705, 0.1594202898550724501, 0.1666666666666666574, 0.1739130434782608647, 0.1811594202898550721, 0.1884057971014492794, 0.1956521739130434867, 0.2028985507246376940, 0.2101449275362318736, 0.2173913043478260809, 0.2246376811594202882, 0.2318840579710144956, 0.2391304347826087029, 0.2463768115942029102, 0.2536231884057971175, 0.2608695652173912971, 0.2681159420289855322, 0.2753623188405797118, 0.2826086956521738913, 0.2898550724637681264, 0.2971014492753623060, 0.3043478260869565410, 0.3115942028985507206, 0.3188405797101449002, 0.3260869565217391353, 0.3333333333333333148, 0.3405797101449275499, 0.3478260869565217295, 0.3550724637681159646, 0.3623188405797101441, 0.3695652173913043237, 0.3768115942028985588, 0.3840579710144927383, 0.3913043478260869734, 0.3985507246376811530, 0.4057971014492753881, 0.4130434782608695676, 0.4202898550724637472, 0.4275362318840579823, 0.4347826086956521618, 0.4420289855072463969, 0.4492753623188405765, 0.4565217391304347561, 0.4637681159420289911, 0.4710144927536231707, 0.4782608695652174058, 0.4855072463768115854, 0.4927536231884058204, 0.5000000000000000000, 0.5072463768115942351, 0.5144927536231883591, 0.5217391304347825942, 0.5289855072463768293, 0.5362318840579710644, 0.5434782608695651884, 0.5507246376811594235, 0.5579710144927536586, 0.5652173913043477826, 0.5724637681159420177, 0.5797101449275362528, 0.5869565217391304879, 0.5942028985507246119, 0.6014492753623188470, 0.6086956521739130821, 0.6159420289855072062, 0.6231884057971014412, 0.6304347826086956763, 0.6376811594202898004, 0.6449275362318840354, 0.6521739130434782705, 0.6594202898550725056, 0.6666666666666666297, 0.6739130434782608647, 0.6811594202898550998, 0.6884057971014492239, 0.6956521739130434590, 0.7028985507246376940, 0.7101449275362319291, 0.7173913043478260532, 0.7246376811594202882, 0.7318840579710145233, 0.7391304347826086474, 0.7463768115942028825, 0.7536231884057971175, 0.7608695652173913526, 0.7681159420289854767, 0.7753623188405797118, 0.7826086956521739468, 0.7898550724637680709, 0.7971014492753623060, 0.8043478260869565410, 0.8115942028985507761, 0.8188405797101449002, 0.8260869565217391353, 0.8333333333333333703, 0.8405797101449274944, 0.8478260869565217295, 0.8550724637681159646, 0.8623188405797101996, 0.8695652173913043237, 0.8768115942028985588, 0.8840579710144927938, 0.8913043478260869179, 0.8985507246376811530, 0.9057971014492753881, 0.9130434782608695121, 0.9202898550724637472, 0.9275362318840579823, 0.9347826086956522174, 0.9420289855072463414, 0.9492753623188405765, 0.9565217391304348116, 0.9637681159420289356, 0.9662082948456578446 ),
 .UNSPECIFIED. ) 
 GEOMETRIC_REPRESENTATION_ITEM ( )  RATIONAL_B_SPLINE_SURFACE ( (
 ( 1.000000000000000000, 0.8660254037844387076, 1.000000000000000000, 0.8660254037844387076, 1.000000000000000000, 0.8660254037844387076, 1.000000000000000000, 0.8660254037844387076, 1.000000000000000000, 0.8660254037844387076, 1.000000000000000000, 0.8660254037844387076, 1.000000000000000000, 0.8660254037844387076, 1.000000000000000000, 0.8660254037844387076, 1.000000000000000000, 0.8660254037844387076, 1.000000000000000000, 0.8660254037844387076, 1.000000000000000000, 0.8660254037844387076, 1.000000000000000000, 0.8660254037844387076, 1.000000000000000000, 0.8660254037844387076, 1.000000000000000000, 0.8660254037844387076, 1.000000000000000000, 0.8660254037844387076, 1.000000000000000000, 0.8660254037844387076, 1.000000000000000000, 0.8660254037844387076, 1.000000000000000000, 0.8660254037844387076, 1.000000000000000000, 0.8660254037844387076, 1.000000000000000000, 0.8660254037844387076, 1.000000000000000000, 0.8660254037844387076, 1.000000000000000000, 0.8660254037844387076, 1.000000000000000000, 0.8660254037844387076, 1.000000000000000000, 0.8660254037844387076, 1.000000000000000000, 0.8660254037844387076, 1.000000000000000000, 0.8660254037844387076, 1.000000000000000000, 0.8660254037844387076, 1.000000000000000000, 0.8660254037844387076, 1.000000000000000000, 0.8660254037844387076, 1.000000000000000000, 0.8660254037844387076, 1.000000000000000000, 0.8660254037844387076, 1.000000000000000000, 0.8660254037844387076, 1.000000000000000000, 0.8660254037844387076, 1.000000000000000000, 0.8660254037844387076, 1.000000000000000000, 0.8660254037844387076, 1.000000000000000000, 0.8660254037844387076, 1.000000000000000000, 0.8660254037844387076, 1.000000000000000000, 0.8660254037844387076, 1.000000000000000000, 0.8660254037844387076, 1.000000000000000000, 0.8660254037844387076, 1.000000000000000000, 0.8660254037844387076, 1.000000000000000000, 0.8660254037844387076, 1.000000000000000000, 0.8660254037844387076, 1.000000000000000000, 0.8660254037844387076, 1.000000000000000000, 0.8660254037844387076, 1.000000000000000000, 0.8660254037844387076, 1.000000000000000000, 0.8660254037844387076, 1.000000000000000000, 0.8660254037844387076, 1.000000000000000000, 0.8660254037844387076, 1.000000000000000000, 0.8660254037844387076, 1.000000000000000000, 0.8660254037844387076, 1.000000000000000000, 0.8660254037844387076, 1.000000000000000000, 0.8660254037844387076, 1.000000000000000000, 0.8660254037844387076, 1.000000000000000000, 0.8660254037844387076, 1.000000000000000000, 0.8660254037844387076, 1.000000000000000000, 0.8660254037844387076, 1.000000000000000000, 0.8660254037844387076, 1.000000000000000000, 0.8660254037844387076, 1.000000000000000000, 0.8660254037844387076, 1.000000000000000000, 0.8660254037844387076, 1.000000000000000000, 0.8660254037844387076, 1.000000000000000000, 0.8660254037844387076, 1.000000000000000000, 0.8660254037844387076, 1.000000000000000000, 0.8660254037844387076, 1.000000000000000000, 0.8660254037844387076, 1.000000000000000000, 0.8660254037844387076, 1.000000000000000000, 0.8660254037844387076, 1.000000000000000000, 0.8660254037844387076, 1.000000000000000000, 0.8660254037844387076, 1.000000000000000000, 0.8660254037844387076, 1.000000000000000000, 0.8660254037844387076, 1.000000000000000000, 0.8660254037844387076, 1.000000000000000000, 0.8660254037844387076, 1.000000000000000000, 0.8660254037844387076, 1.000000000000000000, 0.8660254037844387076, 1.000000000000000000, 0.8660254037844387076, 1.000000000000000000, 0.8660254037844387076, 1.000000000000000000, 0.8660254037844387076, 1.000000000000000000, 0.8660254037844387076, 1.000000000000000000, 0.8660254037844387076, 1.000000000000000000, 0.8660254037844387076, 1.000000000000000000, 0.8660254037844387076, 1.000000000000000000, 0.8660254037844387076, 1.000000000000000000, 0.8660254037844387076, 1.000000000000000000, 0.8660254037844387076, 1.000000000000000000, 0.8660254037844387076, 1.000000000000000000, 0.8660254037844387076, 1.000000000000000000, 0.8660254037844387076, 1.000000000000000000, 0.8660254037844387076, 1.000000000000000000, 0.8660254037844387076, 1.000000000000000000, 0.8660254037844387076, 1.000000000000000000, 0.8660254037844387076, 1.000000000000000000, 0.8660254037844387076, 1.000000000000000000, 0.8660254037844387076, 1.000000000000000000, 0.8660254037844387076, 1.000000000000000000, 0.8660254037844387076, 1.000000000000000000, 0.8660254037844387076, 1.000000000000000000, 0.8660254037844387076, 1.000000000000000000, 0.8660254037844387076, 1.000000000000000000, 0.8660254037844387076, 1.000000000000000000, 0.8660254037844387076, 1.000000000000000000, 0.8660254037844387076, 1.000000000000000000, 0.8660254037844387076, 1.000000000000000000, 0.8660254037844387076, 1.000000000000000000, 0.8660254037844387076, 1.000000000000000000, 0.8660254037844387076, 1.000000000000000000, 0.8660254037844387076, 1.000000000000000000, 0.8660254037844387076, 1.000000000000000000, 0.8660254037844387076, 1.000000000000000000, 0.8660254037844387076, 1.000000000000000000, 0.8660254037844387076, 1.000000000000000000, 0.8660254037844387076, 1.000000000000000000, 0.8660254037844387076, 1.000000000000000000, 0.8660254037844387076, 1.000000000000000000, 0.8660254037844387076, 1.000000000000000000, 0.8660254037844387076, 1.000000000000000000, 0.8660254037844387076, 1.000000000000000000, 0.8660254037844387076, 1.000000000000000000, 0.8660254037844387076, 1.000000000000000000, 0.8660254037844387076, 1.000000000000000000, 0.8660254037844387076, 1.000000000000000000, 0.8660254037844387076, 1.000000000000000000, 0.8660254037844387076, 1.000000000000000000, 0.8660254037844387076, 1.000000000000000000, 0.8660254037844387076, 1.000000000000000000, 0.8660254037844387076, 1.000000000000000000, 0.8660254037844387076, 1.000000000000000000, 0.8660254037844387076, 1.000000000000000000, 0.8660254037844387076, 1.000000000000000000, 0.8660254037844387076, 1.000000000000000000, 0.8660254037844387076, 1.000000000000000000, 0.8660254037844387076, 1.000000000000000000, 0.9548847663035771038, 0.9401541632606846832),
 ( 1.000000000000000000, 0.8660254037844387076, 1.000000000000000000, 0.8660254037844387076, 1.000000000000000000, 0.8660254037844387076, 1.000000000000000000, 0.8660254037844387076, 1.000000000000000000, 0.8660254037844387076, 1.000000000000000000, 0.8660254037844387076, 1.000000000000000000, 0.8660254037844387076, 1.000000000000000000, 0.8660254037844387076, 1.000000000000000000, 0.8660254037844387076, 1.000000000000000000, 0.8660254037844387076, 1.000000000000000000, 0.8660254037844387076, 1.000000000000000000, 0.8660254037844387076, 1.000000000000000000, 0.8660254037844387076, 1.000000000000000000, 0.8660254037844387076, 1.000000000000000000, 0.8660254037844387076, 1.000000000000000000, 0.8660254037844387076, 1.000000000000000000, 0.8660254037844387076, 1.000000000000000000, 0.8660254037844387076, 1.000000000000000000, 0.8660254037844387076, 1.000000000000000000, 0.8660254037844387076, 1.000000000000000000, 0.8660254037844387076, 1.000000000000000000, 0.8660254037844387076, 1.000000000000000000, 0.8660254037844387076, 1.000000000000000000, 0.8660254037844387076, 1.000000000000000000, 0.8660254037844387076, 1.000000000000000000, 0.8660254037844387076, 1.000000000000000000, 0.8660254037844387076, 1.000000000000000000, 0.8660254037844387076, 1.000000000000000000, 0.8660254037844387076, 1.000000000000000000, 0.8660254037844387076, 1.000000000000000000, 0.8660254037844387076, 1.000000000000000000, 0.8660254037844387076, 1.000000000000000000, 0.8660254037844387076, 1.000000000000000000, 0.8660254037844387076, 1.000000000000000000, 0.8660254037844387076, 1.000000000000000000, 0.8660254037844387076, 1.000000000000000000, 0.8660254037844387076, 1.000000000000000000, 0.8660254037844387076, 1.000000000000000000, 0.8660254037844387076, 1.000000000000000000, 0.8660254037844387076, 1.000000000000000000, 0.8660254037844387076, 1.000000000000000000, 0.8660254037844387076, 1.000000000000000000, 0.8660254037844387076, 1.000000000000000000, 0.8660254037844387076, 1.000000000000000000, 0.8660254037844387076, 1.000000000000000000, 0.8660254037844387076, 1.000000000000000000, 0.8660254037844387076, 1.000000000000000000, 0.8660254037844387076, 1.000000000000000000, 0.8660254037844387076, 1.000000000000000000, 0.8660254037844387076, 1.000000000000000000, 0.8660254037844387076, 1.000000000000000000, 0.8660254037844387076, 1.000000000000000000, 0.8660254037844387076, 1.000000000000000000, 0.8660254037844387076, 1.000000000000000000, 0.8660254037844387076, 1.000000000000000000, 0.8660254037844387076, 1.000000000000000000, 0.8660254037844387076, 1.000000000000000000, 0.8660254037844387076, 1.000000000000000000, 0.8660254037844387076, 1.000000000000000000, 0.8660254037844387076, 1.000000000000000000, 0.8660254037844387076, 1.000000000000000000, 0.8660254037844387076, 1.000000000000000000, 0.8660254037844387076, 1.000000000000000000, 0.8660254037844387076, 1.000000000000000000, 0.8660254037844387076, 1.000000000000000000, 0.8660254037844387076, 1.000000000000000000, 0.8660254037844387076, 1.000000000000000000, 0.8660254037844387076, 1.000000000000000000, 0.8660254037844387076, 1.000000000000000000, 0.8660254037844387076, 1.000000000000000000, 0.8660254037844387076, 1.000000000000000000, 0.8660254037844387076, 1.000000000000000000, 0.8660254037844387076, 1.000000000000000000, 0.8660254037844387076, 1.000000000000000000, 0.8660254037844387076, 1.000000000000000000, 0.8660254037844387076, 1.000000000000000000, 0.8660254037844387076, 1.000000000000000000, 0.8660254037844387076, 1.000000000000000000, 0.8660254037844387076, 1.000000000000000000, 0.8660254037844387076, 1.000000000000000000, 0.8660254037844387076, 1.000000000000000000, 0.8660254037844387076, 1.000000000000000000, 0.8660254037844387076, 1.000000000000000000, 0.8660254037844387076, 1.000000000000000000, 0.8660254037844387076, 1.000000000000000000, 0.8660254037844387076, 1.000000000000000000, 0.8660254037844387076, 1.000000000000000000, 0.8660254037844387076, 1.000000000000000000, 0.8660254037844387076, 1.000000000000000000, 0.8660254037844387076, 1.000000000000000000, 0.8660254037844387076, 1.000000000000000000, 0.8660254037844387076, 1.000000000000000000, 0.8660254037844387076, 1.000000000000000000, 0.8660254037844387076, 1.000000000000000000, 0.8660254037844387076, 1.000000000000000000, 0.8660254037844387076, 1.000000000000000000, 0.8660254037844387076, 1.000000000000000000, 0.8660254037844387076, 1.000000000000000000, 0.8660254037844387076, 1.000000000000000000, 0.8660254037844387076, 1.000000000000000000, 0.8660254037844387076, 1.000000000000000000, 0.8660254037844387076, 1.000000000000000000, 0.8660254037844387076, 1.000000000000000000, 0.8660254037844387076, 1.000000000000000000, 0.8660254037844387076, 1.000000000000000000, 0.8660254037844387076, 1.000000000000000000, 0.8660254037844387076, 1.000000000000000000, 0.8660254037844387076, 1.000000000000000000, 0.8660254037844387076, 1.000000000000000000, 0.8660254037844387076, 1.000000000000000000, 0.8660254037844387076, 1.000000000000000000, 0.8660254037844387076, 1.000000000000000000, 0.8660254037844387076, 1.000000000000000000, 0.8660254037844387076, 1.000000000000000000, 0.8660254037844387076, 1.000000000000000000, 0.8660254037844387076, 1.000000000000000000, 0.8660254037844387076, 1.000000000000000000, 0.8660254037844387076, 1.000000000000000000, 0.8660254037844387076, 1.000000000000000000, 0.8660254037844387076, 1.000000000000000000, 0.8660254037844387076, 1.000000000000000000, 0.8660254037844387076, 1.000000000000000000, 0.8660254037844387076, 1.000000000000000000, 0.8660254037844387076, 1.000000000000000000, 0.8660254037844387076, 1.000000000000000000, 0.8660254037844387076, 1.000000000000000000, 0.8660254037844387076, 1.000000000000000000, 0.8660254037844387076, 1.000000000000000000, 0.8660254037844387076, 1.000000000000000000, 0.8660254037844387076, 1.000000000000000000, 0.8660254037844387076, 1.000000000000000000, 0.8660254037844387076, 1.000000000000000000, 0.8660254037844387076, 1.000000000000000000, 0.9548847663035771038, 0.9401541632606846832) ) ) 
 REPRESENTATION_ITEM ( '' )  SURFACE ( )  );
#11925 = CARTESIAN_POINT ( 'NONE',  ( 26.75643035624999655, 241.8718750006145228, -7.049594010296217766E-16 ) ) ;
#11926 = CARTESIAN_POINT ( 'NONE',  ( 8.962234695871567070, 49.03981371789854649, 8.715434833792127023 ) ) ;
#11927 = CARTESIAN_POINT ( 'NONE',  ( -8.962234695871760692, 103.5601862821014549, 8.715434833791933400 ) ) ;
#11928 = CARTESIAN_POINT ( 'NONE',  ( 13.56230152254410370, 5.196152422706630247, -7.162499998770998744 ) ) ;
#11929 = CARTESIAN_POINT ( 'NONE',  ( -67.02455436395489130, 206.6211998817774997, 3.209657149897401585 ) ) ;
#11930 = DIRECTION ( 'NONE',  ( 0.9961946980917459893, 0.000000000000000000, -0.08715574274765348906 ) ) ;
#11931 = CARTESIAN_POINT ( 'NONE',  ( 30.97824309782176755, 6.928203230275514990, 164.0518404977788123 ) ) ;
#11932 = CARTESIAN_POINT ( 'NONE',  ( 8.927990412390657937, 89.47268628210143504, -13.04141134922759804 ) ) ;
#11933 = AXIS2_PLACEMENT_3D ( 'NONE', #10806, #2270, #2455 ) ;
#11934 = CARTESIAN_POINT ( 'NONE',  ( -12.50000000000000355, 3.510186282101451560, -0.1745138560725492671 ) ) ;
#11935 = CARTESIAN_POINT ( 'NONE',  ( 10.56230152254410726, 0.000000000000000000, -8.100000000000024514 ) ) ;
#11936 = ADVANCED_FACE ( 'NONE', ( #13774 ), #30830, .T. ) ;
#11937 = CARTESIAN_POINT ( 'NONE',  ( 20.99999999999997513, 245.3875000000000455, -5.999999999999999112 ) ) ;
#11938 = CARTESIAN_POINT ( 'NONE',  ( -3.796722387233375073, 121.3851862821014578, 8.710071997420127943 ) ) ;
#11939 = CARTESIAN_POINT ( 'NONE',  ( 13.49999999999999645, 199.0625000012290400, -23.38268590217984766 ) ) ;
#11940 =( BOUNDED_CURVE ( )  B_SPLINE_CURVE ( 3, ( #24559, #36109, #13559, #24925 ),
 .UNSPECIFIED., .F., .F. ) 
 B_SPLINE_CURVE_WITH_KNOTS ( ( 4, 4 ),
 ( 0.000000000000000000, 1.570796326794895670 ),
 .UNSPECIFIED. ) 
 CURVE ( )  GEOMETRIC_REPRESENTATION_ITEM ( )  RATIONAL_B_SPLINE_CURVE ( ( 1.000000000000000000, 0.8047378541243652705, 0.8047378541243652705, 1.000000000000000000 ) ) 
 REPRESENTATION_ITEM ( '' )  );
#11941 = CARTESIAN_POINT ( 'NONE',  ( 10.83675517735155225, 9.260186282101427580, 11.08355503943142573 ) ) ;
#11942 = CARTESIAN_POINT ( 'NONE',  ( -27.24356964374999990, 196.6718750006145342, -15.72908226750537786 ) ) ;
#11943 = CARTESIAN_POINT ( 'NONE',  ( 26.75643035624999655, 241.4593750006145285, -3.323476615752271712 ) ) ;
#11944 = ORIENTED_EDGE ( 'NONE', *, *, #10244, .T. ) ;
#11945 = DIRECTION ( 'NONE',  ( -1.000000000000000000, -6.123233995736766036E-17, 0.000000000000000000 ) ) ;
#11946 = CARTESIAN_POINT ( 'NONE',  ( -5.529263428287477744, 48.07268628210143646, 7.954856959092191815 ) ) ;
#11947 = CARTESIAN_POINT ( 'NONE',  ( 26.75643035624999655, -3.323476615752267715, -1.303124999385484095 ) ) ;
#11948 = EDGE_CURVE ( 'NONE', #25619, #19865, #17251, .T. ) ;
#11949 = CYLINDRICAL_SURFACE ( 'NONE', #22148, 5.999999999999999112 ) ;
#11950 = FACE_OUTER_BOUND ( 'NONE', #20514, .T. ) ;
#11951 = CARTESIAN_POINT ( 'NONE',  ( 4.611372152710607075, 195.0000000000000000, 26.85403668788741527 ) ) ;
#11952 = CARTESIAN_POINT ( 'NONE',  ( 10.31873187879410914, 0.000000000000000000, -0.5906249993855583469 ) ) ;
#11953 = CARTESIAN_POINT ( 'NONE',  ( -9.500000000000005329, 43.28981371789856070, 0.1745138560723101806 ) ) ;
#11954 = CARTESIAN_POINT ( 'NONE',  ( -27.24356964375000345, 199.4093750006145456, 0.000000000000000000 ) ) ;
#11955 = ORIENTED_EDGE ( 'NONE', *, *, #28642, .T. ) ;
#11956 = CARTESIAN_POINT ( 'NONE',  ( 24.00000000000000000, 240.3062500012290457, 5.196152422706629359 ) ) ;
#11957 = CARTESIAN_POINT ( 'NONE',  ( 8.715434833792128799, 46.73981371789854933, -8.962234695871567070 ) ) ;
#11958 = CARTESIAN_POINT ( 'NONE',  ( 18.12178482187499640, 4.985214923628404904, -8.878124999385478944 ) ) ;
#11959 = CARTESIAN_POINT ( 'NONE',  ( 12.50000000000000355, 11.08981371789855075, -0.1745138560722771515 ) ) ;
#11960 = EDGE_CURVE ( 'NONE', #29322, #23945, #4853, .T. ) ;
#11961 = CARTESIAN_POINT ( 'NONE',  ( 25.40634911304790577, -3.464101615137787693, 169.2070803003913397 ) ) ;
#11962 = ORIENTED_EDGE ( 'NONE', *, *, #12882, .F. ) ;
#11963 = CARTESIAN_POINT ( 'NONE',  ( 22.80587116629412137, 7.646167579472024665E-16, -4.471874999385533123 ) ) ;
#11964 = CARTESIAN_POINT ( 'NONE',  ( 27.24356964375000345, 198.2281250006145399, -3.336375036156643733E-15 ) ) ;
#11965 = CARTESIAN_POINT ( 'NONE',  ( 28.18128119854344860, -5.407089921784865361, 167.9008835610755455 ) ) ;
#11966 = CARTESIAN_POINT ( 'NONE',  ( -34.55877896937847993, 211.6261429550004607, -6.530955311639245586 ) ) ;
#11967 = AXIS2_PLACEMENT_3D ( 'NONE', #199, #23332, #2668 ) ;
#11968 = CARTESIAN_POINT ( 'NONE',  ( -26.64709556143852964, 195.0000000000000853, -4.774896623102089954 ) ) ;
#11969 = EDGE_CURVE ( 'NONE', #16035, #16919, #19658, .T. ) ;
#11970 = CARTESIAN_POINT ( 'NONE',  ( -51.77752896937850124, 212.3500491399821613, 3.839350919129088435 ) ) ;
#11971 = FACE_OUTER_BOUND ( 'NONE', #8079, .T. ) ;
#11972 = EDGE_LOOP ( 'NONE', ( #31033, #31886, #961, #11119 ) ) ;
#11973 = CARTESIAN_POINT ( 'NONE',  ( 18.00000000000000000, 248.5749999999999886, -5.196152422706630247 ) ) ;
#11974 = CARTESIAN_POINT ( 'NONE',  ( -2.908627838312453306, 13.67731371789853867, 15.53471296425188797 ) ) ;
#11975 = CARTESIAN_POINT ( 'NONE',  ( -55.94122103062156981, 207.8379586601371329, -8.530955311639223382 ) ) ;
#11976 =( BOUNDED_CURVE ( )  B_SPLINE_CURVE ( 2, ( #33401, #33215, #33024, #28079, #19012, #24867, #1368 ),
 .UNSPECIFIED., .F., .F. ) 
 B_SPLINE_CURVE_WITH_KNOTS ( ( 3, 2, 2, 3 ),
 ( 0.1956521739130434034, 0.2028985507246377218, 0.2101449275362319846, 0.2173913043478263030 ),
 .UNSPECIFIED. ) 
 CURVE ( )  GEOMETRIC_REPRESENTATION_ITEM ( )  RATIONAL_B_SPLINE_CURVE ( ( 1.000000000000001554, 0.8660254037844372643, 1.000000000000000000, 0.8660254037844387076, 1.000000000000000000, 0.8660254037844345998, 1.000000000000003997 ) ) 
 REPRESENTATION_ITEM ( '' )  );
#11977 = PRODUCT ( 'extension pipe', 'extension pipe', '', ( #34626 ) ) ;
#11978 = CARTESIAN_POINT ( 'NONE',  ( 8.843639120294328748, 127.1351862821014720, -3.474262827703334722 ) ) ;
#11979 = CARTESIAN_POINT ( 'NONE',  ( 2.660918448318279950, 33.69768628210145067, -12.46528703574805697 ) ) ;
#11980 = CARTESIAN_POINT ( 'NONE',  ( 22.56230152254412857, -3.464101615137755275, -4.762500000000064126 ) ) ;
#11981 = VECTOR ( 'NONE', #22304, 1000.000000000000000 ) ;
#11982 = ORIENTED_EDGE ( 'NONE', *, *, #31483, .F. ) ;
#11983 = CARTESIAN_POINT ( 'NONE',  ( -40.30580436395489841, 216.5000000000000000, 0.1155267958017343610 ) ) ;
#11984 = LINE ( 'NONE', #29224, #22400 ) ;
#11985 = CARTESIAN_POINT ( 'NONE',  ( -2.064181346179269738, 29.09768628210144925, 9.465287035748067623 ) ) ;
#11986 = CARTESIAN_POINT ( 'NONE',  ( 13.62178482187499640, 197.0093750006145399, -23.59362340125807123 ) ) ;
#11987 = CARTESIAN_POINT ( 'NONE',  ( 7.234628195640337545, 198.1799038117967200, -26.99999999999999289 ) ) ;
#11988 = CARTESIAN_POINT ( 'NONE',  ( 22.56230152254410370, 7.347880794884117764E-16, -3.712499998771018106 ) ) ;
#11989 = CYLINDRICAL_SURFACE ( 'NONE', #33984, 5.999999999999998224 ) ;
#11990 = CARTESIAN_POINT ( 'NONE',  ( 28.43415329166666083, 5.196152422706630247, 169.3939006875140194 ) ) ;
#11991 = CARTESIAN_POINT ( 'NONE',  ( 23.87821517812499650, 246.1093750006145342, -4.985214923628404904 ) ) ;
#11992 = CARTESIAN_POINT ( 'NONE',  ( 3.796722387233182339, 86.41481371789855359, 8.710071997420207879 ) ) ;
#11993 = CARTESIAN_POINT ( 'NONE',  ( 15.24356964374999990, 240.4093750006145456, 0.000000000000000000 ) ) ;
#11994 = VECTOR ( 'NONE', #33141, 1000.000000000000000 ) ;
#11995 = ORIENTED_EDGE ( 'NONE', *, *, #32176, .T. ) ;
#11996 = CARTESIAN_POINT ( 'NONE',  ( -52.37872103062156270, 203.4690446883607535, 1.626142955000567936 ) ) ;
#11997 = CARTESIAN_POINT ( 'NONE',  ( 15.00000000000000178, 246.4937500012290457, 3.464101615137757051 ) ) ;
#11998 = CARTESIAN_POINT ( 'NONE',  ( 2.311890736173452421, 101.0773137178985621, -12.53471296425189152 ) ) ;
#11999 = CARTESIAN_POINT ( 'NONE',  ( 16.56230152254411436, 7.209453229046482114, -1.659374999385503591 ) ) ;
#12000 = CARTESIAN_POINT ( 'NONE',  ( 24.36051168362275021, 3.604726614523236616, 160.0477520296136049 ) ) ;
#12001 = CARTESIAN_POINT ( 'NONE',  ( 21.00000000000000000, -6.646953231504538984, -3.290624999385483918 ) ) ;
#12002 = CARTESIAN_POINT ( 'NONE',  ( -10.49813415416004858, 70.02731371789855075, 7.228626920338839135 ) ) ;
#12003 = CARTESIAN_POINT ( 'NONE',  ( 13.62178482187499640, 197.9093750006145456, -23.59362340125807123 ) ) ;
#12004 = ORIENTED_EDGE ( 'NONE', *, *, #11217, .T. ) ;
#12005 = VERTEX_POINT ( 'NONE', #27979 ) ;
#12006 = CARTESIAN_POINT ( 'NONE',  ( 23.87821517812500005, -4.985214923628404016, -6.290624999385458160 ) ) ;
#12007 = CARTESIAN_POINT ( 'NONE',  ( 22.56230152254394383, 3.464101615137847645, -6.374999998770999099 ) ) ;
#12008 = CARTESIAN_POINT ( 'NONE',  ( 23.87821517812500005, 246.7468750006145228, 4.985214923628404016 ) ) ;
#12009 = CARTESIAN_POINT ( 'NONE',  ( -6.932735513423968321, 41.74768628210144783, -10.69584247140445221 ) ) ;
#12010 = EDGE_CURVE ( 'NONE', #18510, #34425, #34225, .T. ) ;
#12011 = CARTESIAN_POINT ( 'NONE',  ( -53.36086230271183695, 213.1499508600178387, -5.686928522499747451 ) ) ;
#12012 = VECTOR ( 'NONE', #32730, 1000.000000000000000 ) ;
#12013 = CARTESIAN_POINT ( 'NONE',  ( -67.41294563604516554, 214.6737587650350747, -4.842901733360249317 ) ) ;
#12014 =( NAMED_UNIT ( * ) SI_UNIT ( $, .STERADIAN. ) SOLID_ANGLE_UNIT ( ) );
#12015 = CARTESIAN_POINT ( 'NONE',  ( 24.74614436184151955, 0.000000000000000000, 161.6609054635707423 ) ) ;
#12016 = CARTESIAN_POINT ( 'NONE',  ( 7.228626920338837358, 104.5273137178985650, 10.49813415416005036 ) ) ;
#12017 = EDGE_CURVE ( 'NONE', #31527, #33538, #15993, .T. ) ;
#12018 = CARTESIAN_POINT ( 'NONE',  ( -57.52455436395489841, 206.6211998817774997, 3.209657149897401585 ) ) ;
#12020 = ADVANCED_FACE ( 'NONE', ( #8268, #28346 ), #36871, .F. ) ;
#12019 = CARTESIAN_POINT ( 'NONE',  ( -67.02455436395489130, 205.1570982666397356, 4.673758765035198159 ) ) ;
#12021 = CARTESIAN_POINT ( 'NONE',  ( 15.24356964374999990, 0.000000000000000000, -7.003124999385490490 ) ) ;
#12022 = CARTESIAN_POINT ( 'NONE',  ( -27.24356964374999635, 194.8906250006145342, 15.72908226750539384 ) ) ;
#12023 = CARTESIAN_POINT ( 'NONE',  ( -15.50000000000000533, 80.08981371789856496, 0.1745138560722471477 ) ) ;
#12024 = CARTESIAN_POINT ( 'NONE',  ( -63.05877896937850835, 212.1620413398627534, -8.530955311639255356 ) ) ;
#12025 = ORIENTED_EDGE ( 'NONE', *, *, #22570, .T. ) ;
#12026 = CARTESIAN_POINT ( 'NONE',  ( 37.15151170766156952, 7.347880794884117764E-16, 165.7703441132237003 ) ) ;
#12027 = CARTESIAN_POINT ( 'NONE',  ( -10.49813415415989581, 96.37268628210145494, -7.228626920339068285 ) ) ;
#12028 = CARTESIAN_POINT ( 'NONE',  ( -8.632099005475501130, 41.74768628210143362, -13.23911966647218996 ) ) ;
#12029 = CARTESIAN_POINT ( 'NONE',  ( 19.97220920615905371, 239.6536485351579699, -5.828890057712500017 ) ) ;
#12030 = CARTESIAN_POINT ( 'NONE',  ( 30.62771359501211066, -7.209453229046482114, 160.0452699470032485 ) ) ;
#12031 = CARTESIAN_POINT ( 'NONE',  ( -0.1745138560725817967, 65.61018628210146630, 15.50000000000000533 ) ) ;
#12032 = DIRECTION ( 'NONE',  ( 1.000000000000000000, 0.000000000000000000, 0.000000000000000000 ) ) ;
#12033 = CARTESIAN_POINT ( 'NONE',  ( 19.68408634441910721, -5.407089921784855591, -8.090624999385564564 ) ) ;
#12034 = DIRECTION ( 'NONE',  ( -0.5887012860850800999, 0.8083506638593009885, -0.000000000000000000 ) ) ;
#12035 = CARTESIAN_POINT ( 'NONE',  ( -53.56622103062157692, 211.6261429550005744, 6.530955311639227823 ) ) ;
#12036 = CARTESIAN_POINT ( 'NONE',  ( 11.02886091400724133, -2.913158743114809823, -10.00000000000000178 ) ) ;
#12037 = CARTESIAN_POINT ( 'NONE',  ( 12.50000000000000355, 35.71018628210144641, 0.1745138560725507937 ) ) ;
#12038 = CARTESIAN_POINT ( 'NONE',  ( 26.99999999999999645, 7.347880794884117764E-16, -7.818749998770941012 ) ) ;
#12039 = CARTESIAN_POINT ( 'NONE',  ( 5.529263428287477744, 15.87268628210144605, -7.954856959092191815 ) ) ;
#12040 = CARTESIAN_POINT ( 'NONE',  ( 23.87821517812500005, 245.5093750006145399, 4.985214923628404016 ) ) ;
#12041 = ORIENTED_EDGE ( 'NONE', *, *, #34859, .T. ) ;
#12042 = CARTESIAN_POINT ( 'NONE',  ( 26.99999999999999645, 7.347880794884117764E-16, -6.975000000000008527 ) ) ;
#12043 = CARTESIAN_POINT ( 'NONE',  ( 0.000000000000000000, 200.0000000000000000, -27.00000000000000355 ) ) ;
#12044 = CARTESIAN_POINT ( 'NONE',  ( 10.56230152254411081, 0.000000000000000000, -7.537499998771012955 ) ) ;
#12045 = CARTESIAN_POINT ( 'NONE',  ( 16.56230152254411436, 7.209453229046475009, -4.753124999385526017 ) ) ;
#12046 = CARTESIAN_POINT ( 'NONE',  ( 34.41253136604939300, -5.407089921784855591, 167.4874711655023418 ) ) ;
#12047 = CARTESIAN_POINT ( 'NONE',  ( 21.00000000000000000, 241.7874999999999943, -6.928203230275506996 ) ) ;
#12048 = CARTESIAN_POINT ( 'NONE',  ( -27.00000000000000355, 199.5124999999999886, -15.58845726811989429 ) ) ;
#12049 = CARTESIAN_POINT ( 'NONE',  ( -6.932735513423968321, 41.74768628210144783, -10.69584247140445221 ) ) ;
#12050 = ORIENTED_EDGE ( 'NONE', *, *, #5172, .T. ) ;
#12051 = VERTEX_POINT ( 'NONE', #25137 ) ;
#12052 = LINE ( 'NONE', #14349, #3058 ) ;
#12053 = CARTESIAN_POINT ( 'NONE',  ( 26.99999999999946354, -3.464101615138058143, -3.356249998770978848 ) ) ;
#12054 = CARTESIAN_POINT ( 'NONE',  ( 18.00000000000000355, 248.2750000000000057, 5.196152422706632912 ) ) ;
#12055 = CARTESIAN_POINT ( 'NONE',  ( 26.75643035624999655, 7.049594010296217766E-16, -5.765624999385460470 ) ) ;
#12056 = CARTESIAN_POINT ( 'NONE',  ( -10.49813415415989581, 96.37268628210145494, -7.228626920339068285 ) ) ;
#12057 = CARTESIAN_POINT ( 'NONE',  ( 14.38691631536194393, 20.86481371789854578, 5.770363421894124656 ) ) ;
#12058 = CARTESIAN_POINT ( 'NONE',  ( 18.00000000000000355, -5.196152422706632912, -5.268749998770943854 ) ) ;
#12059 = CARTESIAN_POINT ( 'NONE',  ( 18.12178482187500350, 240.9343750006145513, 4.985214923628407568 ) ) ;
#12060 = CARTESIAN_POINT ( 'NONE',  ( -36.54538769728824121, 211.3212981617418222, -4.469044688360751749 ) ) ;
#12061 = CYLINDRICAL_SURFACE ( 'NONE', #21000, 6.000000000000001776 ) ;
#12062 = CARTESIAN_POINT ( 'NONE',  ( 25.41288579386105440, 0.000000000000000000, 169.2817949039725818 ) ) ;
#12063 = CARTESIAN_POINT ( 'NONE',  ( -6.594114490232462877, 14.53981371789855892, 6.840914352311949109 ) ) ;
#12064 = CARTESIAN_POINT ( 'NONE',  ( -63.46205436395489841, 214.6737587650352168, 4.842901733360204908 ) ) ;
#12065 = CARTESIAN_POINT ( 'NONE',  ( -31.19419563604517265, 201.5000000000000000, 0.1155267958018195706 ) ) ;
#12066 = DIRECTION ( 'NONE',  ( 0.000000000000000000, 0.000000000000000000, 1.000000000000000000 ) ) ;
#12067 = CARTESIAN_POINT ( 'NONE',  ( 17.54540804174073187, 195.0000000000000000, -20.52215039046394907 ) ) ;
#12068 = CARTESIAN_POINT ( 'NONE',  ( -27.24356964374999635, 196.7468750006145797, 15.72908226750539384 ) ) ;
#12069 = CARTESIAN_POINT ( 'NONE',  ( -13.04141134922778456, 125.2273137178985394, 8.927990412390377273 ) ) ;
#12070 = CARTESIAN_POINT ( 'NONE',  ( -52.17336230271183695, 215.6869285224997270, 3.149950860017831200 ) ) ;
#12071 = VERTEX_POINT ( 'NONE', #33856 ) ;
#12072 = CARTESIAN_POINT ( 'NONE',  ( 12.53471296425194836, 44.62268628210144783, -2.311890736173178418 ) ) ;
#12073 = CARTESIAN_POINT ( 'NONE',  ( 20.99999999999999289, 244.5437500012290570, -5.999999999999997335 ) ) ;
#12074 = CARTESIAN_POINT ( 'NONE',  ( 24.69183098274843502, 4.432317000257220307, -7.999999999999998224 ) ) ;
#12075 = CARTESIAN_POINT ( 'NONE',  ( 25.06810737005524459, -3.604726614523244610, 168.1356077347459461 ) ) ;
#12076 = CARTESIAN_POINT ( 'NONE',  ( 21.00000000000000000, -6.928203230275506996, -2.081249998770946963 ) ) ;
#12077 = DIRECTION ( 'NONE',  ( -0.000000000000000000, -0.000000000000000000, 1.000000000000000000 ) ) ;
#12078 = CARTESIAN_POINT ( 'NONE',  ( 10.31873187879411091, 0.000000000000000000, -1.940624999385548444 ) ) ;
#12079 = CARTESIAN_POINT ( 'NONE',  ( 8.710071997420127943, 63.88518628210145778, 3.796722387233375073 ) ) ;
#12080 = CARTESIAN_POINT ( 'NONE',  ( 21.00000000000000355, 0.000000000000000000, 50.00000000000001421 ) ) ;
#12081 = CARTESIAN_POINT ( 'NONE',  ( -89.59418277001438469, 62.43429747954478159, 3.000000000000000000 ) ) ;
#12082 = CARTESIAN_POINT ( 'NONE',  ( -10.69584247140444866, 103.8476862821014493, 6.932735513423972762 ) ) ;
#12083 = CARTESIAN_POINT ( 'NONE',  ( 10.56230152254410903, 0.000000000000000000, -4.950000000000037481 ) ) ;
#12084 = CARTESIAN_POINT ( 'NONE',  ( 20.99999999999998579, 247.6937500012290059, -5.999999999999997335 ) ) ;
#12085 = ORIENTED_EDGE ( 'NONE', *, *, #6247, .F. ) ;
#12086 = CARTESIAN_POINT ( 'NONE',  ( -77.00000000000002842, 210.0000000000000000, 3.000000000000000000 ) ) ;
#12087 = CARTESIAN_POINT ( 'NONE',  ( 26.99999999999999645, -3.464101615137751278, -0.2625000000000108913 ) ) ;
#12088 = CARTESIAN_POINT ( 'NONE',  ( -26.99999999999999645, 198.3500000012290343, 15.58845726811991561 ) ) ;
#12089 = CARTESIAN_POINT ( 'NONE',  ( 27.90674060888834518, -5.407089921784865361, 164.7628702620865226 ) ) ;
#12090 = CARTESIAN_POINT ( 'NONE',  ( 36.86716609684025059, 7.347880794884125653E-16, 162.5202589094750181 ) ) ;
#12091 = CARTESIAN_POINT ( 'NONE',  ( 27.00000000000000355, 196.6250000000000284, -3.306546357697854128E-15 ) ) ;
#12092 = CARTESIAN_POINT ( 'NONE',  ( 18.00000000000000000, 247.6750000000000114, -5.196152422706630247 ) ) ;
#12093 = CARTESIAN_POINT ( 'NONE',  ( 27.24356964374999279, 196.9156250006145399, -15.72908226750539207 ) ) ;
#12094 = CARTESIAN_POINT ( 'NONE',  ( -11.48171059495408208, 97.91481371789856780, 4.944772684328421875 ) ) ;
#12095 = CARTESIAN_POINT ( 'NONE',  ( -12.50000000000000355, 132.3101862821014549, -0.1745138560725492671 ) ) ;
#12097 = ORIENTED_EDGE ( 'NONE', *, *, #35164, .F. ) ;
#12096 = ORIENTED_EDGE ( 'NONE', *, *, #8355, .F. ) ;
#12098 = CARTESIAN_POINT ( 'NONE',  ( 27.24356964375000345, 195.5281250006145228, -3.336375036156643733E-15 ) ) ;
#12099 = CARTESIAN_POINT ( 'NONE',  ( 23.87821517812500005, 239.9968750006144944, 4.985214923628404016 ) ) ;
#12100 = CARTESIAN_POINT ( 'NONE',  ( -14.25334919248795096, 79.51481371789856212, 6.092822981423662299 ) ) ;
#12101 = CARTESIAN_POINT ( 'NONE',  ( 23.87821517812499650, 4.985214923628404904, -4.003124999385487826 ) ) ;
#12102 = CARTESIAN_POINT ( 'NONE',  ( 26.75643035624999655, 248.3218750006145399, -3.323476615752271712 ) ) ;
#12103 = AXIS2_PLACEMENT_3D ( 'NONE', #36595, #1915, #19002 ) ;
#12104 = CARTESIAN_POINT ( 'NONE',  ( 2.064181346179272847, 98.09768628210146346, -9.465287035748065847 ) ) ;
#12105 = CARTESIAN_POINT ( 'NONE',  ( 27.00000000000001066, 196.7000000012290286, 15.58845726811988897 ) ) ;
#12106 = CARTESIAN_POINT ( 'NONE',  ( -7.954856959092309943, 79.22731371789853938, 5.529263428287300108 ) ) ;
#12107 = CARTESIAN_POINT ( 'NONE',  ( 22.80587116629410716, 7.646167579472015790E-16, -5.315624999385537564 ) ) ;
#12108 = CARTESIAN_POINT ( 'NONE',  ( 26.75643035624999655, 240.9718750006145171, -7.049594010296217766E-16 ) ) ;
#12109 = CARTESIAN_POINT ( 'NONE',  ( 8.962234695871567070, 39.83981371789855075, 8.715434833792127023 ) ) ;
#12110 = PLANE ( 'NONE',  #1878 ) ;
#12111 = AXIS2_PLACEMENT_3D ( 'NONE', #5142, #4400, #16723 ) ;
#12112 = CARTESIAN_POINT ( 'NONE',  ( 12.46528703574805874, 109.5976862821014493, 2.660918448318279950 ) ) ;
#12113 = CARTESIAN_POINT ( 'NONE',  ( 10.56230152254411614, -3.464101615137757051, -5.699999998771023257 ) ) ;
#12114 = CARTESIAN_POINT ( 'NONE',  ( -33.37872103062156981, 203.4690446883607535, 1.626142955000567936 ) ) ;
#12115 = CARTESIAN_POINT ( 'NONE',  ( 26.99999999999999645, 7.347880794884117764E-16, -7.368749998770962151 ) ) ;
#12116 = CARTESIAN_POINT ( 'NONE',  ( 24.75598086634022010, 0.000000000000000000, 164.5679854722048958 ) ) ;
#12117 = CARTESIAN_POINT ( 'NONE',  ( -0.1745138560725817967, 74.81018628210145494, 15.50000000000000533 ) ) ;
#12118 = CARTESIAN_POINT ( 'NONE',  ( 13.44051670066910908, 5.407089921784862696, -4.771874999385556038 ) ) ;
#12119 = LINE ( 'NONE', #23886, #15170 ) ;
#12120 = CARTESIAN_POINT ( 'NONE',  ( 15.12178482187499995, 249.9296875003072387, 0.000000000000000000 ) ) ;
#12121 = LINE ( 'NONE', #26712, #32691 ) ;
#12122 = CARTESIAN_POINT ( 'NONE',  ( -0.1745138560725182642, 120.8101862821014691, 9.500000000000005329 ) ) ;
#12123 = CARTESIAN_POINT ( 'NONE',  ( 27.00000000000001421, 194.9000000012290457, 15.58845726811988897 ) ) ;
#12124 = CARTESIAN_POINT ( 'NONE',  ( -0.1745138560725817967, 10.41018628210144037, 15.50000000000000533 ) ) ;
#12125 = CARTESIAN_POINT ( 'NONE',  ( -13.62178482187500528, 195.7343750006145626, -23.59362340125807123 ) ) ;
#12126 = CARTESIAN_POINT ( 'NONE',  ( 18.12178482187500350, 242.6218750006145228, 4.985214923628407568 ) ) ;
#12127 = EDGE_LOOP ( 'NONE', ( #9129, #11361, #22790, #2673 ) ) ;
#12128 = CARTESIAN_POINT ( 'NONE',  ( 37.48648511030115316, -3.604726614523235284, 166.8044593776906481 ) ) ;
#12129 = CARTESIAN_POINT ( 'NONE',  ( 18.12178482187499640, 4.985214923628404904, -3.365624999385474769 ) ) ;
#12130 = CARTESIAN_POINT ( 'NONE',  ( 10.56230152254410903, 0.000000000000000000, -4.950000000000037481 ) ) ;
#12131 = CARTESIAN_POINT ( 'NONE',  ( 2.999999999999997780, 244.5000000000000000, 2.500000000000000000 ) ) ;
#12132 = CARTESIAN_POINT ( 'NONE',  ( 10.56230152254410903, 0.000000000000000000, -5.737499998771017573 ) ) ;
#12133 = LINE ( 'NONE', #6828, #16241 ) ;
#12134 = ADVANCED_FACE ( 'NONE', ( #37059 ), #25322, .T. ) ;
#12135 = CARTESIAN_POINT ( 'NONE',  ( 22.80587116629410716, 7.646167579472015790E-16, -0.8156249993855335667 ) ) ;
#12136 = CARTESIAN_POINT ( 'NONE',  ( 5.233372021372610483, 18.85231371789855359, -8.152565276336593669 ) ) ;
#12137 = CARTESIAN_POINT ( 'NONE',  ( -13.62178482187500528, 198.8843750006145399, -23.59362340125807123 ) ) ;
#12138 = ORIENTED_EDGE ( 'NONE', *, *, #9024, .T. ) ;
#12139 = CARTESIAN_POINT ( 'NONE',  ( 21.00000000000000000, 249.1843750006144944, -6.646953231504538984 ) ) ;
#12140 = CARTESIAN_POINT ( 'NONE',  ( -8.962234695871565293, 44.43981371789855217, -8.715434833792128799 ) ) ;
#12141 = CARTESIAN_POINT ( 'NONE',  ( 15.24356964375000167, -3.323476615752272600, -0.5531249993854806535 ) ) ;
#12142 = CARTESIAN_POINT ( 'NONE',  ( -10.69584247140429412, 7.352313717898545598, -6.932735513424201024 ) ) ;
#12143 =( BOUNDED_CURVE ( )  B_SPLINE_CURVE ( 2, ( #1792, #4633, #7304, #33445, #10507, #7488, #1414, #13359, #16212, #4447, #27761, #1040, #24729, #16027, #18876, #21532, #35722, #24914, #27576, #33079, #12796, #21346, #1605, #10327, #12992, #30427, #22087, #13173, #21897, #9768, #33637, #15461, #18312, #29852, #3889, #1224, #27015, #21714, #12611, #30044, #4261, #24177, #32885, #6934, #4078, #15650, #27198, #36097, #24365, #35909, #9952, #7122, #18694, #30235, #15836, #27384, #24547, #10141, #34191, #36841, #10696, #16399, #8049, #10884, #5374, #22273, #7676, #33826, #16768, #8238, #25658, #19813, #11258, #28496, #7863, #5004, #5193, #30987, #17142, #25100, #22646, #4818, #31347, #34004, #2352, #22457, #16586, #16953, #2539, #14106, #25844, #37212, #19437, #13924, #22830, #28131, #27944, #37393, #2160, #1975, #37025, #13743, #36658, #34378, #8419, #13547, #25289, #31171, #19624, #19988, #28314, #31532, #5557, #25474, #11071, #28678, #2716, #14292, #11443, #23010, #19256, #30795, #31904, #6505, #17888, #23569, #26210, #56, #8599, #246, #18080, #615, #8974, #17325, #26776, #26400, #14475, #29621, #3656, #3091, #14659, #34746, #5933, #32088, #20361, #15227, #26028, #11998, #35114, #35296, #3469, #28868, #20545, #17512, #29047, #8789, #5745, #11810, #20170, #32273, #23380, #9162, #23198, #31718, #807, #34929, #2902, #433, #11623, #12378, #34560, #6120, #17698, #29238, #3278, #14851, #20730, #6316, #29433, #15038, #26586, #12184, #23757, #9352, #20923, #32462, #30192, #12947, #35867, #6694, #32840, #6885, #15987, #24686, #36056, #30383, #4594, #36240, #13132, #23948, #24508, #21114, #18460, #29809, #30003, #1560, #32653, #19021, #21304, #10282, #7083, #18651, #27535, #26966, #10099, #4404, #4218, #21669, #21856, #33223, #33409, #15796, #7262, #18837, #4032, #7447, #35680, #30578, #27346, #21493, #1377, #18265, #9732, #9909, #995, #16171, #15604, #27721, #1750, #3842, #12571, #27160, #1183, #35490, #15420, #9540, #12757, #24138, #24325, #33033, #34148, #2310, #4960, #16353, #24875, #16542, #22785, #16914, #25248, #33596, #5514, #22416, #13884, #31308, #25433, #28455, #8195, #13501, #10653, #10842, #36612, #34334, #30758, #28274, #36985, #14066, #19771, #7635, #36798, #22232, #7821, #11028, #22603, #31491, #5336, #25059, #8005, #2491, #1933, #10467, #17099, #33783, #22045, #5147, #19212, #28638, #8379, #19398, #33963, #28088, #30941, #25615, #2120, #37172, #4780, #11213, #19950, #13697, #19578, #31130, #27902, #16728, #13317, #36424, #14619, #22972, #11583, #23158, #32234, #3425, #14810, #17850, #32421, #29388, #23339, #23715, #26544, #26355, #14993, #34520, #9122, #391, #3237, #5893, #20127, #573, #11957, #17471, #34700, #2676, #35073, #20688, #34890, #23527, #12140, #6273, #35256, #31674, #9311, #37349, #20882, #6465, #8930, #6075, #2859, #5703, #17283, #18036, #14251, #8560, #28824, #20507, #25987, #11773, #14433, #32044, #29006, #25800, #11401, #17, #8747, #20318, #31859, #3050, #26171, #17660, #207, #29195, #21816, #13091, #30339, #36015, #10240, #4363, #18798, #29580, #18608, #15943, #26731, #24092, #35449, #954, #7225, #765, #24646, #26924, #27495, #12711, #24282, #21630, #32612, #4180, #18226, #12333, #15752, #1517, #15562, #27302, #9867, #12904, #1334, #12529, #24468, #35827, #32988, #10054, #27119, #33181, #36196, #21448, #3618, #35637, #33368, #7405, #23907, #29766, #3797, #30152, #9684, #15184, #15375, #9497, #21073, #1142, #6650, #21261, #32800, #6836, #18414, #7041, #29960, #3988, #22559, #30899, #1705, #11175, #10803, #36383, #28412, #25575, #25016, #36571, #22376, #22749, #33924, #31270, #19540, #8158, #28237, #19358, #16129, #25392, #13277, #4920, #4738, #13464, #30718, #27679, #19170, #4554, #16690, #7780, #5111, #10613, #31087, #19732, #16501 ),
 .UNSPECIFIED., .F., .F. ) 
 B_SPLINE_CURVE_WITH_KNOTS ( ( 3, 2, 2, 2, 2, 2, 2, 2, 2, 2, 2, 2, 2, 2, 2, 2, 2, 2, 2, 2, 2, 2, 2, 2, 2, 2, 2, 2, 2, 2, 2, 2, 2, 2, 2, 2, 2, 2, 2, 2, 2, 2, 2, 2, 2, 2, 2, 2, 2, 2, 2, 2, 2, 2, 2, 2, 2, 2, 2, 2, 2, 2, 2, 2, 2, 2, 2, 2, 2, 2, 2, 2, 2, 2, 2, 2, 2, 2, 2, 2, 2, 2, 2, 2, 2, 2, 2, 2, 2, 2, 2, 2, 2, 2, 2, 2, 2, 2, 2, 2, 2, 2, 2, 2, 2, 2, 2, 2, 2, 2, 2, 2, 2, 2, 2, 2, 2, 2, 2, 2, 2, 2, 2, 2, 2, 2, 2, 2, 2, 2, 2, 2, 2, 2, 2, 2, 2, 2, 2, 2, 2, 2, 2, 2, 2, 2, 2, 2, 2, 2, 2, 2, 2, 2, 2, 2, 2, 2, 2, 2, 2, 2, 2, 2, 2, 2, 2, 2, 2, 2, 2, 2, 2, 2, 2, 2, 2, 2, 2, 2, 2, 2, 2, 2, 2, 2, 2, 2, 2, 2, 2, 2, 2, 2, 2, 2, 2, 2, 2, 2, 2, 2, 2, 2, 2, 2, 2, 2, 2, 2, 2, 2, 2, 2, 2, 2, 2, 2, 2, 2, 2, 2, 2, 2, 2, 2, 2, 2, 2, 2, 2, 2, 2, 2, 2, 2, 2, 2, 3 ),
 ( 0.01079222792828509608, 0.01250000000000000069, 0.01666666666666666644, 0.02083333333333333218, 0.02500000000000000139, 0.02916666666666666713, 0.03333333333333333287, 0.03749999999999999861, 0.04166666666666666435, 0.04583333333333333010, 0.05000000000000000278, 0.05416666666666666852, 0.05833333333333333426, 0.06250000000000000000, 0.06666666666666666574, 0.07083333333333333148, 0.07500000000000001110, 0.07916666666666666297, 0.08333333333333334259, 0.08749999999999999445, 0.09166666666666667407, 0.09583333333333335369, 0.1000000000000000056, 0.1041666666666666852, 0.1083333333333333370, 0.1125000000000000167, 0.1166666666666666685, 0.1208333333333333481, 0.1250000000000000000, 0.1291666666666666796, 0.1333333333333333315, 0.1375000000000000111, 0.1416666666666666630, 0.1458333333333333426, 0.1499999999999999944, 0.1541666666666666741, 0.1583333333333333259, 0.1625000000000000056, 0.1666666666666666574, 0.1708333333333333370, 0.1749999999999999889, 0.1791666666666666685, 0.1833333333333333204, 0.1875000000000000000, 0.1916666666666666796, 0.1958333333333333315, 0.2000000000000000111, 0.2041666666666666630, 0.2083333333333333426, 0.2124999999999999944, 0.2166666666666666741, 0.2208333333333333259, 0.2250000000000000056, 0.2291666666666666574, 0.2333333333333333370, 0.2374999999999999889, 0.2416666666666666685, 0.2458333333333333204, 0.2500000000000000000, 0.2541666666666666519, 0.2583333333333333592, 0.2625000000000000111, 0.2666666666666666630, 0.2708333333333333148, 0.2750000000000000222, 0.2791666666666666741, 0.2833333333333333259, 0.2874999999999999778, 0.2916666666666666852, 0.2958333333333333370, 0.2999999999999999889, 0.3041666666666666408, 0.3083333333333333481, 0.3125000000000000000, 0.3166666666666666519, 0.3208333333333333592, 0.3250000000000000111, 0.3291666666666666630, 0.3333333333333333148, 0.3375000000000000222, 0.3416666666666666741, 0.3458333333333333259, 0.3499999999999999778, 0.3541666666666666852, 0.3583333333333333370, 0.3624999999999999889, 0.3666666666666666408, 0.3708333333333333481, 0.3750000000000000000, 0.3791666666666666519, 0.3833333333333333592, 0.3875000000000000111, 0.3916666666666666630, 0.3958333333333333148, 0.4000000000000000222, 0.4041666666666666741, 0.4083333333333333259, 0.4124999999999999778, 0.4166666666666666852, 0.4208333333333333370, 0.4249999999999999889, 0.4291666666666666408, 0.4333333333333333481, 0.4375000000000000000, 0.4416666666666666519, 0.4458333333333333592, 0.4500000000000000111, 0.4541666666666666630, 0.4583333333333333148, 0.4625000000000000222, 0.4666666666666666741, 0.4708333333333333259, 0.4749999999999999778, 0.4791666666666666852, 0.4833333333333333370, 0.4874999999999999889, 0.4916666666666666408, 0.4958333333333333481, 0.5000000000000000000, 0.5041666666666666519, 0.5083333333333333037, 0.5124999999999999556, 0.5166666666666667185, 0.5208333333333333703, 0.5250000000000000222, 0.5291666666666666741, 0.5333333333333333259, 0.5374999999999999778, 0.5416666666666666297, 0.5458333333333332815, 0.5500000000000000444, 0.5541666666666666963, 0.5583333333333333481, 0.5625000000000000000, 0.5666666666666666519, 0.5708333333333333037, 0.5749999999999999556, 0.5791666666666667185, 0.5833333333333333703, 0.5875000000000000222, 0.5916666666666666741, 0.5958333333333332149, 0.5999999999999999778, 0.6041666666666666297, 0.6083333333333332815, 0.6125000000000000444, 0.6166666666666666963, 0.6208333333333333481, 0.6250000000000000000, 0.6291666666666666519, 0.6333333333333333037, 0.6374999999999999556, 0.6416666666666667185, 0.6458333333333333703, 0.6500000000000000222, 0.6541666666666666741, 0.6583333333333333259, 0.6624999999999999778, 0.6666666666666666297, 0.6708333333333332815, 0.6750000000000000444, 0.6791666666666666963, 0.6833333333333333481, 0.6875000000000000000, 0.6916666666666666519, 0.6958333333333333037, 0.6999999999999999556, 0.7041666666666667185, 0.7083333333333333703, 0.7125000000000000222, 0.7166666666666666741, 0.7208333333333333259, 0.7249999999999999778, 0.7291666666666666297, 0.7333333333333332815, 0.7375000000000000444, 0.7416666666666666963, 0.7458333333333333481, 0.7500000000000000000, 0.7541666666666666519, 0.7583333333333333037, 0.7624999999999999556, 0.7666666666666667185, 0.7708333333333333703, 0.7750000000000000222, 0.7791666666666666741, 0.7833333333333333259, 0.7874999999999999778, 0.7916666666666666297, 0.7958333333333332815, 0.8000000000000000444, 0.8041666666666666963, 0.8083333333333333481, 0.8125000000000000000, 0.8166666666666666519, 0.8208333333333333037, 0.8249999999999999556, 0.8291666666666667185, 0.8333333333333333703, 0.8375000000000000222, 0.8416666666666666741, 0.8458333333333332149, 0.8499999999999999778, 0.8541666666666666297, 0.8583333333333332815, 0.8625000000000000444, 0.8666666666666666963, 0.8708333333333333481, 0.8750000000000000000, 0.8791666666666666519, 0.8833333333333333037, 0.8874999999999999556, 0.8916666666666667185, 0.8958333333333333703, 0.9000000000000000222, 0.9041666666666666741, 0.9083333333333333259, 0.9124999999999999778, 0.9166666666666666297, 0.9208333333333332815, 0.9250000000000000444, 0.9291666666666666963, 0.9333333333333333481, 0.9375000000000000000, 0.9416666666666666519, 0.9458333333333333037, 0.9499999999999999556, 0.9541666666666667185, 0.9583333333333333703, 0.9625000000000000222, 0.9666666666666666741, 0.9708333333333333259, 0.9749999999999999778, 0.9791666666666666297, 0.9833333333333332815, 0.9875000000000000444, 0.9916666666666666963, 0.9958333333333333481, 1.000000000000000000 ),
 .UNSPECIFIED. ) 
 CURVE ( )  GEOMETRIC_REPRESENTATION_ITEM ( )  RATIONAL_B_SPLINE_CURVE ( ( 0.9907048511358500509, 0.9921245532416329560, 1.000000000000000000, 0.9807852804032304306, 1.000000000000000000, 0.9807852804032304306, 1.000000000000000000, 0.9807852804032304306, 1.000000000000000000, 0.9807852804032304306, 1.000000000000000000, 0.9807852804032304306, 1.000000000000000000, 0.9807852804032304306, 1.000000000000000000, 0.9807852804032304306, 1.000000000000000000, 0.9807852804032304306, 1.000000000000000000, 0.9807852804032304306, 1.000000000000000000, 0.9807852804032304306, 1.000000000000000000, 0.9807852804032304306, 1.000000000000000000, 0.9807852804032304306, 1.000000000000000000, 0.9807852804032304306, 1.000000000000000000, 0.9807852804032304306, 1.000000000000000000, 0.9807852804032304306, 1.000000000000000000, 0.9807852804032304306, 1.000000000000000000, 0.9807852804032304306, 1.000000000000000000, 0.9807852804032304306, 1.000000000000000000, 0.9807852804032304306, 1.000000000000000000, 0.9807852804032304306, 1.000000000000000000, 0.9807852804032304306, 1.000000000000000000, 0.9807852804032304306, 1.000000000000000000, 0.9807852804032304306, 1.000000000000000000, 0.9807852804032304306, 1.000000000000000000, 0.9807852804032304306, 1.000000000000000000, 0.9807852804032304306, 1.000000000000000000, 0.9807852804032304306, 1.000000000000000000, 0.9807852804032304306, 1.000000000000000000, 0.9807852804032304306, 1.000000000000000000, 0.9807852804032304306, 1.000000000000000000, 0.9807852804032304306, 1.000000000000000000, 0.9807852804032304306, 1.000000000000000000, 0.9807852804032304306, 1.000000000000000000, 0.9807852804032304306, 1.000000000000000000, 0.9807852804032304306, 1.000000000000000000, 0.9807852804032304306, 1.000000000000000000, 0.9807852804032304306, 1.000000000000000000, 0.9807852804032304306, 1.000000000000000000, 0.9807852804032304306, 1.000000000000000000, 0.9807852804032304306, 1.000000000000000000, 0.9807852804032304306, 1.000000000000000000, 0.9807852804032304306, 1.000000000000000000, 0.9807852804032304306, 1.000000000000000000, 0.9807852804032304306, 1.000000000000000000, 0.9807852804032304306, 1.000000000000000000, 0.9807852804032304306, 1.000000000000000000, 0.9807852804032304306, 1.000000000000000000, 0.9807852804032304306, 1.000000000000000000, 0.9807852804032304306, 1.000000000000000000, 0.9807852804032304306, 1.000000000000000000, 0.9807852804032304306, 1.000000000000000000, 0.9807852804032304306, 1.000000000000000000, 0.9807852804032304306, 1.000000000000000000, 0.9807852804032304306, 1.000000000000000000, 0.9807852804032304306, 1.000000000000000000, 0.9807852804032304306, 1.000000000000000000, 0.9807852804032304306, 1.000000000000000000, 0.9807852804032304306, 1.000000000000000000, 0.9807852804032304306, 1.000000000000000000, 0.9807852804032304306, 1.000000000000000000, 0.9807852804032304306, 1.000000000000000000, 0.9807852804032304306, 1.000000000000000000, 0.9807852804032304306, 1.000000000000000000, 0.9807852804032304306, 1.000000000000000000, 0.9807852804032304306, 1.000000000000000000, 0.9807852804032304306, 1.000000000000000000, 0.9807852804032304306, 1.000000000000000000, 0.9807852804032304306, 1.000000000000000000, 0.9807852804032304306, 1.000000000000000000, 0.9807852804032304306, 1.000000000000000000, 0.9807852804032304306, 1.000000000000000000, 0.9807852804032304306, 1.000000000000000000, 0.9807852804032304306, 1.000000000000000000, 0.9807852804032304306, 1.000000000000000000, 0.9807852804032304306, 1.000000000000000000, 0.9807852804032304306, 1.000000000000000000, 0.9807852804032304306, 1.000000000000000000, 0.9807852804032304306, 1.000000000000000000, 0.9807852804032304306, 1.000000000000000000, 0.9807852804032304306, 1.000000000000000000, 0.9807852804032304306, 1.000000000000000000, 0.9807852804032304306, 1.000000000000000000, 0.9807852804032304306, 1.000000000000000000, 0.9807852804032304306, 1.000000000000000000, 0.9807852804032304306, 1.000000000000000000, 0.9807852804032304306, 1.000000000000000000, 0.9807852804032304306, 1.000000000000000000, 0.9807852804032304306, 1.000000000000000000, 0.9807852804032304306, 1.000000000000000000, 0.9807852804032304306, 1.000000000000000000, 0.9807852804032304306, 1.000000000000000000, 0.9807852804032304306, 1.000000000000000000, 0.9807852804032304306, 1.000000000000000000, 0.9807852804032304306, 1.000000000000000000, 0.9807852804032304306, 1.000000000000000000, 0.9807852804032304306, 1.000000000000000000, 0.9807852804032304306, 1.000000000000000000, 0.9807852804032304306, 1.000000000000000000, 0.9807852804032304306, 1.000000000000000000, 0.9807852804032304306, 1.000000000000000000, 0.9807852804032304306, 1.000000000000000000, 0.9807852804032304306, 1.000000000000000000, 0.9807852804032304306, 1.000000000000000000, 0.9807852804032304306, 1.000000000000000000, 0.9807852804032304306, 1.000000000000000000, 0.9807852804032304306, 1.000000000000000000, 0.9807852804032304306, 1.000000000000000000, 0.9807852804032304306, 1.000000000000000000, 0.9807852804032304306, 1.000000000000000000, 0.9807852804032304306, 1.000000000000000000, 0.9807852804032304306, 1.000000000000000000, 0.9807852804032304306, 1.000000000000000000, 0.9807852804032304306, 1.000000000000000000, 0.9807852804032304306, 1.000000000000000000, 0.9807852804032304306, 1.000000000000000000, 0.9807852804032304306, 1.000000000000000000, 0.9807852804032304306, 1.000000000000000000, 0.9807852804032304306, 1.000000000000000000, 0.9807852804032304306, 1.000000000000000000, 0.9807852804032304306, 1.000000000000000000, 0.9807852804032304306, 1.000000000000000000, 0.9807852804032304306, 1.000000000000000000, 0.9807852804032304306, 1.000000000000000000, 0.9807852804032304306, 1.000000000000000000, 0.9807852804032304306, 1.000000000000000000, 0.9807852804032304306, 1.000000000000000000, 0.9807852804032304306, 1.000000000000000000, 0.9807852804032304306, 1.000000000000000000, 0.9807852804032304306, 1.000000000000000000, 0.9807852804032304306, 1.000000000000000000, 0.9807852804032304306, 1.000000000000000000, 0.9807852804032304306, 1.000000000000000000, 0.9807852804032304306, 1.000000000000000000, 0.9807852804032304306, 1.000000000000000000, 0.9807852804032304306, 1.000000000000000000, 0.9807852804032304306, 1.000000000000000000, 0.9807852804032304306, 1.000000000000000000, 0.9807852804032304306, 1.000000000000000000, 0.9807852804032304306, 1.000000000000000000, 0.9807852804032304306, 1.000000000000000000, 0.9807852804032304306, 1.000000000000000000, 0.9807852804032304306, 1.000000000000000000, 0.9807852804032304306, 1.000000000000000000, 0.9807852804032304306, 1.000000000000000000, 0.9807852804032304306, 1.000000000000000000, 0.9807852804032304306, 1.000000000000000000, 0.9807852804032304306, 1.000000000000000000, 0.9807852804032304306, 1.000000000000000000, 0.9807852804032304306, 1.000000000000000000, 0.9807852804032304306, 1.000000000000000000, 0.9807852804032304306, 1.000000000000000000, 0.9807852804032304306, 1.000000000000000000, 0.9807852804032304306, 1.000000000000000000, 0.9807852804032304306, 1.000000000000000000, 0.9807852804032304306, 1.000000000000000000, 0.9807852804032304306, 1.000000000000000000, 0.9807852804032304306, 1.000000000000000000, 0.9807852804032304306, 1.000000000000000000, 0.9807852804032304306, 1.000000000000000000, 0.9807852804032304306, 1.000000000000000000, 0.9807852804032304306, 1.000000000000000000, 0.9807852804032304306, 1.000000000000000000, 0.9807852804032304306, 1.000000000000000000, 0.9807852804032304306, 1.000000000000000000, 0.9807852804032304306, 1.000000000000000000, 0.9807852804032304306, 1.000000000000000000, 0.9807852804032304306, 1.000000000000000000, 0.9807852804032304306, 1.000000000000000000, 0.9807852804032304306, 1.000000000000000000, 0.9807852804032304306, 1.000000000000000000, 0.9807852804032304306, 1.000000000000000000, 0.9807852804032304306, 1.000000000000000000, 0.9807852804032304306, 1.000000000000000000, 0.9807852804032304306, 1.000000000000000000, 0.9807852804032304306, 1.000000000000000000, 0.9807852804032304306, 1.000000000000000000, 0.9807852804032304306, 1.000000000000000000, 0.9807852804032304306, 1.000000000000000000, 0.9807852804032304306, 1.000000000000000000, 0.9807852804032304306, 1.000000000000000000, 0.9807852804032304306, 1.000000000000000000, 0.9807852804032304306, 1.000000000000000000, 0.9807852804032304306, 1.000000000000000000, 0.9807852804032304306, 1.000000000000000000, 0.9807852804032304306, 1.000000000000000000, 0.9807852804032304306, 1.000000000000000000, 0.9807852804032304306, 1.000000000000000000, 0.9807852804032304306, 1.000000000000000000, 0.9807852804032304306, 1.000000000000000000, 0.9807852804032304306, 1.000000000000000000, 0.9807852804032304306, 1.000000000000000000, 0.9807852804032304306, 1.000000000000000000, 0.9807852804032304306, 1.000000000000000000, 0.9807852804032304306, 1.000000000000000000, 0.9807852804032304306, 1.000000000000000000, 0.9807852804032304306, 1.000000000000000000, 0.9807852804032304306, 1.000000000000000000, 0.9807852804032304306, 1.000000000000000000, 0.9807852804032304306, 1.000000000000000000, 0.9807852804032304306, 1.000000000000000000, 0.9807852804032304306, 1.000000000000000000, 0.9807852804032304306, 1.000000000000000000, 0.9807852804032304306, 1.000000000000000000, 0.9807852804032304306, 1.000000000000000000, 0.9807852804032304306, 1.000000000000000000, 0.9807852804032304306, 1.000000000000000000, 0.9807852804032304306, 1.000000000000000000, 0.9807852804032304306, 1.000000000000000000, 0.9807852804032304306, 1.000000000000000000, 0.9807852804032304306, 1.000000000000000000, 0.9807852804032304306, 1.000000000000000000, 0.9807852804032304306, 1.000000000000000000, 0.9807852804032304306, 1.000000000000000000, 0.9807852804032304306, 1.000000000000000000, 0.9807852804032304306, 1.000000000000000000, 0.9807852804032304306, 1.000000000000000000, 0.9807852804032304306, 1.000000000000000000, 0.9807852804032304306, 1.000000000000000000, 0.9807852804032304306, 1.000000000000000000, 0.9807852804032304306, 1.000000000000000000, 0.9807852804032304306, 1.000000000000000000, 0.9807852804032304306, 1.000000000000000000, 0.9807852804032304306, 1.000000000000000000, 0.9807852804032304306, 1.000000000000000000, 0.9807852804032304306, 1.000000000000000000, 0.9807852804032304306, 1.000000000000000000, 0.9807852804032304306, 1.000000000000000000, 0.9807852804032304306, 1.000000000000000000, 0.9807852804032304306, 1.000000000000000000, 0.9807852804032304306, 1.000000000000000000, 0.9807852804032304306, 1.000000000000000000, 0.9807852804032304306, 1.000000000000000000, 0.9807852804032304306, 1.000000000000000000, 0.9807852804032304306, 1.000000000000000000, 0.9807852804032304306, 1.000000000000000000, 0.9807852804032304306, 1.000000000000000000, 0.9807852804032304306, 1.000000000000000000 ) ) 
 REPRESENTATION_ITEM ( '' )  );
#12144 = EDGE_CURVE ( 'NONE', #972, #4178, #1954, .T. ) ;
#12145 = CARTESIAN_POINT ( 'NONE',  ( 31.27239372959508756, -6.928203230275514990, 167.4139976038384532 ) ) ;
#12146 = ORIENTED_EDGE ( 'NONE', *, *, #13809, .T. ) ;
#12147 = CARTESIAN_POINT ( 'NONE',  ( 19.68408634441912142, -5.407089921784861808, -3.196874999385534988 ) ) ;
#12148 = FACE_OUTER_BOUND ( 'NONE', #18874, .T. ) ;
#12149 = CARTESIAN_POINT ( 'NONE',  ( 27.93288733171263516, 5.407089921784862696, 165.0617286715140608 ) ) ;
#12150 = AXIS2_PLACEMENT_3D ( 'NONE', #23312, #20476, #29164 ) ;
#12151 = CARTESIAN_POINT ( 'NONE',  ( -65.43377896937850835, 207.8379586601372750, 8.530955311639258909 ) ) ;
#12152 = DIRECTION ( 'NONE',  ( -1.000000000000000000, -6.123233995736766036E-17, 0.000000000000000000 ) ) ;
#12153 =( NAMED_UNIT ( * ) PLANE_ANGLE_UNIT ( ) SI_UNIT ( $, .RADIAN. ) );
#12154 = EDGE_CURVE ( 'NONE', #10052, #16958, #21360, .T. ) ;
#12155 = CARTESIAN_POINT ( 'NONE',  ( 15.00000000000000355, 7.347880794884112834E-16, 50.26196565745150480 ) ) ;
#12156 = CARTESIAN_POINT ( 'NONE',  ( -64.04836230271183695, 206.0451222850691977, -2.149950860017851184 ) ) ;
#12157 = CARTESIAN_POINT ( 'NONE',  ( 28.05502581071438328, -5.196152422706632912, 165.0604537508149008 ) ) ;
#12158 = CARTESIAN_POINT ( 'NONE',  ( 24.87690945940258302, -3.604726614523240613, 165.9502056158071355 ) ) ;
#12159 = VERTEX_POINT ( 'NONE', #10544 ) ;
#12160 =( BOUNDED_CURVE ( )  B_SPLINE_CURVE ( 2, ( #31960, #6747, #35732, #9217, #17754, #15091, #20788 ),
 .UNSPECIFIED., .F., .F. ) 
 B_SPLINE_CURVE_WITH_KNOTS ( ( 3, 2, 2, 3 ),
 ( 0.9347826086956532166, 0.9420289855072474516, 0.9492753623188416867, 0.9565217391304360328 ),
 .UNSPECIFIED. ) 
 CURVE ( )  GEOMETRIC_REPRESENTATION_ITEM ( )  RATIONAL_B_SPLINE_CURVE ( ( 0.9999999999999815703, 0.8660254037844571373, 1.000000000000000000, 0.8660254037844387076, 1.000000000000000000, 0.8660254037844161701, 1.000000000000022649 ) ) 
 REPRESENTATION_ITEM ( '' )  );
#12161 = DIRECTION ( 'NONE',  ( 0.000000000000000000, 1.000000000000000000, 0.000000000000000000 ) ) ;
#12162 = CARTESIAN_POINT ( 'NONE',  ( 15.50000000000000533, 136.9101862821014777, 0.1745138560725827404 ) ) ;
#12163 = CARTESIAN_POINT ( 'NONE',  ( -60.69122103062156981, 207.8379586601371329, -8.530955311639223382 ) ) ;
#12164 = CARTESIAN_POINT ( 'NONE',  ( -3.474262827703337830, 134.0351862821014493, -8.843639120294326972 ) ) ;
#12165 = CARTESIAN_POINT ( 'NONE',  ( 18.00000000000000355, 246.5312500012290400, 5.196152422706632912 ) ) ;
#12166 = CARTESIAN_POINT ( 'NONE',  ( 8.962234695871762469, 34.56018628210144783, -8.715434833791931624 ) ) ;
#12167 = CARTESIAN_POINT ( 'NONE',  ( 13.56230152254411792, -5.196152422706638241, -6.225000000000063594 ) ) ;
#12168 = ORIENTED_EDGE ( 'NONE', *, *, #11552, .F. ) ;
#12169 = CARTESIAN_POINT ( 'NONE',  ( 5.438367727407757144E-14, 197.7500000012290400, -27.00000000000000000 ) ) ;
#12170 = CARTESIAN_POINT ( 'NONE',  ( -13.04141134922759804, 123.9726862821014493, -8.927990412390657937 ) ) ;
#12171 = CARTESIAN_POINT ( 'NONE',  ( 19.39230484541326760, 242.4424038105676686, 5.999999999999999112 ) ) ;
#12172 = CARTESIAN_POINT ( 'NONE',  ( -9.465287035748065847, 3.797686282101448096, -2.064181346179273735 ) ) ;
#12173 = CARTESIAN_POINT ( 'NONE',  ( -27.24356964375000345, 194.9093750006145456, 0.000000000000000000 ) ) ;
#12174 = DIRECTION ( 'NONE',  ( -0.000000000000000000, -1.000000000000000000, -0.000000000000000000 ) ) ;
#12175 = CARTESIAN_POINT ( 'NONE',  ( 22.53918047650689616, -0.9001358824703226125, -10.00000000000000355 ) ) ;
#12176 = CARTESIAN_POINT ( 'NONE',  ( 10.49999999999999645, 237.0000000000000000, -5.000000000000000000 ) ) ;
#12177 = CARTESIAN_POINT ( 'NONE',  ( 36.64165061258780298, 7.347880794884117764E-16, 159.9426051293869477 ) ) ;
#12178 = CARTESIAN_POINT ( 'NONE',  ( 26.75643035624999655, 242.4718750006145456, -3.323476615752271712 ) ) ;
#12179 = CARTESIAN_POINT ( 'NONE',  ( -8.152565276336593669, 80.95231371789854791, -5.233372021372610483 ) ) ;
#12180 = CARTESIAN_POINT ( 'NONE',  ( 20.99999999999999645, 240.5218750006145285, 6.646953231504538984 ) ) ;
#12181 = AXIS2_PLACEMENT_3D ( 'NONE', #1310, #24445, #26711 ) ;
#12182 = ORIENTED_EDGE ( 'NONE', *, *, #33078, .F. ) ;
#12183 = CARTESIAN_POINT ( 'NONE',  ( 18.00000000000000000, 245.4812500012290570, -5.196152422706630247 ) ) ;
#12184 = CARTESIAN_POINT ( 'NONE',  ( -2.660918448318005058, 91.30231371789855643, -12.46528703574811558 ) ) ;
#12185 = EDGE_CURVE ( 'NONE', #6022, #28136, #10730, .T. ) ;
#12186 = CARTESIAN_POINT ( 'NONE',  ( 22.80587116629412492, 3.604726614523243278, -3.534374999385544669 ) ) ;
#12187 = CARTESIAN_POINT ( 'NONE',  ( 19.39230484541324628, 246.7575961894322631, -5.999999999999989342 ) ) ;
#12188 = CARTESIAN_POINT ( 'NONE',  ( 21.00000000000000000, 6.646953231504538984, -2.615624999385474325 ) ) ;
#12189 = CARTESIAN_POINT ( 'NONE',  ( -12.53471296425189152, 71.17731371789855643, -2.311890736173453753 ) ) ;
#12190 = CARTESIAN_POINT ( 'NONE',  ( -1.926257025242585782E-15, 197.4968750006145513, -31.45816453501075927 ) ) ;
#12191 = ORIENTED_EDGE ( 'NONE', *, *, #10512, .T. ) ;
#12192 = ORIENTED_EDGE ( 'NONE', *, *, #1022, .F. ) ;
#12193 = CARTESIAN_POINT ( 'NONE',  ( 23.87821517812499650, 4.985214923628404904, -4.790624999385456384 ) ) ;
#12194 = CYLINDRICAL_SURFACE ( 'NONE', #7612, 5.999999999999998224 ) ;
#12195 = CARTESIAN_POINT ( 'NONE',  ( 15.24356964374999990, 245.6968750006145115, 0.000000000000000000 ) ) ;
#12196 = CARTESIAN_POINT ( 'NONE',  ( -11.48171059495397373, 40.88518628210144357, -4.944772684328680334 ) ) ;
#12197 = CARTESIAN_POINT ( 'NONE',  ( -44.65252896937850835, 206.6499508600178387, -5.571401726697954970 ) ) ;
#12198 = CARTESIAN_POINT ( 'NONE',  ( 14.16903250679951043, 216.8309674931686004, -1.338899061176967997 ) ) ;
#12199 = CARTESIAN_POINT ( 'NONE',  ( -34.75669563604515844, 209.8844732041982297, -4.499999999999996447 ) ) ;
#12200 = SURFACE_SIDE_STYLE ('',( #26602 ) ) ;
#12201 =( BOUNDED_CURVE ( )  B_SPLINE_CURVE ( 2, ( #12264, #35191, #9238, #17966, #29508, #3549, #26663, #23835, #35376 ),
 .UNSPECIFIED., .F., .T. ) 
 B_SPLINE_CURVE_WITH_KNOTS ( ( 3, 2, 2, 2, 3 ),
 ( 0.4021739130434782705, 0.4057971014492753881, 0.4130434782608695676, 0.4202898550724637472, 0.4239130434782608647 ),
 .UNSPECIFIED. ) 
 CURVE ( )  GEOMETRIC_REPRESENTATION_ITEM ( )  RATIONAL_B_SPLINE_CURVE ( ( 0.9330127018922194093, 0.9330127018922194093, 1.000000000000000000, 0.8660254037844387076, 1.000000000000000000, 0.8660254037844387076, 1.000000000000000000, 0.9330127018922194093, 0.9330127018922194093 ) ) 
 REPRESENTATION_ITEM ( '' )  );
#12202 = CARTESIAN_POINT ( 'NONE',  ( 24.78863278643100188, -3.464101615137757051, 162.1465503788904243 ) ) ;
#12203 = AXIS2_PLACEMENT_3D ( 'NONE', #5547, #7854, #27753 ) ;
#12204 = CARTESIAN_POINT ( 'NONE',  ( 8.715434833792128799, 92.73981371789855643, -8.962234695871567070 ) ) ;
#12205 = CARTESIAN_POINT ( 'NONE',  ( -59.50372103062157692, 214.5309553116392749, -1.090244570138262148 ) ) ;
#12206 = CARTESIAN_POINT ( 'NONE',  ( -31.99330436395490196, 210.1155267958016850, -8.500000000000003553 ) ) ;
#12207 = CARTESIAN_POINT ( 'NONE',  ( 20.99999999999999645, 6.646953231504538984, -6.665624999385467930 ) ) ;
#12208 = DIRECTION ( 'NONE',  ( 0.000000000000000000, 0.000000000000000000, 1.000000000000000000 ) ) ;
#12209 = CARTESIAN_POINT ( 'NONE',  ( 3.257655550456945548, 59.10231371789854649, 15.46528703574811736 ) ) ;
#12210 = CARTESIAN_POINT ( 'NONE',  ( -56.92336230271183695, 217.4189793300686233, 4.149950860017807663 ) ) ;
#12211 = AXIS2_PLACEMENT_3D ( 'NONE', #11298, #22687, #95 ) ;
#12212 = CARTESIAN_POINT ( 'NONE',  ( 15.00000000000000000, 0.000000000000000000, -0.8437499987709595750 ) ) ;
#12213 = CARTESIAN_POINT ( 'NONE',  ( 12.53471296425194836, 81.42268628210145209, -2.311890736173178418 ) ) ;
#12214 = CARTESIAN_POINT ( 'NONE',  ( 11.08355503943142750, 43.76018628210144357, -10.83675517735155225 ) ) ;
#12216 = ADVANCED_FACE ( 'NONE', ( #10916 ), #34039, .T. ) ;
#12215 = CARTESIAN_POINT ( 'NONE',  ( 22.56230152254411436, -3.464101615137755275, -0.7125000000000065725 ) ) ;
#12217 = CARTESIAN_POINT ( 'NONE',  ( 24.35887751344623098, 0.000000000000000000, 160.0290733790243962 ) ) ;
#12218 = CARTESIAN_POINT ( 'NONE',  ( -15.53471296425195369, 49.22268628210144215, 2.908627838312118019 ) ) ;
#12219 = CARTESIAN_POINT ( 'NONE',  ( 27.24356964374999279, 199.1656250006145399, -15.72908226750539207 ) ) ;
#12220 = CARTESIAN_POINT ( 'NONE',  ( 10.31873187879411091, 3.604726614523236616, -9.628124999385549998 ) ) ;
#12221 = CARTESIAN_POINT ( 'NONE',  ( 10.56230152254371824, -3.464101615137531009, -2.662500000000047162 ) ) ;
#12222 = CARTESIAN_POINT ( 'NONE',  ( -54.75372103062154849, 216.5309553116391612, -1.626142955000564383 ) ) ;
#12223 = CARTESIAN_POINT ( 'NONE',  ( 24.00000000000000000, 241.2062500012290513, 5.196152422706629359 ) ) ;
#12224 = CARTESIAN_POINT ( 'NONE',  ( 10.49813415415989581, 27.37268628210144783, 7.228626920339068285 ) ) ;
#12225 = CARTESIAN_POINT ( 'NONE',  ( 20.99999999999999645, 192.3000000000000398, 0.000000000000000000 ) ) ;
#12226 = CARTESIAN_POINT ( 'NONE',  ( 5.529263428287300108, 141.3273137178985621, 7.954856959092309943 ) ) ;
#12227 = CARTESIAN_POINT ( 'NONE',  ( 15.24356964375000167, 247.6468750006145854, 3.323476615752272600 ) ) ;
#12228 = ORIENTED_EDGE ( 'NONE', *, *, #24193, .F. ) ;
#12229 = CARTESIAN_POINT ( 'NONE',  ( 15.00000000000000178, -3.464101615137757051, -8.062499999999991118 ) ) ;
#12230 = CARTESIAN_POINT ( 'NONE',  ( 14.99999999999936229, 3.464101615137384904, -3.187499999999991118 ) ) ;
#12231 = ADVANCED_FACE ( 'NONE', ( #11474 ), #5780, .T. ) ;
#12232 = LINE ( 'NONE', #29477, #17113 ) ;
#12233 = CARTESIAN_POINT ( 'NONE',  ( 10.31873187879410914, 0.000000000000000000, -3.290624999385538541 ) ) ;
#12234 = CARTESIAN_POINT ( 'NONE',  ( 31.14247720061542424, -7.209453229046475009, 165.9290448826076272 ) ) ;
#12235 = CARTESIAN_POINT ( 'NONE',  ( 21.00000000000000000, 242.2374999999999829, -6.928203230275506996 ) ) ;
#12236 = CARTESIAN_POINT ( 'NONE',  ( 27.00000000000001066, 199.7375000000000114, 15.58845726811988897 ) ) ;
#12237 = CARTESIAN_POINT ( 'NONE',  ( 4.622313124798573369, 46.63518628210145067, 11.61527771782819940 ) ) ;
#12238 = ORIENTED_EDGE ( 'NONE', *, *, #37101, .F. ) ;
#12239 = ORIENTED_EDGE ( 'NONE', *, *, #29268, .T. ) ;
#12240 = CARTESIAN_POINT ( 'NONE',  ( 7.234628195640363302, 196.8299038117967257, -26.99999999999996803 ) ) ;
#12241 = CARTESIAN_POINT ( 'NONE',  ( 22.56230152254412147, 7.347880794884125653E-16, -3.825000000000050804 ) ) ;
#12242 = DIRECTION ( 'NONE',  ( 0.000000000000000000, 0.000000000000000000, 1.000000000000000000 ) ) ;
#12243 = CARTESIAN_POINT ( 'NONE',  ( 5.438367727407757144E-14, 198.2000000012290002, -27.00000000000000000 ) ) ;
#12244 = CARTESIAN_POINT ( 'NONE',  ( 26.75643035624999655, 7.049594010296217766E-16, -5.315624999385482496 ) ) ;
#12245 = CARTESIAN_POINT ( 'NONE',  ( 11.48171059495397728, 91.48518628210145209, 4.944772684328674117 ) ) ;
#12246 = CARTESIAN_POINT ( 'NONE',  ( 14.38691631536194393, 11.66481371789854293, 5.770363421894124656 ) ) ;
#12247 = DIRECTION ( 'NONE',  ( 1.000000000000000000, 0.000000000000000000, 0.000000000000000000 ) ) ;
#12248 = EDGE_CURVE ( 'NONE', #8427, #15760, #7075, .T. ) ;
#12249 = CARTESIAN_POINT ( 'NONE',  ( -3.253724281355068545E-15, 195.9500000012290002, -27.00000000000000355 ) ) ;
#12250 = CARTESIAN_POINT ( 'NONE',  ( -34.96205436395489841, 213.2096571498974242, 3.378800118222489601 ) ) ;
#12251 = CARTESIAN_POINT ( 'NONE',  ( 21.00000000000000355, 0.000000000000000000, 50.00000000000001421 ) ) ;
#12252 = CARTESIAN_POINT ( 'NONE',  ( 36.81484116775207127, -3.604726614523238837, 159.1275339855211257 ) ) ;
#12253 = CARTESIAN_POINT ( 'NONE',  ( 0.1745138560722779009, 132.9898137178985564, 12.50000000000000355 ) ) ;
#12254 = CARTESIAN_POINT ( 'NONE',  ( -63.65997103062156981, 215.5714017266979852, 3.350049139982118618 ) ) ;
#12255 =( BOUNDED_CURVE ( )  B_SPLINE_CURVE ( 2, ( #7360, #13610, #25345, #21956, #33133, #36151, #27440 ),
 .UNSPECIFIED., .F., .F. ) 
 B_SPLINE_CURVE_WITH_KNOTS ( ( 3, 2, 2, 3 ),
 ( 0.3478260869565210078, 0.3550724637681152984, 0.3623188405797095890, 0.3695652173913038241 ),
 .UNSPECIFIED. ) 
 CURVE ( )  GEOMETRIC_REPRESENTATION_ITEM ( )  RATIONAL_B_SPLINE_CURVE ( ( 1.000000000000013323, 0.8660254037844252739, 1.000000000000000000, 0.8660254037844387076, 1.000000000000000000, 0.8660254037844479225, 0.9999999999999907851 ) ) 
 REPRESENTATION_ITEM ( '' )  );
#12256 = CARTESIAN_POINT ( 'NONE',  ( -65.24330436395489130, 210.1155267958016850, -8.500000000000003553 ) ) ;
#12257 = DIRECTION ( 'NONE',  ( 1.000000000000000000, 0.000000000000000000, 0.000000000000000000 ) ) ;
#12258 = CARTESIAN_POINT ( 'NONE',  ( 15.24356964374999990, 0.000000000000000000, -0.7031249993854904456 ) ) ;
#12259 = CARTESIAN_POINT ( 'NONE',  ( 13.62178482187499640, 198.3031250006145285, -23.59362340125807123 ) ) ;
#12260 = CARTESIAN_POINT ( 'NONE',  ( 13.23911966647199812, 140.7523137178985166, 8.632099005475788900 ) ) ;
#12261 = CARTESIAN_POINT ( 'NONE',  ( -56.72544563604517265, 214.8429017333602360, 4.673758765035156415 ) ) ;
#12262 = ORIENTED_EDGE ( 'NONE', *, *, #8908, .F. ) ;
#12263 = CARTESIAN_POINT ( 'NONE',  ( -11.48171059495397373, 40.88518628210144357, -4.944772684328680334 ) ) ;
#12264 = CARTESIAN_POINT ( 'NONE',  ( 20.99999999999999289, 245.4437500012290343, -5.999999999999997335 ) ) ;
#12265 = CIRCLE ( 'NONE', #11076, 4.000000000000003553 ) ;
#12266 = CARTESIAN_POINT ( 'NONE',  ( 20.53679726638638314, 5.749653476603932667, -8.000000000000005329 ) ) ;
#12267 = CARTESIAN_POINT ( 'NONE',  ( 24.94391043663983965, 3.604726614523240613, 166.7160302899652322 ) ) ;
#12268 = CARTESIAN_POINT ( 'NONE',  ( 8.927990412390657937, 107.8726862821014549, -13.04141134922759804 ) ) ;
#12269 = CARTESIAN_POINT ( 'NONE',  ( -64.25372103062156270, 216.5309553116392181, -1.626142955000564383 ) ) ;
#12270 = CARTESIAN_POINT ( 'NONE',  ( 13.44051670066911441, 5.407089921784856479, -2.465624999385545912 ) ) ;
#12271 = CARTESIAN_POINT ( 'NONE',  ( -6.840914352312096547, 66.76018628210144357, 6.594114490232313663 ) ) ;
#12272 = ADVANCED_FACE ( 'NONE', ( #34959 ), #3122, .T. ) ;
#12273 = LINE ( 'NONE', #32545, #11017 ) ;
#12274 = CARTESIAN_POINT ( 'NONE',  ( 10.56230152254410903, 0.000000000000000000, -4.500000000000031974 ) ) ;
#12275 = CARTESIAN_POINT ( 'NONE',  ( 7.228626920339068285, 89.47268628210144925, -10.49813415415989581 ) ) ;
#12276 = CYLINDRICAL_SURFACE ( 'NONE', #6383, 27.00000000000000000 ) ;
#12277 = CARTESIAN_POINT ( 'NONE',  ( 20.99999999999999645, 185.0294372515228645, 0.000000000000000000 ) ) ;
#12278 = CARTESIAN_POINT ( 'NONE',  ( 30.63261610554166126, -7.209453229046475009, 160.1013058987709314 ) ) ;
#12279 = CARTESIAN_POINT ( 'NONE',  ( 23.87821517812500005, -4.985214923628404016, -8.990624999385465443 ) ) ;
#12280 = CARTESIAN_POINT ( 'NONE',  ( -4.694659320240884604E-14, 197.4124999999999943, 27.00000000000000000 ) ) ;
#12281 = CARTESIAN_POINT ( 'NONE',  ( 37.36719068741531657, 7.646167579472024665E-16, 165.4409178846775603 ) ) ;
#12282 = PRODUCT_DEFINITION_CONTEXT ( 'detailed design', #17071, 'design' ) ;
#12283 = CARTESIAN_POINT ( 'NONE',  ( 37.02731477413906447, 3.464101615137759271, 164.3507666672186076 ) ) ;
#12284 = DIRECTION ( 'NONE',  ( 0.000000000000000000, 0.000000000000000000, 1.000000000000000000 ) ) ;
#12285 = CARTESIAN_POINT ( 'NONE',  ( 15.00000000000000000, 247.7500000000000000, 0.000000000000000000 ) ) ;
#12286 = CARTESIAN_POINT ( 'NONE',  ( 27.24356964375000345, 196.8781250006145171, -3.336375036156643733E-15 ) ) ;
#12287 = ADVANCED_FACE ( 'NONE', ( #9004 ), #26616, .T. ) ;
#12288 = CARTESIAN_POINT ( 'NONE',  ( -8.962234695871565293, 108.8398137178985507, -8.715434833792128799 ) ) ;
#12289 = CARTESIAN_POINT ( 'NONE',  ( -6.932735513423968321, 96.94768628210145778, -10.69584247140445221 ) ) ;
#12290 = ORIENTED_EDGE ( 'NONE', *, *, #32495, .F. ) ;
#12291 = CARTESIAN_POINT ( 'NONE',  ( -13.62178482187500528, 195.6781250006145569, -23.59362340125807123 ) ) ;
#12292 = CARTESIAN_POINT ( 'NONE',  ( 26.75643035624999655, 240.9343750006144944, 3.323476615752267715 ) ) ;
#12293 = CARTESIAN_POINT ( 'NONE',  ( -14.25334919248795096, 70.31481371789853085, 6.092822981423662299 ) ) ;
#12294 = CARTESIAN_POINT ( 'NONE',  ( 21.00000000000000000, 6.646953231504538984, -4.865624999385484983 ) ) ;
#12295 = CARTESIAN_POINT ( 'NONE',  ( 26.75643035624999655, 247.3468750006145171, 3.323476615752267715 ) ) ;
#12296 = CARTESIAN_POINT ( 'NONE',  ( 8.710071997420127943, 91.48518628210145209, 3.796722387233375073 ) ) ;
#12297 = CARTESIAN_POINT ( 'NONE',  ( 5.727106289114498080E-15, 194.8250000012290570, 31.17691453623979214 ) ) ;
#12298 = CARTESIAN_POINT ( 'NONE',  ( -8.843639120294245259, 71.46481371789856496, -3.474262827703533230 ) ) ;
#12299 = CARTESIAN_POINT ( 'NONE',  ( 22.80587116629410716, 7.646167579472015790E-16, -6.215624999385549465 ) ) ;
#12300 = CARTESIAN_POINT ( 'NONE',  ( -6.594114490232462877, 106.5398137178985536, 6.840914352311949109 ) ) ;
#12301 = CARTESIAN_POINT ( 'NONE',  ( 18.12178482187499640, 242.4718750006145171, -4.985214923628404904 ) ) ;
#12302 = CARTESIAN_POINT ( 'NONE',  ( 2.660918448318002838, 49.90231371789855075, 12.46528703574811558 ) ) ;
#12303 = PRESENTATION_LAYER_ASSIGNMENT (  '', '', ( #30481 ) ) ;
#12304 = CARTESIAN_POINT ( 'NONE',  ( -1.045839947578415010E-13, 196.0625000000000284, 27.00000000000000355 ) ) ;
#12305 = CARTESIAN_POINT ( 'NONE',  ( -8.715434833791929847, 105.8601862821014521, -8.962234695871762469 ) ) ;
#12306 = CARTESIAN_POINT ( 'NONE',  ( 22.56230152254411081, 3.464101615137755275, -6.824999998770996612 ) ) ;
#12307 = CARTESIAN_POINT ( 'NONE',  ( -33.77455436395490551, 205.1570982666397356, 4.673758765035198159 ) ) ;
#12308 = CARTESIAN_POINT ( 'NONE',  ( -2.311890736173176641, 134.3226862821014436, -12.53471296425194836 ) ) ;
#12309 = CARTESIAN_POINT ( 'NONE',  ( 24.71676078210377625, 0.000000000000000000, 164.1196978580636028 ) ) ;
#12310 = CARTESIAN_POINT ( 'NONE',  ( 14.25334919248782661, 91.48518628210145209, 6.092822981423971385 ) ) ;
#12311 = CARTESIAN_POINT ( 'NONE',  ( 16.56230152254411436, -7.209453229046482114, -3.684374999385500615 ) ) ;
#12312 = CARTESIAN_POINT ( 'NONE',  ( 20.99999999999998579, 248.3124999999999716, 5.999999999999998224 ) ) ;
#12313 = LINE ( 'NONE', #26522, #32149 ) ;
#12314 = CARTESIAN_POINT ( 'NONE',  ( -27.00000000000000355, 199.0999999999999943, 0.000000000000000000 ) ) ;
#12315 = CARTESIAN_POINT ( 'NONE',  ( 8.710071997420127943, 119.0851862821014606, 3.796722387233375073 ) ) ;
#12316 = DIRECTION ( 'NONE',  ( -0.000000000000000000, -0.000000000000000000, 1.000000000000000000 ) ) ;
#12317 = CARTESIAN_POINT ( 'NONE',  ( 8.632099005475504683, 18.74768628210143362, 13.23911966647218996 ) ) ;
#12318 = AXIS2_PLACEMENT_3D ( 'NONE', #35104, #12174, #32453 ) ;
#12319 = CARTESIAN_POINT ( 'NONE',  ( -1.926257025242585782E-15, 196.1468750006145285, -31.45816453501075927 ) ) ;
#12320 = CARTESIAN_POINT ( 'NONE',  ( 26.75643035624999655, 243.2593750006145115, -3.323476615752271712 ) ) ;
#12321 = ORIENTED_EDGE ( 'NONE', *, *, #14077, .T. ) ;
#12322 = CARTESIAN_POINT ( 'NONE',  ( 25.03052145599531997, 0.000000000000000000, 167.7059987711938902 ) ) ;
#12323 = CARTESIAN_POINT ( 'NONE',  ( 23.87821517812500005, -4.985214923628404016, -2.240624999385460114 ) ) ;
#12324 = CARTESIAN_POINT ( 'NONE',  ( 5.778771075727756162E-15, 199.5218750006145569, 31.45816453501076637 ) ) ;
#12325 = DIRECTION ( 'NONE',  ( -0.9848055780335318588, 2.371220701776928982E-05, 0.1736605105133940674 ) ) ;
#12326 = CARTESIAN_POINT ( 'NONE',  ( 22.56230152254410370, 7.347880794884117764E-16, -5.962499998771020771 ) ) ;
#12327 = CARTESIAN_POINT ( 'NONE',  ( 13.49999999999999645, 198.5000000000000000, -23.38268590217984766 ) ) ;
#12328 = CARTESIAN_POINT ( 'NONE',  ( 7.954856959092311719, 28.62731371789854506, -5.529263428287300108 ) ) ;
#12329 = CARTESIAN_POINT ( 'NONE',  ( -1.926257025242585782E-15, 197.9468750006145399, -31.45816453501076637 ) ) ;
#12331 = ORIENTED_EDGE ( 'NONE', *, *, #5987, .F. ) ;
#12330 = ORIENTED_EDGE ( 'NONE', *, *, #24996, .T. ) ;
#12332 = CARTESIAN_POINT ( 'NONE',  ( 26.75643035624999655, 246.4093750006145171, -3.323476615752271712 ) ) ;
#12333 = CARTESIAN_POINT ( 'NONE',  ( 2.311890736173452421, 27.47731371789855004, -12.53471296425189152 ) ) ;
#12334 = CARTESIAN_POINT ( 'NONE',  ( 18.12178482187500350, -4.985214923628407568, -2.315624999385479388 ) ) ;
#12335 = CARTESIAN_POINT ( 'NONE',  ( -2.908627838312453306, 124.0773137178985621, 15.53471296425188797 ) ) ;
#12336 = AXIS2_PLACEMENT_3D ( 'NONE', #12467, #21389, #3932 ) ;
#12337 = CARTESIAN_POINT ( 'NONE',  ( 26.99999999999999645, -3.464101615137751278, -7.856249998770961085 ) ) ;
#12338 = CARTESIAN_POINT ( 'NONE',  ( 0.000000000000000000, 2.000000000000000000, 0.000000000000000000 ) ) ;
#12339 = ORIENTED_EDGE ( 'NONE', *, *, #18881, .F. ) ;
#12340 = CARTESIAN_POINT ( 'NONE',  ( 16.56230152254411792, 7.209453229046482114, -4.359374999385510208 ) ) ;
#12341 = ORIENTED_EDGE ( 'NONE', *, *, #2771, .T. ) ;
#12342 = CARTESIAN_POINT ( 'NONE',  ( 27.24356964374999635, 197.3656250006145285, -15.72908226750539029 ) ) ;
#12343 = CARTESIAN_POINT ( 'NONE',  ( 31.00030439525832193, 7.209453229046482114, 164.3040022813455039 ) ) ;
#12344 = CARTESIAN_POINT ( 'NONE',  ( -62.86086230271182984, 214.1499508600178387, -7.418979330068641964 ) ) ;
#12345 = CARTESIAN_POINT ( 'NONE',  ( 0.000000000000000000, 210.0000000000000284, -28.99999999999999645 ) ) ;
#12346 = APPLICATION_PROTOCOL_DEFINITION ( 'draft international standard', 'automotive_design', 1998, #19249 ) ;
#12347 = CARTESIAN_POINT ( 'NONE',  ( -42.59364919042334918, 252.0388376121882175, -0.4999999999999995559 ) ) ;
#12348 = CARTESIAN_POINT ( 'NONE',  ( -39.90252896937850124, 207.6499508600178387, -3.839350919129087547 ) ) ;
#12350 = EDGE_CURVE ( 'NONE', #26752, #55, #3495, .T. ) ;
#12349 = CARTESIAN_POINT ( 'NONE',  ( 26.99999999999999645, 197.1125000000000114, -15.58845726811990495 ) ) ;
#12351 = CARTESIAN_POINT ( 'NONE',  ( 34.33409119757650529, -5.407089921784855591, 166.5908959372197558 ) ) ;
#12352 = ORIENTED_EDGE ( 'NONE', *, *, #6818, .T. ) ;
#12353 = LINE ( 'NONE', #23926, #13113 ) ;
#12354 = CARTESIAN_POINT ( 'NONE',  ( -8.632099005475501130, 133.7476862821013981, -13.23911966647218996 ) ) ;
#12355 = VECTOR ( 'NONE', #9951, 1000.000000000000000 ) ;
#12356 = CARTESIAN_POINT ( 'NONE',  ( -64.84747103062156270, 214.3500491399821044, -7.303452534266878793 ) ) ;
#12357 = CARTESIAN_POINT ( 'NONE',  ( -9.465287035748065847, 132.5976862821014493, -2.064181346179273735 ) ) ;
#12358 = AXIS2_PLACEMENT_3D ( 'NONE', #24560, #37225, #36852 ) ;
#12359 = CARTESIAN_POINT ( 'NONE',  ( 20.99999999999999645, 202.0000000000000000, 0.000000000000000000 ) ) ;
#12360 = CARTESIAN_POINT ( 'NONE',  ( -2.311890736173176641, 23.92268628210143788, -12.53471296425194836 ) ) ;
#12361=STYLED_ITEM('',(#37528),#33058);
#12362 = CARTESIAN_POINT ( 'NONE',  ( 10.56230152254410726, 3.464101615137757051, -5.887500000000069456 ) ) ;
#12363 = ORIENTED_EDGE ( 'NONE', *, *, #31285, .F. ) ;
#12364 = CARTESIAN_POINT ( 'NONE',  ( 26.99999999999999645, 197.6750000012290229, -15.58845726811990495 ) ) ;
#12365 = CARTESIAN_POINT ( 'NONE',  ( -6.092822981423970496, 130.5851862821014606, 14.25334919248782661 ) ) ;
#12366 = CARTESIAN_POINT ( 'NONE',  ( -81.72704584564829133, 216.6260876520869658, 7.500000000000000000 ) ) ;
#12367 = CARTESIAN_POINT ( 'NONE',  ( 5.233372021372610483, 138.4523137178985621, -8.152565276336593669 ) ) ;
#12368 = CARTESIAN_POINT ( 'NONE',  ( -13.62178482187498396, 197.6281250006145171, 23.59362340125808188 ) ) ;
#12370 = CARTESIAN_POINT ( 'NONE',  ( 13.49999999999999645, 195.9125000012290343, -23.38268590217984766 ) ) ;
#12369 =( BOUNDED_CURVE ( )  B_SPLINE_CURVE ( 3, ( #17173, #28900, #5965, #22862 ),
 .UNSPECIFIED., .F., .F. ) 
 B_SPLINE_CURVE_WITH_KNOTS ( ( 4, 4 ),
 ( 4.712388980384729642, 6.283185307179586232 ),
 .UNSPECIFIED. ) 
 CURVE ( )  GEOMETRIC_REPRESENTATION_ITEM ( )  RATIONAL_B_SPLINE_CURVE ( ( 1.000000000000000000, 0.8047378541243743744, 0.8047378541243743744, 1.000000000000000000 ) ) 
 REPRESENTATION_ITEM ( '' )  );
#12371 = CARTESIAN_POINT ( 'NONE',  ( 15.59980547062007616, -2.577807756931967287, -7.999999999999994671 ) ) ;
#12372 = ADVANCED_FACE ( 'NONE', ( #29269 ), #17727, .T. ) ;
#12373 = CARTESIAN_POINT ( 'NONE',  ( 24.99999999999999289, 0.000000000000000000, 50.00000000000000000 ) ) ;
#12374 = CARTESIAN_POINT ( 'NONE',  ( -3.474262827703527901, 78.36481371789855643, 8.843639120294245259 ) ) ;
#12375 = DIRECTION ( 'NONE',  ( 0.08715574274765150453, 0.000000000000000000, 0.9961946980917461003 ) ) ;
#12376 = ORIENTED_EDGE ( 'NONE', *, *, #16176, .F. ) ;
#12377 = CARTESIAN_POINT ( 'NONE',  ( 26.99999999999999645, 243.1187500012290172, -3.464101615137755275 ) ) ;
#12378 = CARTESIAN_POINT ( 'NONE',  ( 10.69584247140429589, 94.75231371789854506, 6.932735513424201024 ) ) ;
#12379 = CARTESIAN_POINT ( 'NONE',  ( 22.80587116629411781, 3.604726614523243278, -3.084374999385516514 ) ) ;
#12380 = FACE_OUTER_BOUND ( 'NONE', #15088, .T. ) ;
#12381 = CARTESIAN_POINT ( 'NONE',  ( 26.75643035624999655, -3.323476615752267715, -4.565624999385477167 ) ) ;
#12382 = CARTESIAN_POINT ( 'NONE',  ( -0.1745138560722763466, 54.78981371789855359, -12.50000000000000355 ) ) ;
#12383 = CARTESIAN_POINT ( 'NONE',  ( -27.24356964374999635, 198.0968750006145456, 15.72908226750539384 ) ) ;
#12384 = ADVANCED_FACE ( 'NONE', ( #8633 ), #8819, .T. ) ;
#12385 = EDGE_LOOP ( 'NONE', ( #5752, #24553, #10268, #37206 ) ) ;
#12386 = ORIENTED_EDGE ( 'NONE', *, *, #30218, .T. ) ;
#12387 = CARTESIAN_POINT ( 'NONE',  ( 15.24356964374999990, 0.000000000000000000, -5.990624999385463667 ) ) ;
#12388 = CARTESIAN_POINT ( 'NONE',  ( 22.56230152254349974, 3.464101615138115875, -1.087500000000032774 ) ) ;
#12389 = CARTESIAN_POINT ( 'NONE',  ( 26.75643035624999655, 243.7093750006145285, -3.323476615752271712 ) ) ;
#12390 = CARTESIAN_POINT ( 'NONE',  ( -10.49813415415989581, 41.17268628210144499, -7.228626920339068285 ) ) ;
#12391 = CARTESIAN_POINT ( 'NONE',  ( -38.71502896937850124, 215.5714017266979567, -3.350049139982168800 ) ) ;
#12392 = CARTESIAN_POINT ( 'NONE',  ( -63.05877896937850835, 211.6261429550004607, -6.530955311639245586 ) ) ;
#12393 = CARTESIAN_POINT ( 'NONE',  ( 30.67428744509644289, 6.928203230275506996, 160.5776114894082127 ) ) ;
#12394 = CARTESIAN_POINT ( 'NONE',  ( 4.944772684328420986, 86.41481371789855359, 11.48171059495408208 ) ) ;
#12395 = CARTESIAN_POINT ( 'NONE',  ( -52.97247103062156270, 207.6499508600178387, 3.839350919129076445 ) ) ;
#12396 = CARTESIAN_POINT ( 'NONE',  ( -35.15997103062156270, 217.3034525342668815, 4.350049139982096413 ) ) ;
#12397 = CARTESIAN_POINT ( 'NONE',  ( 15.24356964374999990, 3.323476615752268604, -6.140624999385478233 ) ) ;
#12398 = CARTESIAN_POINT ( 'NONE',  ( 22.56230152254358501, 3.464101615138066137, -7.387500000000006395 ) ) ;
#12399 = CARTESIAN_POINT ( 'NONE',  ( 14.38691631536194393, 57.66481371789855359, 5.770363421894124656 ) ) ;
#12400 = CARTESIAN_POINT ( 'NONE',  ( -62.46502896937850124, 217.3034525342667962, -4.350049139982195001 ) ) ;
#12401 = EDGE_CURVE ( 'NONE', #11787, #18467, #35437, .T. ) ;
#12402 = CARTESIAN_POINT ( 'NONE',  ( 30.85077782416043490, -6.928203230275506996, 162.5949057530440029 ) ) ;
#12403 = CARTESIAN_POINT ( 'NONE',  ( -12.46528703574805697, 86.59768628210144925, -2.660918448318280838 ) ) ;
#12404 = CARTESIAN_POINT ( 'NONE',  ( 8.927990412390657937, 34.27268628210144641, -13.04141134922759804 ) ) ;
#12405 = CARTESIAN_POINT ( 'NONE',  ( 5.438367727407757775E-14, 198.0875000000000057, -27.00000000000000355 ) ) ;
#12406 = CARTESIAN_POINT ( 'NONE',  ( 30.68654372136677821, 7.209453229046482114, 160.7177013682151596 ) ) ;
#12407 = CARTESIAN_POINT ( 'NONE',  ( -6.092822981423970496, 47.78518628210144215, 14.25334919248782661 ) ) ;
#12408 = CARTESIAN_POINT ( 'NONE',  ( 5.778771075727756162E-15, 198.5656250006145456, 31.45816453501076637 ) ) ;
#12409 = EDGE_CURVE ( 'NONE', #10799, #24633, #12369, .T. ) ;
#12410 = CARTESIAN_POINT ( 'NONE',  ( -27.12178482187499995, 199.9296875003072671, 0.000000000000000000 ) ) ;
#12411 = CIRCLE ( 'NONE', #19179, 2.649999999999999467 ) ;
#12412 = CARTESIAN_POINT ( 'NONE',  ( 10.56230152254410903, 0.000000000000000000, -2.700000000000063238 ) ) ;
#12413 = CARTESIAN_POINT ( 'NONE',  ( -40.70163769728823411, 215.6869285224996986, -3.149950860017881382 ) ) ;
#12414 = CARTESIAN_POINT ( 'NONE',  ( 10.56230152254411081, 0.000000000000000000, -7.537499998771012955 ) ) ;
#12415 = CARTESIAN_POINT ( 'NONE',  ( -8.715434833791929847, 13.86018628210145032, -8.962234695871762469 ) ) ;
#12416 = AXIS2_PLACEMENT_3D ( 'NONE', #5837, #36923, #34642 ) ;
#12417 = CARTESIAN_POINT ( 'NONE',  ( 15.00000000000000178, 247.3937500012290513, 3.464101615137757051 ) ) ;
#12418 = CARTESIAN_POINT ( 'NONE',  ( -8.710071997420207879, 125.5148137178985763, 3.796722387233182339 ) ) ;
#12419 = CARTESIAN_POINT ( 'NONE',  ( 18.12178482187500350, 245.4343750006145228, 4.985214923628407568 ) ) ;
#12420 = VERTEX_POINT ( 'NONE', #6347 ) ;
#12421 = CARTESIAN_POINT ( 'NONE',  ( 24.00000000000000000, -5.196152422706629359, -7.050000000000000711 ) ) ;
#12422 = CYLINDRICAL_SURFACE ( 'NONE', #21445, 5.999999999999999112 ) ;
#12423 = EDGE_CURVE ( 'NONE', #29694, #6323, #26191, .T. ) ;
#12424 = DIRECTION ( 'NONE',  ( 0.000000000000000000, 0.000000000000000000, 1.000000000000000000 ) ) ;
#12425 = CARTESIAN_POINT ( 'NONE',  ( 19.68408634441910721, 5.407089921784857367, -6.140624999385558169 ) ) ;
#12426 = CARTESIAN_POINT ( 'NONE',  ( 34.26872439051576436, 5.407089921784857367, 165.8437499136509814 ) ) ;
#12427 = DIRECTION ( 'NONE',  ( -0.9810603962227041341, -0.1736474146266793750, 0.08583166290373737961 ) ) ;
#12428 = CARTESIAN_POINT ( 'NONE',  ( 27.00000000000000355, 199.3249999999999886, -3.306546357697854128E-15 ) ) ;
#12429 = CARTESIAN_POINT ( 'NONE',  ( 6.932735513423970097, 55.54768628210145209, 10.69584247140445044 ) ) ;
#12430 = ORIENTED_EDGE ( 'NONE', *, *, #20852, .F. ) ;
#12431 = ORIENTED_EDGE ( 'NONE', *, *, #15030, .F. ) ;
#12432 = FACE_OUTER_BOUND ( 'NONE', #22931, .T. ) ;
#12433 = CARTESIAN_POINT ( 'NONE',  ( 20.99999999999999289, 243.5874999999999488, -5.999999999999997335 ) ) ;
#12434 = CARTESIAN_POINT ( 'NONE',  ( 23.99999999999999645, 246.6999999999999886, -5.196152422706631135 ) ) ;
#12435 = CARTESIAN_POINT ( 'NONE',  ( 13.50000000000001421, 195.2000000000000171, 23.38268590217984055 ) ) ;
#12436 = CARTESIAN_POINT ( 'NONE',  ( 23.87821517812499650, 4.985214923628404904, -7.490624999385464555 ) ) ;
#12437 = CARTESIAN_POINT ( 'NONE',  ( 4.944772684328679446, 98.38518628210145778, -11.48171059495397373 ) ) ;
#12438 = CARTESIAN_POINT ( 'NONE',  ( -13.04141134922778456, 24.02731371789854364, 8.927990412390377273 ) ) ;
#12439 = CARTESIAN_POINT ( 'NONE',  ( 1.120210788295102201E-13, 197.1875000000000568, -27.00000000000000711 ) ) ;
#12440 = EDGE_CURVE ( 'NONE', #17872, #6483, #21132, .T. ) ;
#12441 = CARTESIAN_POINT ( 'NONE',  ( 14.95628864315606421, 216.0437113568463303, 2.958957796639721582 ) ) ;
#12442 = CARTESIAN_POINT ( 'NONE',  ( -65.23586230271183695, 207.8500491399821613, 3.954877714930852495 ) ) ;
#12443 = AXIS2_PLACEMENT_3D ( 'NONE', #22698, #7726, #4871 ) ;
#12444 = DIRECTION ( 'NONE',  ( 0.000000000000000000, -1.000000000000000000, 0.000000000000000000 ) ) ;
#12445 = CARTESIAN_POINT ( 'NONE',  ( 24.35560917309319251, 3.604726614523240613, 159.9917160778459220 ) ) ;
#12446 = CARTESIAN_POINT ( 'NONE',  ( 3.474262827703532341, 9.364813717898543999, -8.843639120294245259 ) ) ;
#12447 = CARTESIAN_POINT ( 'NONE',  ( -53.96205436395489130, 214.6737587650352168, 4.842901733360204908 ) ) ;
#12448 = CARTESIAN_POINT ( 'NONE',  ( -69.39955436395489130, 216.3070033484980002, -6.137860380172975638 ) ) ;
#12449 = CARTESIAN_POINT ( 'NONE',  ( 22.56230152254410370, 7.347880794884117764E-16, -4.612499998771030008 ) ) ;
#12450 = CARTESIAN_POINT ( 'NONE',  ( 27.24356964374999635, 198.7156250006145513, -15.72908226750539029 ) ) ;
#12451 = CARTESIAN_POINT ( 'NONE',  ( -14.25334919248795096, 116.3148137178985735, 6.092822981423662299 ) ) ;
#12452 = CARTESIAN_POINT ( 'NONE',  ( -63.25669563604516554, 209.8844732041982013, -6.500000000000000888 ) ) ;
#12453 = ADVANCED_FACE ( 'NONE', ( #30408, #33247 ), #15631, .T. ) ;
#12454 = VERTEX_POINT ( 'NONE', #23978 ) ;
#12455 = CARTESIAN_POINT ( 'NONE',  ( -7.228626920339069173, 29.67268628210144499, 10.49813415415989581 ) ) ;
#12456 = CARTESIAN_POINT ( 'NONE',  ( -42.15435043487492095, 254.8329415120769283, 2.500000000000000000 ) ) ;
#12457 = DIRECTION ( 'NONE',  ( -0.000000000000000000, -1.000000000000000000, -0.000000000000000000 ) ) ;
#12458 = CARTESIAN_POINT ( 'NONE',  ( 31.23562490067698150, 7.209453229046482114, 166.9937279661931768 ) ) ;
#12459 = CARTESIAN_POINT ( 'NONE',  ( 13.04141134922759804, 110.1726862821014663, 8.927990412390657937 ) ) ;
#12460 = CARTESIAN_POINT ( 'NONE',  ( -62.07663769728823411, 204.3130714775002730, 3.149950860017883603 ) ) ;
#12461 = CARTESIAN_POINT ( 'NONE',  ( 10.31873187879411446, -3.604726614523240613, -2.803124999385555149 ) ) ;
#12462 = CARTESIAN_POINT ( 'NONE',  ( -6.594114490232312775, 59.86018628210145209, -6.840914352312096547 ) ) ;
#12463 = LINE ( 'NONE', #24032, #27344 ) ;
#12464 = CARTESIAN_POINT ( 'NONE',  ( -69.20163769728823411, 215.6869285224996986, -3.149950860017881382 ) ) ;
#12465 = CARTESIAN_POINT ( 'NONE',  ( -2.660918448318275509, 84.29768628210145209, 12.46528703574805874 ) ) ;
#12466 = CARTESIAN_POINT ( 'NONE',  ( 24.69385091608528526, 3.464101615137450185, 161.0631886434913440 ) ) ;
#12467 = CARTESIAN_POINT ( 'NONE',  ( -70.80918835584510873, 215.2843023367891249, 7.500000000000000000 ) ) ;
#12468 = LINE ( 'NONE', #29522, #28029 ) ;
#12469 = CARTESIAN_POINT ( 'NONE',  ( 24.36704836432882004, -3.604726614523240613, 160.1224666319704681 ) ) ;
#12470 = EDGE_CURVE ( 'NONE', #33602, #14808, #1208, .T. ) ;
#12471 = CARTESIAN_POINT ( 'NONE',  ( 15.24356964374999990, 3.323476615752268604, -9.178124999385456562 ) ) ;
#12472 = CARTESIAN_POINT ( 'NONE',  ( 22.56230152254396160, -3.464101615137847645, -6.562500000000048850 ) ) ;
#12473 = CARTESIAN_POINT ( 'NONE',  ( 34.26382187998621731, 5.407089921784862696, 165.7877139618832985 ) ) ;
#12474 = CARTESIAN_POINT ( 'NONE',  ( 25.08605175845023894, 3.464101615137757051, 165.5460647849041607 ) ) ;
#12475 = CARTESIAN_POINT ( 'NONE',  ( 16.56230152254410726, 0.000000000000000000, -10.00000000000000000 ) ) ;
#12476 = CARTESIAN_POINT ( 'NONE',  ( 15.00000000000000178, 247.3374999999999773, 3.464101615137757051 ) ) ;
#12477 = CARTESIAN_POINT ( 'NONE',  ( -13.62178482187500528, 195.6781250006145569, -23.59362340125807123 ) ) ;
#12478 = CARTESIAN_POINT ( 'NONE',  ( -12.46528703574811558, 107.4023137178985650, 2.660918448318003726 ) ) ;
#12479 = CARTESIAN_POINT ( 'NONE',  ( 12.46528703574805874, 100.3976862821014464, 2.660918448318279950 ) ) ;
#12480 = ORIENTED_EDGE ( 'NONE', *, *, #2868, .T. ) ;
#12481 = ORIENTED_EDGE ( 'NONE', *, *, #26262, .T. ) ;
#12482 = CARTESIAN_POINT ( 'NONE',  ( -1.926257025242585782E-15, 196.0906250006145228, -31.45816453501075927 ) ) ;
#12483 = CARTESIAN_POINT ( 'NONE',  ( 26.75643035624999655, 240.5218750006145001, -7.049594010296217766E-16 ) ) ;
#12484 = CARTESIAN_POINT ( 'NONE',  ( -13.04141134922778456, 79.22731371789853938, 8.927990412390377273 ) ) ;
#12485 =( BOUNDED_CURVE ( )  B_SPLINE_CURVE ( 2, ( #35380, #327, #3734, #1078, #20444, #35574, #34824, #15307, #8867, #29131, #21195, #29513, #6397, #11892, #6015, #3554, #15116, #32170, #6770, #26859, #23460, #15496, #29893, #9057, #26667, #26478, #6208, #14931, #697, #12269, #23840, #29700, #9430, #17780, #21008, #29323, #32542, #888, #3923, #6584, #12460, #27052, #21381, #24400, #27613, #18542, #24583, #36135, #30272, #32921, #10549, #27420, #9987, #10364, #18916, #15877, #33113, #33484, #10176, #7712, #21938, #7157, #19294, #21751, #33303, #7528, #24213, #1453, #6973, #21568, #19102, #16435, #7342, #30467, #18731, #30653, #4115, #2013, #30833, #4488, #30080, #16251, #4668, #16065, #4857, #27982, #4298, #12833, #1644, #36504, #27801, #13216, #24765, #13027, #1828, #35758, #36316, #13397, #9803, #24947, #22124, #33672, #15687, #27239, #1262, #35948, #17685, #29418, #17873, #14645, #13777, #36874, #2885, #28166, #29222, #13588, #26382, #35099, #8773, #2197, #10920, #14458, #22495, #25140, #3265, #23365, #19474, #34729, #26195, #31020, #20531, #36694, #10734, #14837, #22307, #32073, #33859, #7901, #417, #20345, #26013, #5042, #34915, #16624, #9148, #3076, #25325, #34042, #8087, #32258, #11983, #19661, #42, #5729, #31702, #6102, #17310, #28851, #23555, #11607, #20715, #23182, #6302, #31887, #5917, #17496, #29032, #8960, #233, #11796, #29988, #3643, #3450, #600, #21657, #15784, #18824, #29796, #32639, #23743, #21101, #32826, #35281, #4019, #15213, #6870, #24311, #10087, #7250, #793, #12934, #6680, #3828 ),
 .UNSPECIFIED., .F., .F. ) 
 B_SPLINE_CURVE_WITH_KNOTS ( ( 3, 2, 2, 2, 2, 2, 2, 2, 2, 2, 2, 2, 2, 2, 2, 2, 2, 2, 2, 2, 2, 2, 2, 2, 2, 2, 2, 2, 2, 2, 2, 2, 2, 2, 2, 2, 2, 2, 2, 2, 2, 2, 2, 2, 2, 2, 2, 2, 2, 2, 2, 2, 2, 2, 2, 2, 2, 2, 2, 2, 2, 2, 2, 2, 2, 2, 2, 2, 2, 2, 2, 2, 2, 2, 2, 2, 2, 2, 2, 2, 2, 2, 2, 2, 2, 2, 2, 2, 2, 2, 2, 2, 2, 2, 2, 2, 3 ),
 ( 0.000000000000000000, 0.01041666666666666609, 0.02083333333333333218, 0.03125000000000000000, 0.04166666666666666435, 0.05208333333333333565, 0.06250000000000000000, 0.07291666666666667129, 0.08333333333333332871, 0.09375000000000000000, 0.1041666666666666713, 0.1145833333333333287, 0.1250000000000000000, 0.1354166666666666574, 0.1458333333333333426, 0.1562500000000000000, 0.1666666666666666574, 0.1770833333333333426, 0.1875000000000000000, 0.1979166666666666574, 0.2083333333333333426, 0.2187500000000000000, 0.2291666666666666574, 0.2395833333333333426, 0.2500000000000000000, 0.2604166666666666852, 0.2708333333333333148, 0.2812500000000000000, 0.2916666666666666852, 0.3020833333333333148, 0.3125000000000000000, 0.3229166666666666852, 0.3333333333333333148, 0.3437500000000000000, 0.3541666666666666852, 0.3645833333333333148, 0.3750000000000000000, 0.3854166666666666852, 0.3958333333333333148, 0.4062500000000000000, 0.4166666666666666852, 0.4270833333333333148, 0.4375000000000000000, 0.4479166666666666852, 0.4583333333333333148, 0.4687500000000000000, 0.4791666666666666852, 0.4895833333333333148, 0.5000000000000000000, 0.5104166666666666297, 0.5208333333333333703, 0.5312500000000000000, 0.5416666666666666297, 0.5520833333333333703, 0.5625000000000000000, 0.5729166666666666297, 0.5833333333333333703, 0.5937500000000000000, 0.6041666666666666297, 0.6145833333333333703, 0.6250000000000000000, 0.6354166666666666297, 0.6458333333333333703, 0.6562500000000000000, 0.6666666666666666297, 0.6770833333333333703, 0.6875000000000000000, 0.6979166666666666297, 0.7083333333333333703, 0.7187500000000000000, 0.7291666666666666297, 0.7395833333333333703, 0.7500000000000000000, 0.7604166666666666297, 0.7708333333333333703, 0.7812500000000000000, 0.7916666666666666297, 0.8020833333333333703, 0.8125000000000000000, 0.8229166666666666297, 0.8333333333333333703, 0.8437500000000000000, 0.8541666666666666297, 0.8645833333333333703, 0.8750000000000000000, 0.8854166666666666297, 0.8958333333333333703, 0.9062500000000000000, 0.9166666666666666297, 0.9270833333333333703, 0.9375000000000000000, 0.9479166666666666297, 0.9583333333333333703, 0.9687500000000000000, 0.9791666666666666297, 0.9895833333333333703, 1.000000000000000000 ),
 .UNSPECIFIED. ) 
 CURVE ( )  GEOMETRIC_REPRESENTATION_ITEM ( )  RATIONAL_B_SPLINE_CURVE ( ( 1.000000000000000000, 0.9659258262890683122, 1.000000000000000000, 0.9659258262890683122, 1.000000000000000000, 0.9659258262890683122, 1.000000000000000000, 0.9659258262890683122, 1.000000000000000000, 0.9659258262890683122, 1.000000000000000000, 0.9659258262890683122, 1.000000000000000000, 0.9659258262890683122, 1.000000000000000000, 0.9659258262890683122, 1.000000000000000000, 0.9659258262890683122, 1.000000000000000000, 0.9659258262890683122, 1.000000000000000000, 0.9659258262890683122, 1.000000000000000000, 0.9659258262890683122, 1.000000000000000000, 0.9659258262890683122, 1.000000000000000000, 0.9659258262890683122, 1.000000000000000000, 0.9659258262890683122, 1.000000000000000000, 0.9659258262890683122, 1.000000000000000000, 0.9659258262890683122, 1.000000000000000000, 0.9659258262890683122, 1.000000000000000000, 0.9659258262890683122, 1.000000000000000000, 0.9659258262890683122, 1.000000000000000000, 0.9659258262890683122, 1.000000000000000000, 0.9659258262890683122, 1.000000000000000000, 0.9659258262890683122, 1.000000000000000000, 0.9659258262890683122, 1.000000000000000000, 0.9659258262890683122, 1.000000000000000000, 0.9659258262890683122, 1.000000000000000000, 0.9659258262890683122, 1.000000000000000000, 0.9659258262890683122, 1.000000000000000000, 0.9659258262890683122, 1.000000000000000000, 0.9659258262890683122, 1.000000000000000000, 0.9659258262890683122, 1.000000000000000000, 0.9659258262890683122, 1.000000000000000000, 0.9659258262890683122, 1.000000000000000000, 0.9659258262890683122, 1.000000000000000000, 0.9659258262890683122, 1.000000000000000000, 0.9659258262890683122, 1.000000000000000000, 0.9659258262890683122, 1.000000000000000000, 0.9659258262890683122, 1.000000000000000000, 0.9659258262890683122, 1.000000000000000000, 0.9659258262890683122, 1.000000000000000000, 0.9659258262890683122, 1.000000000000000000, 0.9659258262890683122, 1.000000000000000000, 0.9659258262890683122, 1.000000000000000000, 0.9659258262890683122, 1.000000000000000000, 0.9659258262890683122, 1.000000000000000000, 0.9659258262890683122, 1.000000000000000000, 0.9659258262890683122, 1.000000000000000000, 0.9659258262890683122, 1.000000000000000000, 0.9659258262890683122, 1.000000000000000000, 0.9659258262890683122, 1.000000000000000000, 0.9659258262890683122, 1.000000000000000000, 0.9659258262890683122, 1.000000000000000000, 0.9659258262890683122, 1.000000000000000000, 0.9659258262890683122, 1.000000000000000000, 0.9659258262890683122, 1.000000000000000000, 0.9659258262890683122, 1.000000000000000000, 0.9659258262890683122, 1.000000000000000000, 0.9659258262890683122, 1.000000000000000000, 0.9659258262890683122, 1.000000000000000000, 0.9659258262890683122, 1.000000000000000000, 0.9659258262890683122, 1.000000000000000000, 0.9659258262890683122, 1.000000000000000000, 0.9659258262890683122, 1.000000000000000000, 0.9659258262890683122, 1.000000000000000000, 0.9659258262890683122, 1.000000000000000000, 0.9659258262890683122, 1.000000000000000000, 0.9659258262890683122, 1.000000000000000000, 0.9659258262890683122, 1.000000000000000000, 0.9659258262890683122, 1.000000000000000000, 0.9659258262890683122, 1.000000000000000000, 0.9659258262890683122, 1.000000000000000000, 0.9659258262890683122, 1.000000000000000000, 0.9659258262890683122, 1.000000000000000000, 0.9659258262890683122, 1.000000000000000000, 0.9659258262890683122, 1.000000000000000000, 0.9659258262890683122, 1.000000000000000000, 0.9659258262890683122, 1.000000000000000000, 0.9659258262890683122, 1.000000000000000000, 0.9659258262890683122, 1.000000000000000000, 0.9659258262890683122, 1.000000000000000000, 0.9659258262890683122, 1.000000000000000000, 0.9659258262890683122, 1.000000000000000000, 0.9659258262890683122, 1.000000000000000000, 0.9659258262890683122, 1.000000000000000000, 0.9659258262890683122, 1.000000000000000000, 0.9659258262890683122, 1.000000000000000000, 0.9659258262890683122, 1.000000000000000000, 0.9659258262890683122, 1.000000000000000000, 0.9659258262890683122, 1.000000000000000000, 0.9659258262890683122, 1.000000000000000000, 0.9659258262890683122, 1.000000000000000000, 0.9659258262890683122, 1.000000000000000000, 0.9659258262890683122, 1.000000000000000000, 0.9659258262890683122, 1.000000000000000000, 0.9659258262890683122, 1.000000000000000000, 0.9659258262890683122, 1.000000000000000000 ) ) 
 REPRESENTATION_ITEM ( '' )  );
#12486 = CARTESIAN_POINT ( 'NONE',  ( 23.87821517812500005, -4.985214923628404016, -7.753124999385491378 ) ) ;
#12487 = CARTESIAN_POINT ( 'NONE',  ( 15.24356964374999990, 248.0593750006145228, 0.000000000000000000 ) ) ;
#12488 = CARTESIAN_POINT ( 'NONE',  ( 6.594114490232313663, 101.2601862821014436, 6.840914352312096547 ) ) ;
#12489 = AXIS2_PLACEMENT_3D ( 'NONE', #13296, #1728, #15962 ) ;
#12490 = CARTESIAN_POINT ( 'NONE',  ( 22.60769515458672885, 243.1736538117966973, -5.999999999999998224 ) ) ;
#12491 = CARTESIAN_POINT ( 'NONE',  ( 8.843639120294245259, 57.66481371789855359, 3.474262827703527901 ) ) ;
#12492 = CARTESIAN_POINT ( 'NONE',  ( 19.68408634441910721, -5.407089921784855591, -4.940624999385550886 ) ) ;
#12493 = EDGE_CURVE ( 'NONE', #1851, #2775, #14429, .T. ) ;
#12494 = CARTESIAN_POINT ( 'NONE',  ( -8.152565276336593669, 117.7523137178985735, -5.233372021372610483 ) ) ;
#12495 = CARTESIAN_POINT ( 'NONE',  ( 18.12178482187500350, 239.9218750006145058, 4.985214923628407568 ) ) ;
#12496 = CARTESIAN_POINT ( 'NONE',  ( 2.311890736173452865, 36.67731371789854933, -12.53471296425189152 ) ) ;
#12497 = DIRECTION ( 'NONE',  ( -1.000000000000000000, 0.000000000000000000, 0.000000000000000000 ) ) ;
#12498 = CARTESIAN_POINT ( 'NONE',  ( 6.932735513423970097, 73.94768628210145778, 10.69584247140445044 ) ) ;
#12499 = CARTESIAN_POINT ( 'NONE',  ( 22.56230152254411792, -3.464101615137751278, -5.549999998771003362 ) ) ;
#12500 = ADVANCED_FACE ( 'NONE', ( #32487 ), #3686, .F. ) ;
#12501 = VECTOR ( 'NONE', #32459, 1000.000000000000114 ) ;
#12502 =( BOUNDED_CURVE ( )  B_SPLINE_CURVE ( 2, ( #6079, #8934, #3428, #19637, #5204, #10896, #32049 ),
 .UNSPECIFIED., .F., .F. ) 
 B_SPLINE_CURVE_WITH_KNOTS ( ( 3, 2, 2, 3 ),
 ( 0.1086956521739117498, 0.1159420289855060821, 0.1231884057971004143, 0.1304347826086947326 ),
 .UNSPECIFIED. ) 
 CURVE ( )  GEOMETRIC_REPRESENTATION_ITEM ( )  RATIONAL_B_SPLINE_CURVE ( ( 1.000000000000023759, 0.8660254037844148378, 1.000000000000000000, 0.8660254037844387076, 1.000000000000000000, 0.8660254037844556940, 0.9999999999999830136 ) ) 
 REPRESENTATION_ITEM ( '' )  );
#12503 = CARTESIAN_POINT ( 'NONE',  ( 15.00000000000000000, 0.000000000000000000, -1.743749998770943721 ) ) ;
#12504 = CARTESIAN_POINT ( 'NONE',  ( 27.95086320365434318, -5.407089921784859143, 165.2671938279954702 ) ) ;
#12505 = CARTESIAN_POINT ( 'NONE',  ( 15.46528703574804986, 81.99768628210142651, 3.257655550457285720 ) ) ;
#12506 = CARTESIAN_POINT ( 'NONE',  ( 13.44051670066911441, -5.407089921784865361, -5.071874999385522997 ) ) ;
#12507 = FACE_OUTER_BOUND ( 'NONE', #13544, .T. ) ;
#12508 = CARTESIAN_POINT ( 'NONE',  ( 10.56230152254442700, 3.464101615137936019, -7.124999998771008869 ) ) ;
#12509 = CARTESIAN_POINT ( 'NONE',  ( 10.56230152254410903, 7.347880794884117764E-16, -10.00000000000000000 ) ) ;
#12510 = CARTESIAN_POINT ( 'NONE',  ( -9.465287035748065847, 114.1976862821014578, -2.064181346179273735 ) ) ;
#12511 = CARTESIAN_POINT ( 'NONE',  ( 1.255007937094097924E-14, 199.1000000012290627, -27.00000000000000000 ) ) ;
#12512 = CARTESIAN_POINT ( 'NONE',  ( -8.715434833791929847, 133.4601862821014606, -8.962234695871762469 ) ) ;
#12513 = CARTESIAN_POINT ( 'NONE',  ( -1.926257025242585782E-15, 195.2468750006145513, -31.45816453501075927 ) ) ;
#12514 = CARTESIAN_POINT ( 'NONE',  ( 26.75643035624999655, 249.1843750006145228, -7.049594010296217766E-16 ) ) ;
#12515 = EDGE_LOOP ( 'NONE', ( #3784, #21961, #25481, #8100 ) ) ;
#12516 = CARTESIAN_POINT ( 'NONE',  ( 28.09467017918796472, 5.407089921784856479, 166.9109150798468306 ) ) ;
#12517 = CARTESIAN_POINT ( 'NONE',  ( 23.87821517812499650, 4.985214923628404904, -2.090624999385476634 ) ) ;
#12518 = AXIS2_PLACEMENT_3D ( 'NONE', #12251, #29874, #23821 ) ;
#12519 = CARTESIAN_POINT ( 'NONE',  ( -1.926257025242585782E-15, 199.7468750006145513, -31.45816453501076637 ) ) ;
#12520 = CARTESIAN_POINT ( 'NONE',  ( 16.56230152254411436, 6.928203230275514990, -7.762500000000014388 ) ) ;
#12521 = DIRECTION ( 'NONE',  ( 0.9933043639548628789, -0.1155267958017759528, 0.000000000000000000 ) ) ;
#12522 = CARTESIAN_POINT ( 'NONE',  ( -4.694659320240884604E-14, 197.5250000012290172, 27.00000000000000000 ) ) ;
#12523 = CARTESIAN_POINT ( 'NONE',  ( -3.253724281355068545E-15, 198.9874999999999829, -27.00000000000000000 ) ) ;
#12524 = CARTESIAN_POINT ( 'NONE',  ( -9.534712964251895073, 25.17731371789854933, -1.715153634034446428 ) ) ;
#12525 = CARTESIAN_POINT ( 'NONE',  ( 13.62178482187499640, 196.5593750006145513, -23.59362340125807123 ) ) ;
#12527 = ORIENTED_EDGE ( 'NONE', *, *, #20519, .T. ) ;
#12526 = ORIENTED_EDGE ( 'NONE', *, *, #26608, .T. ) ;
#12528 = CARTESIAN_POINT ( 'NONE',  ( 26.75643035624999655, 247.7593750006145399, -3.323476615752271712 ) ) ;
#12529 = CARTESIAN_POINT ( 'NONE',  ( -12.53471296425189152, 25.17731371789855288, -2.311890736173453309 ) ) ;
#12530 = CARTESIAN_POINT ( 'NONE',  ( 23.87821517812499650, 4.985214923628404904, -2.540624999385482141 ) ) ;
#12531 = CARTESIAN_POINT ( 'NONE',  ( 8.632099005475788900, 138.4523137178985621, -13.23911966647199812 ) ) ;
#12532 = CARTESIAN_POINT ( 'NONE',  ( 26.99999999999999645, 3.464101615137755275, -8.231249998770962861 ) ) ;
#12533 = LINE ( 'NONE', #35453, #6937 ) ;
#12534 = VERTEX_POINT ( 'NONE', #18294 ) ;
#12535 = CARTESIAN_POINT ( 'NONE',  ( 16.56230152254411436, 7.209453229046482114, -5.259374999385502569 ) ) ;
#12537 = ORIENTED_EDGE ( 'NONE', *, *, #34486, .T. ) ;
#12536 = VECTOR ( 'NONE', #18296, 1000.000000000000000 ) ;
#12538 = CARTESIAN_POINT ( 'NONE',  ( 5.778771075727756162E-15, 195.8656250006145285, 31.45816453501075927 ) ) ;
#12539 = CARTESIAN_POINT ( 'NONE',  ( 2.311890736173175753, 138.9226862821014663, 12.53471296425194836 ) ) ;
#12540 = CARTESIAN_POINT ( 'NONE',  ( 37.12860184164360788, -3.604726614523238837, 162.7138348986514131 ) ) ;
#12541 = CARTESIAN_POINT ( 'NONE',  ( -52.17336230271184405, 217.4189793300686233, 4.149950860017807663 ) ) ;
#12542 = CARTESIAN_POINT ( 'NONE',  ( 23.87821517812499650, 246.8968750006145285, -4.985214923628404904 ) ) ;
#12543 = AXIS2_PLACEMENT_3D ( 'NONE', #21734, #25812, #19591 ) ;
#12544 = CARTESIAN_POINT ( 'NONE',  ( 2.999999999999997335, 244.5000000000000000, 0.000000000000000000 ) ) ;
#12545 = CARTESIAN_POINT ( 'NONE',  ( -45.44419563604516554, 205.4999999999999716, 0.1155267958017633378 ) ) ;
#12546 = CARTESIAN_POINT ( 'NONE',  ( -32.98288769728824121, 203.5309553116391612, -1.857196546604028775 ) ) ;
#12547 = CARTESIAN_POINT ( 'NONE',  ( 24.90959286293295349, 3.604726614523236616, 166.3237786275915937 ) ) ;
#12548 = EDGE_LOOP ( 'NONE', ( #29374, #6944, #27249, #898 ) ) ;
#12549 = CARTESIAN_POINT ( 'NONE',  ( -74.35000000000002274, 210.0000000000000000, 2.500000000000001332 ) ) ;
#12550 = CARTESIAN_POINT ( 'NONE',  ( -13.23911966647218463, 131.4476862821014436, 8.632099005475506459 ) ) ;
#12551 = CARTESIAN_POINT ( 'NONE',  ( -45.64955436395490551, 216.3070033484980002, -6.137860380172975638 ) ) ;
#12552 = CARTESIAN_POINT ( 'NONE',  ( -5.529263428287477744, 121.6726862821014521, 7.954856959092191815 ) ) ;
#12553 = CARTESIAN_POINT ( 'NONE',  ( 18.00000000000000355, 249.2312500012290570, 5.196152422706632912 ) ) ;
#12554 = CARTESIAN_POINT ( 'NONE',  ( 7.228626920339068285, 34.27268628210144641, -10.49813415415989581 ) ) ;
#12556 = EDGE_CURVE ( 'NONE', #33064, #27793, #31365, .T. ) ;
#12555 = CARTESIAN_POINT ( 'NONE',  ( 10.56230152254410903, 0.000000000000000000, -7.200000000000040146 ) ) ;
#12557 = VERTEX_POINT ( 'NONE', #9935 ) ;
#12558 = CARTESIAN_POINT ( 'NONE',  ( 8.927990412390657937, 117.0726862821014294, -13.04141134922759804 ) ) ;
#12559 = CARTESIAN_POINT ( 'NONE',  ( 22.56230152254410370, 0.000000000000000000, -10.00000000000000000 ) ) ;
#12560 = CARTESIAN_POINT ( 'NONE',  ( -5.233372021372612259, 143.0523137178985280, 8.152565276336593669 ) ) ;
#12561 = CARTESIAN_POINT ( 'NONE',  ( 27.24356964374999635, 197.3656250006145285, -15.72908226750539029 ) ) ;
#12562 = FACE_OUTER_BOUND ( 'NONE', #7893, .T. ) ;
#12563 = CARTESIAN_POINT ( 'NONE',  ( 27.24356964374999635, 199.2218750006145456, -15.72908226750539029 ) ) ;
#12564 = CARTESIAN_POINT ( 'NONE',  ( 21.13469769562223988, -4.064762008813216809, -9.999999999999996447 ) ) ;
#12565 = CYLINDRICAL_SURFACE ( 'NONE', #7379, 2.649999999999992806 ) ;
#12566 = DIRECTION ( 'NONE',  ( 1.000000000000000000, 0.000000000000000000, 0.000000000000000000 ) ) ;
#12567 = CARTESIAN_POINT ( 'NONE',  ( -6.840914352311947333, 72.03981371789855359, -6.594114490232462877 ) ) ;
#12568 = CARTESIAN_POINT ( 'NONE',  ( 28.04195244930222586, 5.196152422706630247, 164.9110245461011743 ) ) ;
#12569 = VERTEX_POINT ( 'NONE', #12405 ) ;
#12570 = CARTESIAN_POINT ( 'NONE',  ( 21.00000000000000000, 243.4187500012290286, 6.928203230275506996 ) ) ;
#12571 = CARTESIAN_POINT ( 'NONE',  ( 8.715434833792128799, 74.33981371789855075, -8.962234695871567070 ) ) ;
#12572 = CARTESIAN_POINT ( 'NONE',  ( 10.31873187879410558, 3.604726614523240613, -3.384374999385492355 ) ) ;
#12573 = CARTESIAN_POINT ( 'NONE',  ( -13.99999999999999467, 143.0000000000000000, -1.543483589373963192E-13 ) ) ;
#12574 = CARTESIAN_POINT ( 'NONE',  ( 23.87821517812499650, 4.985214923628404904, -4.903124999385472194 ) ) ;
#12575 = CARTESIAN_POINT ( 'NONE',  ( 11.48171059495408208, 47.31481371789855928, -4.944772684328420986 ) ) ;
#12576 = ORIENTED_EDGE ( 'NONE', *, *, #5426, .T. ) ;
#12577 = CARTESIAN_POINT ( 'NONE',  ( 20.99999999999999645, 6.646953231504538984, -7.903124999385464200 ) ) ;
#12578 = CARTESIAN_POINT ( 'NONE',  ( 15.24356964374999990, 243.4468750006145115, 0.000000000000000000 ) ) ;
#12579 = CARTESIAN_POINT ( 'NONE',  ( -12.46528703574805697, 22.19768628210145067, -2.660918448318280838 ) ) ;
#12580 = CARTESIAN_POINT ( 'NONE',  ( -43.46502896937849414, 215.5714017266979567, -3.350049139982168800 ) ) ;
#12581 = CARTESIAN_POINT ( 'NONE',  ( -61.47544563604515133, 214.8429017333602360, 4.673758765035156415 ) ) ;
#12582 = PRESENTATION_STYLE_ASSIGNMENT (( #17904 ) ) ;
#12583 = CARTESIAN_POINT ( 'NONE',  ( 36.60569886870439404, 3.464101615137755275, 159.5316748164241574 ) ) ;
#12584 = CARTESIAN_POINT ( 'NONE',  ( 11.61527771782809637, 85.26481371789856212, 4.622313124798827388 ) ) ;
#12585 = CARTESIAN_POINT ( 'NONE',  ( -45.64955436395490551, 213.3788001182225003, -3.209657149897400252 ) ) ;
#12586 = CARTESIAN_POINT ( 'NONE',  ( -69.39955436395486288, 214.8429017333601792, -4.673758765035196383 ) ) ;
#12587 = CARTESIAN_POINT ( 'NONE',  ( 18.12178482187499640, 4.985214923628404904, -7.528124999385488181 ) ) ;
#12588 = FACE_OUTER_BOUND ( 'NONE', #20621, .T. ) ;
#12589 = CARTESIAN_POINT ( 'NONE',  ( 13.04141134922778988, 56.22731371789854649, -8.927990412390371944 ) ) ;
#12590 = CARTESIAN_POINT ( 'NONE',  ( -48.41294563604517265, 216.1378603801729241, -6.307003348498026796 ) ) ;
#12591 = AXIS2_PLACEMENT_3D ( 'NONE', #20571, #11837, #17914 ) ;
#12592 = DIRECTION ( 'NONE',  ( -0.000000000000000000, -0.000000000000000000, -1.000000000000000000 ) ) ;
#12593 = CARTESIAN_POINT ( 'NONE',  ( -7.228626920339069173, 84.87268628210146915, 10.49813415415989581 ) ) ;
#12594 = CARTESIAN_POINT ( 'NONE',  ( 10.83675517735155225, 27.66018628210143859, 11.08355503943142573 ) ) ;
#12595 = CARTESIAN_POINT ( 'NONE',  ( 19.56230152254412502, 5.196152422706637353, -0.1500000000000112355 ) ) ;
#12596 = CARTESIAN_POINT ( 'NONE',  ( 27.51453976652391376, -5.407089921784865361, 160.2799941206736776 ) ) ;
#12597 = ORIENTED_EDGE ( 'NONE', *, *, #36966, .T. ) ;
#12598 = AXIS2_PLACEMENT_3D ( 'NONE', #7078, #18831, #6687 ) ;
#12599 = CARTESIAN_POINT ( 'NONE',  ( -3.257655550457281723, 56.69768628210144357, 15.46528703574804986 ) ) ;
#12600 = CARTESIAN_POINT ( 'NONE',  ( 27.24356964375000700, 196.3906250006145342, 15.72908226750537075 ) ) ;
#12601 = CARTESIAN_POINT ( 'NONE',  ( 6.500000000000000888, 244.5000000000000000, -11.00000000000000000 ) ) ;
#12602 = CARTESIAN_POINT ( 'NONE',  ( -4.500000000000001776, 227.8255434699758837, -2.500000000000000000 ) ) ;
#12603 = CARTESIAN_POINT ( 'NONE',  ( -41.29538769728821990, 211.8571965466039444, -6.469044688360768625 ) ) ;
#12604 = DIRECTION ( 'NONE',  ( -0.000000000000000000, 1.000000000000000000, -0.000000000000000000 ) ) ;
#12605 = CARTESIAN_POINT ( 'NONE',  ( 4.944772684328679446, 24.78518628210143859, -11.48171059495397373 ) ) ;
#12606 = CARTESIAN_POINT ( 'NONE',  ( -2.064181346179062349, 128.1023137178985678, -9.465287035748106703 ) ) ;
#12607 = CARTESIAN_POINT ( 'NONE',  ( 15.24356964374999990, 247.5718750006145399, -3.323476615752268604 ) ) ;
#12608 = VERTEX_POINT ( 'NONE', #21141 ) ;
#12609 = CARTESIAN_POINT ( 'NONE',  ( 26.99999999999999645, -3.464101615137751278, -7.462500000000007461 ) ) ;
#12610 = CARTESIAN_POINT ( 'NONE',  ( 24.00000000000000000, -5.196152422706629359, -4.349999999999992539 ) ) ;
#12611 = CARTESIAN_POINT ( 'NONE',  ( 4.944772684328420986, 132.4148137178985678, 11.48171059495408208 ) ) ;
#12612 = CARTESIAN_POINT ( 'NONE',  ( 22.80587116629411071, -3.604726614523235284, -5.803124999385537386 ) ) ;
#12613 = CARTESIAN_POINT ( 'NONE',  ( 37.14004103287923186, 3.604726614523238837, 162.8445854527759309 ) ) ;
#12614 = CARTESIAN_POINT ( 'NONE',  ( 0.000000000000000000, 148.0000000000000000, -24.80000000000000426 ) ) ;
#12615 = CARTESIAN_POINT ( 'NONE',  ( -27.00000000000000355, 200.0000000000000000, 0.000000000000000000 ) ) ;
#12616 = EDGE_CURVE ( 'NONE', #31449, #15078, #35522, .T. ) ;
#12617 = CARTESIAN_POINT ( 'NONE',  ( 8.715434833791931624, 46.06018628210144072, 8.962234695871760692 ) ) ;
#12618 = EDGE_LOOP ( 'NONE', ( #15709, #11497 ) ) ;
#12619 = VECTOR ( 'NONE', #16804, 1000.000000000000000 ) ;
#12620 = EDGE_LOOP ( 'NONE', ( #25163, #4640, #1879, #13089 ) ) ;
#12621 = CARTESIAN_POINT ( 'NONE',  ( 7.234628195640322446, 196.6450961906613770, 26.99999999999999645 ) ) ;
#12622 = CARTESIAN_POINT ( 'NONE',  ( 22.56230152254433818, -3.464101615137632706, -3.862500000000038014 ) ) ;
#12623 = CARTESIAN_POINT ( 'NONE',  ( 37.22995187613445012, 7.347880794884117764E-16, 166.6669193415062580 ) ) ;
#12624 = DIRECTION ( 'NONE',  ( 1.000000000000000000, 0.000000000000000000, 2.312964634635742957E-16 ) ) ;
#12625 = CARTESIAN_POINT ( 'NONE',  ( 26.75643035624999655, -3.323476615752267715, -9.403124999385470417 ) ) ;
#12626 = CARTESIAN_POINT ( 'NONE',  ( -0.1745138560725500443, 84.01018628210145778, 12.50000000000000355 ) ) ;
#12627 = CARTESIAN_POINT ( 'NONE',  ( -6.092822981423666739, 17.41481371789854649, -14.25334919248795096 ) ) ;
#12628 = FACE_BOUND ( 'NONE', #5990, .T. ) ;
#12629 = CARTESIAN_POINT ( 'NONE',  ( 15.84454946586467194, 211.9332939503076148, 5.693556627483092214 ) ) ;
#12630 = CARTESIAN_POINT ( 'NONE',  ( -62.26711230271183695, 214.4690446883608104, -1.321298161741814914 ) ) ;
#12631 = CARTESIAN_POINT ( 'NONE',  ( -50.22894823740646331, 235.3444610600932094, 5.000000000000000000 ) ) ;
#12632 = CARTESIAN_POINT ( 'NONE',  ( 31.16453849805197862, -6.928203230275506996, 166.1812066661742904 ) ) ;
#12633 = CARTESIAN_POINT ( 'NONE',  ( 8.962234695871567070, 141.0398137178985678, 8.715434833792127023 ) ) ;
#12634 = CARTESIAN_POINT ( 'NONE',  ( -51.38913769728823411, 206.8500491399821044, -5.686928522499717253 ) ) ;
#12635 = CARTESIAN_POINT ( 'NONE',  ( -30.79836230271183339, 202.5810206699313767, -4.149950860017804111 ) ) ;
#12636 = APPLICATION_PROTOCOL_DEFINITION ( 'draft international standard', 'automotive_design', 1998, #28197 ) ;
#12637 = CARTESIAN_POINT ( 'NONE',  ( 24.00000000000000000, 247.0000000000000000, 5.196152422706629359 ) ) ;
#12638 = CARTESIAN_POINT ( 'NONE',  ( 13.62178482187501416, 198.6031250006145399, 23.59362340125806767 ) ) ;
#12639 = CARTESIAN_POINT ( 'NONE',  ( -5.770363421894122880, 105.9648137178985650, 14.38691631536194393 ) ) ;
#12640 = CARTESIAN_POINT ( 'NONE',  ( -47.62127896937847993, 216.5309553116391612, 1.626142955000506873 ) ) ;
#12641 = EDGE_CURVE ( 'NONE', #26027, #15426, #16012, .T. ) ;
#12642 = EDGE_LOOP ( 'NONE', ( #17704, #14999, #30614, #8493 ) ) ;
#12643 = CARTESIAN_POINT ( 'NONE',  ( -8.962234695871760692, 29.96018628210143930, 8.715434833791933400 ) ) ;
#12644 = DIRECTION ( 'NONE',  ( -0.000000000000000000, -0.000000000000000000, 1.000000000000000000 ) ) ;
#12645 = CARTESIAN_POINT ( 'NONE',  ( -3.253724281355068545E-15, 197.6374999999999602, -27.00000000000000000 ) ) ;
#12646 = CARTESIAN_POINT ( 'NONE',  ( 37.44563085588819717, 7.646167579472024665E-16, 166.3374931129601464 ) ) ;
#12647 = CARTESIAN_POINT ( 'NONE',  ( 14.25334919248782661, 109.8851862821014720, 6.092822981423971385 ) ) ;
#12648 = FACE_OUTER_BOUND ( 'NONE', #36783, .T. ) ;
#12649 = CARTESIAN_POINT ( 'NONE',  ( 16.56230152254411081, 7.209453229046475009, -4.303124999385498306 ) ) ;
#12650 = CARTESIAN_POINT ( 'NONE',  ( 9.465287035748067623, 35.99768628210143362, 2.064181346179272847 ) ) ;
#12651 = CARTESIAN_POINT ( 'NONE',  ( 21.00000000000000000, 240.7187500012290400, 5.999999999999998224 ) ) ;
#12652 = CARTESIAN_POINT ( 'NONE',  ( -36.14955436395489841, 216.3070033484980002, -6.137860380172975638 ) ) ;
#12653 = DIRECTION ( 'NONE',  ( 0.000000000000000000, -0.000000000000000000, 1.000000000000000000 ) ) ;
#12654 = CARTESIAN_POINT ( 'NONE',  ( 11.61527771782819940, 81.13518628210145778, -4.622313124798573369 ) ) ;
#12655 = CARTESIAN_POINT ( 'NONE',  ( 15.00000000000000000, 0.000000000000000000, -4.500000000000003553 ) ) ;
#12656 = DIRECTION ( 'NONE',  ( -0.000000000000000000, 1.000000000000000000, -0.000000000000000000 ) ) ;
#12658 = ORIENTED_EDGE ( 'NONE', *, *, #14057, .F. ) ;
#12657 = CARTESIAN_POINT ( 'NONE',  ( 5.233372021372432847, 46.34768628210144925, 8.152565276336710909 ) ) ;
#12659 = CARTESIAN_POINT ( 'NONE',  ( -56.70466238434235606, 244.2363183625454894, 7.500000000000000000 ) ) ;
#12660 = CARTESIAN_POINT ( 'NONE',  ( 15.24356964374999990, 0.000000000000000000, -9.590624999385454430 ) ) ;
#12661 = CARTESIAN_POINT ( 'NONE',  ( 37.01094158893428698, -3.604726614523238837, 161.3689720562275909 ) ) ;
#12662 = CARTESIAN_POINT ( 'NONE',  ( 37.02077809343298753, -3.464101615137755275, 164.2760520648617160 ) ) ;
#12663 = CARTESIAN_POINT ( 'NONE',  ( 18.00000000000000000, 246.7750000000000057, -5.196152422706630247 ) ) ;
#12664 = CARTESIAN_POINT ( 'NONE',  ( 27.24356964374999279, 196.4656250006145797, -15.72908226750539207 ) ) ;
#12665 = CARTESIAN_POINT ( 'NONE',  ( -2.311890736173448424, 96.47731371789855359, 12.53471296425189330 ) ) ;
#12666 = CARTESIAN_POINT ( 'NONE',  ( -2.311890736173176641, 106.7226862821014635, -12.53471296425194659 ) ) ;
#12667 = EDGE_LOOP ( 'NONE', ( #7039, #30243, #19756, #29848, #16169 ) ) ;
#12668 = VERTEX_POINT ( 'NONE', #30027 ) ;
#12669 = B_SPLINE_CURVE_WITH_KNOTS ( 'NONE', 3,
 ( #5244, #12701, #36889, #16639, #32977, #30847, #25154, #30141, #13604, #15553, #9858, #15741, #31035, #19676, #2399, #7914, #2211, #31215, #16451, #13793, #22321, #1133, #25340, #22509, #5057, #8102 ),
 .UNSPECIFIED., .F., .F.,
 ( 4, 2, 2, 2, 2, 2, 2, 2, 2, 2, 2, 2, 4 ),
 ( 0.000000000000000000, 0.001454664733950383586, 0.002181997100925580149, 0.002909329467900777580, 0.004363994201851170707, 0.005091326568826366403, 0.005818658935801563833, 0.006545991302776761264, 0.007273323669751959562, 0.008727988403702353556, 0.01018265313765274842, 0.01090998550462794758, 0.01163731787160314328 ),
 .UNSPECIFIED. ) ;
#12670 = CARTESIAN_POINT ( 'NONE',  ( -27.24356964375000345, 195.3031250006145285, 0.000000000000000000 ) ) ;
#12671 = CARTESIAN_POINT ( 'NONE',  ( 10.56230152254241439, -3.464101615136776946, -9.299999998771010468 ) ) ;
#12672 = CARTESIAN_POINT ( 'NONE',  ( -8.927990412390371944, 72.32731371789854791, -13.04141134922778988 ) ) ;
#12673 = CARTESIAN_POINT ( 'NONE',  ( 26.75643035624999655, 7.049594010296217766E-16, -6.328124999385481786 ) ) ;
#12674 = CARTESIAN_POINT ( 'NONE',  ( 26.75643035624999655, 245.0968750006145456, 3.323476615752267715 ) ) ;
#12675 = CARTESIAN_POINT ( 'NONE',  ( -5.233372021372430183, 96.94768628210147199, -8.152565276336710909 ) ) ;
#12676 = CARTESIAN_POINT ( 'NONE',  ( -14.50000000000000533, 237.0000000000000000, -2.500000000000000000 ) ) ;
#12677 = CARTESIAN_POINT ( 'NONE',  ( -3.796722387233185003, 63.41481371789855359, -8.710071997420207879 ) ) ;
#12678 = CARTESIAN_POINT ( 'NONE',  ( 16.56230152254411081, 7.209453229046475009, -7.903124999385497063 ) ) ;
#12679 = CARTESIAN_POINT ( 'NONE',  ( 2.064181346179061460, 114.3023137178985422, 9.465287035748106703 ) ) ;
#12680 = PLANE ( 'NONE',  #28280 ) ;
#12681 = CARTESIAN_POINT ( 'NONE',  ( -8.962234695871565293, 35.23981371789855643, -8.715434833792128799 ) ) ;
#12682 = CARTESIAN_POINT ( 'NONE',  ( 15.00000000000000355, 7.347880794884112834E-16, -8.000000000000000000 ) ) ;
#12683 = CARTESIAN_POINT ( 'NONE',  ( 8.962234695871762469, 89.76018628210144357, -8.715434833791931624 ) ) ;
#12684 = CARTESIAN_POINT ( 'NONE',  ( 13.56230152254411614, -5.196152422706632912, -5.212499998771047416 ) ) ;
#12685 = CARTESIAN_POINT ( 'NONE',  ( 7.234628195640269155, 196.0825961894323939, 27.00000000000003197 ) ) ;
#12686 = CARTESIAN_POINT ( 'NONE',  ( 27.87242303518145548, -5.407089921784859143, 164.3706185997128841 ) ) ;
#12687 = CARTESIAN_POINT ( 'NONE',  ( 22.80587116629412847, -3.604726614523238837, -4.059374999385534366 ) ) ;
#12688 = CARTESIAN_POINT ( 'NONE',  ( 24.69711925643884598, 0.000000000000000000, 161.1005459446697614 ) ) ;
#12689 = DIRECTION ( 'NONE',  ( 1.000000000000000000, 0.000000000000000000, 2.057406622567553763E-16 ) ) ;
#12690 = CARTESIAN_POINT ( 'NONE',  ( -9.465287035748065847, 104.9976862821014549, -2.064181346179273735 ) ) ;
#12691 = DIRECTION ( 'NONE',  ( 0.9961946980917462113, 0.000000000000000000, -0.08715574274765118534 ) ) ;
#12692 = CARTESIAN_POINT ( 'NONE',  ( 10.49813415415989581, 128.5726862821014720, 7.228626920339068285 ) ) ;
#12693 = APPLICATION_CONTEXT ( 'automotive_design' ) ;
#12694 = CARTESIAN_POINT ( 'NONE',  ( -7.751135216212685641, 143.0000000000000568, 8.679851443715339343 ) ) ;
#12695 = CARTESIAN_POINT ( 'NONE',  ( 18.12178482187499640, 249.3343750006145285, -4.985214923628404904 ) ) ;
#12696 = EDGE_LOOP ( 'NONE', ( #64, #26312, #16210, #12096 ) ) ;
#12697 = CARTESIAN_POINT ( 'NONE',  ( 25.03378979634835488, -3.604726614523240613, 167.7433560723723076 ) ) ;
#12698 = CARTESIAN_POINT ( 'NONE',  ( 21.00000000000000000, -6.646953231504538984, -3.178124999385461003 ) ) ;
#12699 = DIRECTION ( 'NONE',  ( 1.000000000000000000, 0.000000000000000000, 0.000000000000000000 ) ) ;
#12701 = CARTESIAN_POINT ( 'NONE',  ( 20.48038928096284650, -5.986770049455423681, -7.999999999999998224 ) ) ;
#12700 =( BOUNDED_CURVE ( )  B_SPLINE_CURVE ( 2, ( #8183, #33951, #4391, #15971, #28074, #24862, #36410 ),
 .UNSPECIFIED., .F., .F. ) 
 B_SPLINE_CURVE_WITH_KNOTS ( ( 3, 2, 2, 3 ),
 ( 0.7608695652173907975, 0.7681159420289841444, 0.7753623188405776023, 0.7826086956521710603 ),
 .UNSPECIFIED. ) 
 CURVE ( )  GEOMETRIC_REPRESENTATION_ITEM ( )  RATIONAL_B_SPLINE_CURVE ( ( 1.000000000000010214, 0.8660254037844284936, 1.000000000000000000, 0.8660254037844387076, 1.000000000000000000, 0.8660254037844921093, 0.9999999999999465983 ) ) 
 REPRESENTATION_ITEM ( '' )  );
#12702 = DIRECTION ( 'NONE',  ( 1.000000000000000000, 0.000000000000000000, 0.000000000000000000 ) ) ;
#12703 = CARTESIAN_POINT ( 'NONE',  ( 37.11229162342512211, 7.347880794884117764E-16, 165.3220564990824073 ) ) ;
#12704 = CARTESIAN_POINT ( 'NONE',  ( 19.68408634441910721, -5.407089921784855591, -0.4406249993855471114 ) ) ;
#12705 = CARTESIAN_POINT ( 'NONE',  ( -9.500000000000005329, 15.68981371789854329, 0.1745138560723101806 ) ) ;
#12706 = CARTESIAN_POINT ( 'NONE',  ( 27.24356964375000345, 196.4843750006145626, -3.336375036156643733E-15 ) ) ;
#12707 = AXIS2_PLACEMENT_3D ( 'NONE', #2104, #22214, #2290 ) ;
#12709 = ORIENTED_EDGE ( 'NONE', *, *, #25346, .F. ) ;
#12708 = VERTEX_POINT ( 'NONE', #18108 ) ;
#12710 = CARTESIAN_POINT ( 'NONE',  ( 21.00000000000000000, 247.6093750006145342, 6.646953231504538984 ) ) ;
#12711 = CARTESIAN_POINT ( 'NONE',  ( 12.46528703574811558, 29.20231371789855501, -2.660918448318005947 ) ) ;
#12712 = ADVANCED_FACE ( 'NONE', ( #35893 ), #11924, .T. ) ;
#12713 = CARTESIAN_POINT ( 'NONE',  ( 26.75643035624999655, 7.049594010296217766E-16, -1.265624999385456251 ) ) ;
#12714 = CARTESIAN_POINT ( 'NONE',  ( 15.46528703574811736, 139.6023137178985394, -3.257655550456947768 ) ) ;
#12715 = EDGE_CURVE ( 'NONE', #20600, #29886, #6727, .T. ) ;
#12716 = CARTESIAN_POINT ( 'NONE',  ( 18.00000000000000355, -5.196152422706632912, -9.768749998770948295 ) ) ;
#12717 = CARTESIAN_POINT ( 'NONE',  ( -27.00000000000000355, 199.6250000012290400, -15.58845726811989429 ) ) ;
#12718 = ORIENTED_EDGE ( 'NONE', *, *, #20728, .T. ) ;
#12719 = CARTESIAN_POINT ( 'NONE',  ( 10.31873187879411091, 3.604726614523240613, -6.984374999385521754 ) ) ;
#12720 = EDGE_LOOP ( 'NONE', ( #3642, #6101 ) ) ;
#12721 = CARTESIAN_POINT ( 'NONE',  ( 13.62178482187499640, 196.5031250006145456, -23.59362340125807123 ) ) ;
#12722 = VECTOR ( 'NONE', #19809, 1000.000000000000000 ) ;
#12723 = CARTESIAN_POINT ( 'NONE',  ( 8.962234695871762469, 135.7601862821014720, -8.715434833791931624 ) ) ;
#12724 = CARTESIAN_POINT ( 'NONE',  ( 37.20704201011650269, -3.604726614523238837, 163.6104101269339424 ) ) ;
#12725 = ADVANCED_FACE ( 'NONE', ( #30413 ), #33067, .T. ) ;
#12726 =( BOUNDED_CURVE ( )  B_SPLINE_CURVE ( 2, ( #2343, #31160, #11060, #27935, #37200, #16757, #10497 ),
 .UNSPECIFIED., .F., .F. ) 
 B_SPLINE_CURVE_WITH_KNOTS ( ( 3, 2, 2, 3 ),
 ( 0.1739130434782606149, 0.1811594202898547112, 0.1884057971014488075, 0.1956521739130429038 ),
 .UNSPECIFIED. ) 
 CURVE ( )  GEOMETRIC_REPRESENTATION_ITEM ( )  RATIONAL_B_SPLINE_CURVE ( ( 1.000000000000004663, 0.8660254037844340447, 1.000000000000000000, 0.8660254037844387076, 1.000000000000000000, 0.8660254037844494768, 0.9999999999999892308 ) ) 
 REPRESENTATION_ITEM ( '' )  );
#12727 = CARTESIAN_POINT ( 'NONE',  ( -51.18377896937850835, 207.8379586601372750, 8.530955311639258909 ) ) ;
#12728 = CARTESIAN_POINT ( 'NONE',  ( 23.87821517812499650, 247.3468750006144887, -4.985214923628404904 ) ) ;
#12729 = PRESENTATION_STYLE_ASSIGNMENT (( #29404 ) ) ;
#12730 = LINE ( 'NONE', #24482, #7330 ) ;
#12731 = CARTESIAN_POINT ( 'NONE',  ( -46.82961230271182984, 211.3212981617417938, 4.469044688360757966 ) ) ;
#12732 = CARTESIAN_POINT ( 'NONE',  ( -10.69584247140444866, 140.6476862821014890, 6.932735513423972762 ) ) ;
#12733 = CARTESIAN_POINT ( 'NONE',  ( 34.37331128181295270, -5.407089921784855591, 167.0391835513610488 ) ) ;
#12734 = ORIENTED_EDGE ( 'NONE', *, *, #19321, .F. ) ;
#12735 = CARTESIAN_POINT ( 'NONE',  ( 26.99999999999999645, 247.9937500012290457, 3.464101615137751278 ) ) ;
#12736 = CARTESIAN_POINT ( 'NONE',  ( -15.53471296425195369, 132.0226862821014322, 2.908627838312118019 ) ) ;
#12737 = CARTESIAN_POINT ( 'NONE',  ( -50.79538769728824121, 212.3930949314662371, -8.469044688360781947 ) ) ;
#12738 = CARTESIAN_POINT ( 'NONE',  ( 7.954856959092191815, 119.3726862821014265, 5.529263428287477744 ) ) ;
#12739 = CARTESIAN_POINT ( 'NONE',  ( -47.00000000000000711, 252.0000000000000000, -2.499999999999997780 ) ) ;
#12740 = CARTESIAN_POINT ( 'NONE',  ( 11.48171059495397728, 27.08518628210144996, 4.944772684328674117 ) ) ;
#12741 = CARTESIAN_POINT ( 'NONE',  ( 19.56230152254411792, 5.196152422706637353, -7.800000000000029132 ) ) ;
#12742 = UNCERTAINTY_MEASURE_WITH_UNIT (LENGTH_MEASURE( 1.000000000000000082E-05 ), #3858, 'distance_accuracy_value', 'NONE');
#12743 = ORIENTED_EDGE ( 'NONE', *, *, #894, .T. ) ;
#12744 = CARTESIAN_POINT ( 'NONE',  ( 11.08355503943142750, 117.3601862821014663, -10.83675517735155225 ) ) ;
#12745 = CARTESIAN_POINT ( 'NONE',  ( 19.56230152254411081, -5.196152422706629359, -6.037499998771039600 ) ) ;
#12746 = CARTESIAN_POINT ( 'NONE',  ( -8.710071997420207879, 143.9148137178985678, 3.796722387233182339 ) ) ;
#12747 = CIRCLE ( 'NONE', #30907, 7.500000000000000000 ) ;
#12748 = CARTESIAN_POINT ( 'NONE',  ( 27.24356964375000345, 199.1281250006145171, -3.336375036156643733E-15 ) ) ;
#12749 = CARTESIAN_POINT ( 'NONE',  ( 18.00000000000000000, 5.196152422706630247, -1.425000000000009592 ) ) ;
#12750 = CARTESIAN_POINT ( 'NONE',  ( 13.62178482187499640, 199.2593750006145399, -23.59362340125807123 ) ) ;
#12751 = CYLINDRICAL_SURFACE ( 'NONE', #19872, 6.000000000000001776 ) ;
#12752 = PLANE ( 'NONE',  #10995 ) ;
#12753 = CARTESIAN_POINT ( 'NONE',  ( 27.83604700695378398, 5.196152422706636465, 162.5575145706350781 ) ) ;
#12754 = CARTESIAN_POINT ( 'NONE',  ( 3.474262827703532341, 82.96481371789856496, -8.843639120294245259 ) ) ;
#12755 = VERTEX_POINT ( 'NONE', #21145 ) ;
#12756 = CARTESIAN_POINT ( 'NONE',  ( 26.99999999999999645, 243.9812500012290570, -7.347880794884117764E-16 ) ) ;
#12757 = CARTESIAN_POINT ( 'NONE',  ( -4.944772684328424539, 72.61481371789855643, -11.48171059495408031 ) ) ;
#12758 = CARTESIAN_POINT ( 'NONE',  ( 13.44051670066911086, 5.407089921784862696, -3.871874999385516158 ) ) ;
#12759 = CARTESIAN_POINT ( 'NONE',  ( 13.62178482187501416, 199.5031250006145456, 23.59362340125806767 ) ) ;
#12760 = CARTESIAN_POINT ( 'NONE',  ( 21.00000000000000000, -6.646953231504538984, -4.190624999385508254 ) ) ;
#12761 = CARTESIAN_POINT ( 'NONE',  ( -4.622313124798826500, 41.56481371789855217, 11.61527771782809637 ) ) ;
#12762 = CIRCLE ( 'NONE', #19462, 2.649999999999991029 ) ;
#12763 = EDGE_LOOP ( 'NONE', ( #518, #35136, #5399, #17789 ) ) ;
#12764 = CARTESIAN_POINT ( 'NONE',  ( 3.061616997868383043E-15, 200.0000000000000000, 25.00000000000000000 ) ) ;
#12765 = CARTESIAN_POINT ( 'NONE',  ( 15.24356964374999990, 245.2093750006145285, -3.323476615752268604 ) ) ;
#12766 = CARTESIAN_POINT ( 'NONE',  ( -6.932735513423968321, 14.14768628210144463, -10.69584247140445221 ) ) ;
#12767 = CARTESIAN_POINT ( 'NONE',  ( -42.07961230271182984, 211.8571965466040581, 6.469044688360755302 ) ) ;
#12768 = CARTESIAN_POINT ( 'NONE',  ( -58.11086230271183695, 213.1499508600178387, -5.686928522499747451 ) ) ;
#12769 = DIRECTION ( 'NONE',  ( 0.000000000000000000, -0.000000000000000000, 1.000000000000000000 ) ) ;
#12770 = CARTESIAN_POINT ( 'NONE',  ( 4.622313124798831829, 82.96481371789856496, -11.61527771782809282 ) ) ;
#12771 = CARTESIAN_POINT ( 'NONE',  ( -42.48288769728823411, 205.5309553116392465, -1.321298161741839117 ) ) ;
#12772 = CARTESIAN_POINT ( 'NONE',  ( -51.58705436395488420, 205.3262412349647263, -4.842901733360204020 ) ) ;
#12773 = CARTESIAN_POINT ( 'NONE',  ( 20.99999999999999645, 6.646953231504538984, -7.115624999385463667 ) ) ;
#12774 = FACE_OUTER_BOUND ( 'NONE', #21343, .T. ) ;
#12775 = CARTESIAN_POINT ( 'NONE',  ( -2.908627838312453306, 50.47731371789854649, 15.53471296425188797 ) ) ;
#12776 = CARTESIAN_POINT ( 'NONE',  ( -48.21502896937850124, 217.3034525342667962, -4.350049139982195001 ) ) ;
#12777 = DIRECTION ( 'NONE',  ( 0.08715574274765150453, 0.000000000000000000, 0.9961946980917461003 ) ) ;
#12778 = CARTESIAN_POINT ( 'NONE',  ( 12.50000000000000355, 81.71018628210144641, 0.1745138560725507937 ) ) ;
#12779 = CARTESIAN_POINT ( 'NONE',  ( -6.092822981423970496, 20.18518628210144783, 14.25334919248782661 ) ) ;
#12780 = DIRECTION ( 'NONE',  ( -0.000000000000000000, -0.000000000000000000, 1.000000000000000000 ) ) ;
#12781 = CARTESIAN_POINT ( 'NONE',  ( 20.99999999999995381, 244.3187500012290627, 5.999999999999998224 ) ) ;
#12782 = AXIS2_PLACEMENT_3D ( 'NONE', #32821, #21095, #18634 ) ;
#12783 = VERTEX_POINT ( 'NONE', #13162 ) ;
#12784 = CARTESIAN_POINT ( 'NONE',  ( -8.632099005475501130, 41.74768628210143362, -13.23911966647218996 ) ) ;
#12785 = CARTESIAN_POINT ( 'NONE',  ( 13.62178482187501416, 198.6031250006145399, 23.59362340125806767 ) ) ;
#12786 = CARTESIAN_POINT ( 'NONE',  ( 10.56230152254527788, 3.464101615138426737, -8.474999998771037824 ) ) ;
#12787 = CYLINDRICAL_SURFACE ( 'NONE', #21325, 5.999999999999999112 ) ;
#12788 = DIRECTION ( 'NONE',  ( 0.08715574274765150453, 0.000000000000000000, 0.9961946980917461003 ) ) ;
#12789 = CARTESIAN_POINT ( 'NONE',  ( 19.56230152254410370, 5.196152422706631135, -7.687499998771024856 ) ) ;
#12790 = CARTESIAN_POINT ( 'NONE',  ( 8.715434833791931624, 27.66018628210144215, 8.962234695871760692 ) ) ;
#12791 = DIRECTION ( 'NONE',  ( 0.000000000000000000, 0.000000000000000000, 1.000000000000000000 ) ) ;
#12792 = CARTESIAN_POINT ( 'NONE',  ( -9.534712964251895073, 135.5773137178985905, -1.715153634034446428 ) ) ;
#12793 = CARTESIAN_POINT ( 'NONE',  ( 26.75643035624999655, 244.2718750006145001, -3.323476615752271268 ) ) ;
#12794 = ORIENTED_EDGE ( 'NONE', *, *, #20123, .T. ) ;
#12795 = CARTESIAN_POINT ( 'NONE',  ( -42.15435043487494227, 254.8329415120769852, 5.000000000000000000 ) ) ;
#12796 = CARTESIAN_POINT ( 'NONE',  ( -0.1745138560722763466, 137.5898137178985792, -12.50000000000000355 ) ) ;
#12797 = CARTESIAN_POINT ( 'NONE',  ( 10.31873187879411091, -3.604726614523240613, -6.853124999385484806 ) ) ;
#12798 = CARTESIAN_POINT ( 'NONE',  ( 34.15106413780644345, 5.407089921784857367, 164.4988870712271023 ) ) ;
#12799 = CARTESIAN_POINT ( 'NONE',  ( -13.50000000000000533, 198.1250000000000284, -23.38268590217984411 ) ) ;
#12800 = ORIENTED_EDGE ( 'NONE', *, *, #19147, .F. ) ;
#12801 = CARTESIAN_POINT ( 'NONE',  ( -7.228626920339070061, 57.27268628210143930, 10.49813415415989404 ) ) ;
#12802 = ORIENTED_EDGE ( 'NONE', *, *, #21001, .F. ) ;
#12803 = ORIENTED_EDGE ( 'NONE', *, *, #1726, .T. ) ;
#12804 = CARTESIAN_POINT ( 'NONE',  ( 27.57131143846490673, 5.196152422706630247, 159.5315731764057716 ) ) ;
#12805 = CARTESIAN_POINT ( 'NONE',  ( 15.24356964374999990, 3.323476615752268604, -1.078124999385470462 ) ) ;
#12806 = CARTESIAN_POINT ( 'NONE',  ( -26.99999999999999645, 199.2500000012290116, 15.58845726811991561 ) ) ;
#12807 = CARTESIAN_POINT ( 'NONE',  ( 24.77555942491173369, 0.000000000000000000, 161.9971211729523475 ) ) ;
#12808 = CARTESIAN_POINT ( 'NONE',  ( 26.75643035624999655, 3.323476615752271712, -9.778124999385472194 ) ) ;
#12809 = AXIS2_PLACEMENT_3D ( 'NONE', #423, #5922, #23561 ) ;
#12810 = CARTESIAN_POINT ( 'NONE',  ( 11.48171059495397728, 82.28518628210146346, 4.944772684328674117 ) ) ;
#12811 = CARTESIAN_POINT ( 'NONE',  ( 3.257655550456945548, 13.10231371789855181, 15.46528703574811736 ) ) ;
#12812 = CARTESIAN_POINT ( 'NONE',  ( -27.00000000000000355, 197.2624999999999886, -15.58845726811989429 ) ) ;
#12813 = CARTESIAN_POINT ( 'NONE',  ( 16.56230152254411436, 6.928203230275506996, -4.949999998771019705 ) ) ;
#12814 = CARTESIAN_POINT ( 'NONE',  ( -50.39211230271182984, 205.5309553116392465, 1.321298161741817356 ) ) ;
#12815 = CARTESIAN_POINT ( 'NONE',  ( 0.000000000000000000, 200.0000000000000000, 0.000000000000000000 ) ) ;
#12816 = CARTESIAN_POINT ( 'NONE',  ( 37.27244030072392889, 3.464101615137755275, 167.1525642568259968 ) ) ;
#12817 = CARTESIAN_POINT ( 'NONE',  ( -8.152565276336593669, 7.352313717898546486, -5.233372021372610483 ) ) ;
#12818 = CARTESIAN_POINT ( 'NONE',  ( -44.46205436395488420, 214.6737587650352168, 4.842901733360204908 ) ) ;
#12819 = CARTESIAN_POINT ( 'NONE',  ( -68.40997103062156270, 217.3034525342668815, 4.350049139982096413 ) ) ;
#12820 = ITEM_DEFINED_TRANSFORMATION ( 'NONE', 'NONE', #17811,  #17215 ) ;
#12821 = CYLINDRICAL_SURFACE ( 'NONE', #31848, 2.649999999999999467 ) ;
#12822 = CARTESIAN_POINT ( 'NONE',  ( -13.62178482187500528, 199.2781250006145228, -23.59362340125807123 ) ) ;
#12823 = CARTESIAN_POINT ( 'NONE',  ( -10.83675517735179028, 106.5398137178985536, 11.08355503943118947 ) ) ;
#12824 = CARTESIAN_POINT ( 'NONE',  ( -46.03794563604517265, 205.3262412349647832, 4.842901733360250205 ) ) ;
#12825 = ORIENTED_EDGE ( 'NONE', *, *, #4077, .F. ) ;
#12826 = CARTESIAN_POINT ( 'NONE',  ( -10.49813415415989581, 22.77268628210143575, -7.228626920339068285 ) ) ;
#12827 = CARTESIAN_POINT ( 'NONE',  ( -7.234628195640354420, 196.1549038117966859, 26.99999999999996803 ) ) ;
#12828 = EDGE_CURVE ( 'NONE', #17773, #34698, #27145, .T. ) ;
#12829 = CARTESIAN_POINT ( 'NONE',  ( 37.41624727615045742, 7.347880794884125653E-16, 168.7962855074530069 ) ) ;
#12830 = CARTESIAN_POINT ( 'NONE',  ( 31.33367511126808935, -7.209453229046482114, 168.1144470015464378 ) ) ;
#12831 = CARTESIAN_POINT ( 'NONE',  ( 11.08355503943142750, 108.1601862821014635, -10.83675517735155225 ) ) ;
#12832 = AXIS2_PLACEMENT_3D ( 'NONE', #22915, #17038, #20256 ) ;
#12833 = CARTESIAN_POINT ( 'NONE',  ( -52.77455436395490551, 205.1570982666397640, 4.673758765035199048 ) ) ;
#12834 = CARTESIAN_POINT ( 'NONE',  ( 22.80587116629411071, -3.604726614523235284, -4.453124999385550176 ) ) ;
#12835 = CARTESIAN_POINT ( 'NONE',  ( 9.500000000000005329, 35.71018628210144641, 0.1745138560725188748 ) ) ;
#12836 = DIRECTION ( 'NONE',  ( 0.000000000000000000, 0.000000000000000000, 1.000000000000000000 ) ) ;
#12837 = CARTESIAN_POINT ( 'NONE',  ( -42.68080436395489841, 201.5000000000000000, -0.1155267958017054536 ) ) ;
#12838 = CARTESIAN_POINT ( 'NONE',  ( 0.000000000000000000, 202.0000000000000000, 0.000000000000000000 ) ) ;
#12839 = EDGE_CURVE ( 'NONE', #11530, #23355, #1711, .T. ) ;
#12840 = CARTESIAN_POINT ( 'NONE',  ( 0.1745138560725515708, 79.41018628210144925, -12.50000000000000355 ) ) ;
#12841 = DIRECTION ( 'NONE',  ( -1.000000000000000000, 0.000000000000000000, -0.000000000000000000 ) ) ;
#12843 = ORIENTED_EDGE ( 'NONE', *, *, #37247, .F. ) ;
#12842 = CARTESIAN_POINT ( 'NONE',  ( 8.843639120294328748, 53.53518628210145636, -3.474262827703334722 ) ) ;
#12844 = DIRECTION ( 'NONE',  ( 0.08715574274765150453, 0.000000000000000000, 0.9961946980917461003 ) ) ;
#12845 = VERTEX_POINT ( 'NONE', #15450 ) ;
#12846 = CARTESIAN_POINT ( 'NONE',  ( 15.24356964374999990, 0.000000000000000000, -9.140624999385476457 ) ) ;
#12847 = CARTESIAN_POINT ( 'NONE',  ( -7.234628195640263826, 195.5200961906613770, -27.00000000000003553 ) ) ;
#12848 = CARTESIAN_POINT ( 'NONE',  ( 33.93698784468253393, -5.407089921784861808, 162.0519838440392562 ) ) ;
#12849 = CARTESIAN_POINT ( 'NONE',  ( 33.80667851479820030, 5.196152422706637353, 161.9598655117922874 ) ) ;
#12850 = CARTESIAN_POINT ( 'NONE',  ( 21.00000000000000000, 245.3875000000000455, -6.928203230275506996 ) ) ;
#12851 = CARTESIAN_POINT ( 'NONE',  ( 27.24356964375000345, 195.0781250006145342, -3.336375036156643733E-15 ) ) ;
#12852 = EDGE_CURVE ( 'NONE', #29586, #21112, #25219, .T. ) ;
#12853 = CARTESIAN_POINT ( 'NONE',  ( -10.49813415416004858, 79.22731371789855359, 7.228626920338839135 ) ) ;
#12854 = CARTESIAN_POINT ( 'NONE',  ( 7.228626920339069173, 98.67268628210146630, -10.49813415415989404 ) ) ;
#12855 = VERTEX_POINT ( 'NONE', #15824 ) ;
#12856 = ORIENTED_EDGE ( 'NONE', *, *, #3607, .T. ) ;
#12857 = CARTESIAN_POINT ( 'NONE',  ( -13.50000000000000533, 197.7875000012290627, -23.38268590217984411 ) ) ;
#12858 = CARTESIAN_POINT ( 'NONE',  ( 21.00000000000000000, 240.8593750006145342, 6.646953231504538984 ) ) ;
#12859 = EDGE_CURVE ( 'NONE', #19808, #11398, #10808, .T. ) ;
#12860 = CARTESIAN_POINT ( 'NONE',  ( 14.38691631536194393, 66.86481371789854222, 5.770363421894124656 ) ) ;
#12861 = CARTESIAN_POINT ( 'NONE',  ( 26.75643035624999655, 3.323476615752271712, -5.840624999385470417 ) ) ;
#12862 = EDGE_CURVE ( 'NONE', #5775, #5529, #3691, .T. ) ;
#12863 = CARTESIAN_POINT ( 'NONE',  ( 15.24356964375000167, 244.0468750006145342, 3.323476615752272600 ) ) ;
#12864 = CARTESIAN_POINT ( 'NONE',  ( 1.715153634034233487, 92.92268628210145209, 9.534712964251941258 ) ) ;
#12865 = CARTESIAN_POINT ( 'NONE',  ( 26.99999999999999645, 243.1187500012290172, -3.464101615137755275 ) ) ;
#12866 = CARTESIAN_POINT ( 'NONE',  ( -3.474262827703527901, 50.76481371789856212, 8.843639120294245259 ) ) ;
#12867 = CARTESIAN_POINT ( 'NONE',  ( 16.56230152254411081, 7.209453229046475009, -8.803124999385518734 ) ) ;
#12868 = CARTESIAN_POINT ( 'NONE',  ( -8.710071997420207879, 116.3148137178985735, 3.796722387233182339 ) ) ;
#12869 = CARTESIAN_POINT ( 'NONE',  ( 7.234628195640337545, 198.0674038105676971, -26.99999999999999289 ) ) ;
#12870 = CARTESIAN_POINT ( 'NONE',  ( 12.50000000000000355, 38.68981371789855217, -0.1745138560722771515 ) ) ;
#12871 = CARTESIAN_POINT ( 'NONE',  ( -0.1745138560725500443, 84.01018628210145778, 12.50000000000000355 ) ) ;
#12872 = CARTESIAN_POINT ( 'NONE',  ( 10.56230152254410548, 3.464101615137752166, -8.024999998771027876 ) ) ;
#12873 = CARTESIAN_POINT ( 'NONE',  ( 22.56230152254411792, 7.347880794884125653E-16, -1.125000000000042633 ) ) ;
#12874 = CARTESIAN_POINT ( 'NONE',  ( 27.79398286670857132, -5.407089921784859143, 163.4740433714303265 ) ) ;
#12875 = CARTESIAN_POINT ( 'NONE',  ( 19.68408634441910721, 5.407089921784862696, -4.396874999385541827 ) ) ;
#12876 = FILL_AREA_STYLE ('',( #21984 ) ) ;
#12877 = FACE_OUTER_BOUND ( 'NONE', #4109, .T. ) ;
#12878 = EDGE_CURVE ( 'NONE', #19498, #14298, #1029, .T. ) ;
#12879 = CARTESIAN_POINT ( 'NONE',  ( 31.35083389806797527, -6.928203230275514990, 168.3105728321210393 ) ) ;
#12880 = CARTESIAN_POINT ( 'NONE',  ( -2.064181346179269738, 93.49768628210142651, 9.465287035748067623 ) ) ;
#12881 = CARTESIAN_POINT ( 'NONE',  ( 0.000000000000000000, 202.0000000000000000, 0.000000000000000000 ) ) ;
#12882 = EDGE_CURVE ( 'NONE', #23999, #21775, #27374, .T. ) ;
#12883 = CARTESIAN_POINT ( 'NONE',  ( 12.53471296425194836, 127.4226862821014663, -2.311890736173178418 ) ) ;
#12884 = DIRECTION ( 'NONE',  ( 1.000000000000000000, 0.000000000000000000, 0.000000000000000000 ) ) ;
#12885 = CARTESIAN_POINT ( 'NONE',  ( 18.12178482187499640, 249.7843750006145456, -4.985214923628404904 ) ) ;
#12886 = ORIENTED_EDGE ( 'NONE', *, *, #33509, .T. ) ;
#12887 = CARTESIAN_POINT ( 'NONE',  ( 37.48975345065418452, 7.646167579472015790E-16, 166.8418166788690655 ) ) ;
#12888 = CARTESIAN_POINT ( 'NONE',  ( 15.24356964375000167, -3.323476615752272600, -3.703124999385450700 ) ) ;
#12890 = EDGE_CURVE ( 'NONE', #36429, #8730, #4066, .T. ) ;
#12889 = CARTESIAN_POINT ( 'NONE',  ( 13.56230152254411614, -5.196152422706632912, -5.212499998771047416 ) ) ;
#12891 = CARTESIAN_POINT ( 'NONE',  ( 20.00041297495057080, 239.8598985277379256, -5.668978411116884608 ) ) ;
#12892 = CARTESIAN_POINT ( 'NONE',  ( 28.39820154767614468, -5.196152422706638241, 168.9829703733268218 ) ) ;
#12893 = CARTESIAN_POINT ( 'NONE',  ( 25.13834520420595098, 0.000000000000000000, 166.1437816049835874 ) ) ;
#12894 = CARTESIAN_POINT ( 'NONE',  ( 21.00000000000000000, 242.0968750006145456, -6.646953231504538984 ) ) ;
#12895 = AXIS2_PLACEMENT_3D ( 'NONE', #30508, #16104, #24441 ) ;
#12896 = CARTESIAN_POINT ( 'NONE',  ( 13.44051670066911264, -5.407089921784859143, -3.215624999385519267 ) ) ;
#12897 = CARTESIAN_POINT ( 'NONE',  ( 0.1745138560723095977, 13.38981371789854613, 9.500000000000005329 ) ) ;
#12898 = CARTESIAN_POINT ( 'NONE',  ( 27.24356964375000345, 198.2843750006145456, -3.336375036156643733E-15 ) ) ;
#12899 = B_SPLINE_CURVE_WITH_KNOTS ( 'NONE', 3,
 ( #10792, #25004, #7582, #18454, #19159, #7770, #16303, #30708, #6688, #29996, #35674, #3836, #1178, #29802, #15599, #21108, #27155, #32834, #4727, #22365, #25198, #27850, #12371, #15414, #18073, #13645 ),
 .UNSPECIFIED., .F., .F.,
 ( 4, 2, 2, 2, 2, 2, 2, 2, 2, 2, 2, 2, 4 ),
 ( 0.000000000000000000, 0.001456441005936622663, 0.002184661508904929550, 0.002912882011873236653, 0.004369323017809840018, 0.005097543520778138014, 0.005825764023746436877, 0.007282205029683033737, 0.008010425532651330865, 0.008738646035619629729, 0.01019508704155622919, 0.01092330754452452632, 0.01165152804749282692 ),
 .UNSPECIFIED. ) ;
#12901 = ORIENTED_EDGE ( 'NONE', *, *, #10394, .T. ) ;
#12900 = ORIENTED_EDGE ( 'NONE', *, *, #30304, .F. ) ;
#12902 = CARTESIAN_POINT ( 'NONE',  ( 18.12178482187499640, 247.8718750006145228, -4.985214923628404904 ) ) ;
#12903 = EDGE_CURVE ( 'NONE', #17773, #30563, #24537, .T. ) ;
#12904 = CARTESIAN_POINT ( 'NONE',  ( -10.69584247140429412, 25.75231371789854506, -6.932735513424201024 ) ) ;
#12905 = CARTESIAN_POINT ( 'NONE',  ( 18.12178482187500350, -4.985214923628407568, -1.865624999385473437 ) ) ;
#12906 = CARTESIAN_POINT ( 'NONE',  ( -15.46528703574811736, 125.8023137178985706, 3.257655550456946436 ) ) ;
#12907 = CARTESIAN_POINT ( 'NONE',  ( 26.75643035624999655, -3.323476615752267715, -0.5156249993854836733 ) ) ;
#12908 = VERTEX_POINT ( 'NONE', #24165 ) ;
#12909 = CARTESIAN_POINT ( 'NONE',  ( 16.56230152254411436, -7.209453229046482114, -5.934374999385512162 ) ) ;
#12910 = MECHANICAL_DESIGN_GEOMETRIC_PRESENTATION_REPRESENTATION (  '', ( #33498 ), #18381 ) ;
#12911 = ORIENTED_EDGE ( 'NONE', *, *, #26308, .T. ) ;
#12912 = CARTESIAN_POINT ( 'NONE',  ( -27.24356964374999990, 196.6156250006145285, -15.72908226750537786 ) ) ;
#12913 = CARTESIAN_POINT ( 'NONE',  ( -4.944772684328673229, 130.5851862821014606, 11.48171059495397728 ) ) ;
#12914 = VECTOR ( 'NONE', #35943, 1000.000000000000000 ) ;
#12915 = CARTESIAN_POINT ( 'NONE',  ( 24.75107835581066240, 0.000000000000000000, 164.5119495204372413 ) ) ;
#12916 = CARTESIAN_POINT ( 'NONE',  ( -56.72544563604517265, 216.3070033484980854, 6.137860380172893926 ) ) ;
#12917 = CARTESIAN_POINT ( 'NONE',  ( 18.12178482187499640, 246.5218750006145001, -4.985214923628404904 ) ) ;
#12918 = DIRECTION ( 'NONE',  ( 1.000000000000000000, 0.000000000000000000, 0.000000000000000000 ) ) ;
#12919 = LINE ( 'NONE', #13105, #30324 ) ;
#12920 = CARTESIAN_POINT ( 'NONE',  ( -44.05877896937850124, 211.0902445701383101, -4.530955311639234040 ) ) ;
#12921 = CARTESIAN_POINT ( 'NONE',  ( 7.228626920339068285, 135.4726862821014493, -10.49813415415989581 ) ) ;
#12922 = CARTESIAN_POINT ( 'NONE',  ( 24.99130137175887612, 0.000000000000000000, 167.2577111570525972 ) ) ;
#12923 = ORIENTED_EDGE ( 'NONE', *, *, #12903, .T. ) ;
#12924 = CARTESIAN_POINT ( 'NONE',  ( 0.000000000000000000, 200.0000000000000000, 0.000000000000000000 ) ) ;
#12925 = CARTESIAN_POINT ( 'NONE',  ( 8.632099005475504683, 138.3476862821014208, 13.23911966647218996 ) ) ;
#12926 = CARTESIAN_POINT ( 'NONE',  ( -50.99330436395489841, 210.1155267958016850, -8.500000000000003553 ) ) ;
#12927 = CARTESIAN_POINT ( 'NONE',  ( -3.474262827703337830, 115.6351862821014436, -8.843639120294326972 ) ) ;
#12928 = EDGE_CURVE ( 'NONE', #15078, #13979, #5832, .T. ) ;
#12929 =( BOUNDED_CURVE ( )  B_SPLINE_CURVE ( 2, ( #33791, #7830, #8202, #27912, #7456, #22611, #30766 ),
 .UNSPECIFIED., .F., .F. ) 
 B_SPLINE_CURVE_WITH_KNOTS ( ( 3, 2, 2, 3 ),
 ( 0.8695652173913078764, 0.8768115942029022225, 0.8840579710144965686, 0.8913043478260908037 ),
 .UNSPECIFIED. ) 
 CURVE ( )  GEOMETRIC_REPRESENTATION_ITEM ( )  RATIONAL_B_SPLINE_CURVE ( ( 0.9999999999999342748, 0.8660254037845044328, 1.000000000000000000, 0.8660254037844387076, 1.000000000000000000, 0.8660254037843668762, 1.000000000000071942 ) ) 
 REPRESENTATION_ITEM ( '' )  );
#12930 = PLANE ( 'NONE',  #26627 ) ;
#12931 = CARTESIAN_POINT ( 'NONE',  ( -0.1745138560725500443, 10.41018628210144215, 12.50000000000000355 ) ) ;
#12932 = CARTESIAN_POINT ( 'NONE',  ( 13.56230152254411614, -5.196152422706638241, -8.025000000000058975 ) ) ;
#12933 = ORIENTED_EDGE ( 'NONE', *, *, #6157, .F. ) ;
#12934 = CARTESIAN_POINT ( 'NONE',  ( -32.38913769728823411, 206.8500491399821044, -5.686928522499717253 ) ) ;
#12935 = CARTESIAN_POINT ( 'NONE',  ( -14.38691631536207183, 113.3351862821014606, 5.770363421893814682 ) ) ;
#12936 = CARTESIAN_POINT ( 'NONE',  ( 0.000000000000000000, 141.0000000000000000, 0.000000000000000000 ) ) ;
#12937 = CARTESIAN_POINT ( 'NONE',  ( -9.465287035748106703, 144.2023137178985905, 2.064181346179061460 ) ) ;
#12938 = CARTESIAN_POINT ( 'NONE',  ( -1.926257025242585782E-15, 198.3406250006145228, -31.45816453501075927 ) ) ;
#12939 = DIRECTION ( 'NONE',  ( 0.000000000000000000, 0.000000000000000000, 1.000000000000000000 ) ) ;
#12940 = CARTESIAN_POINT ( 'NONE',  ( -13.50000000000000533, 196.3249999999999886, -23.38268590217984411 ) ) ;
#12941 = DIRECTION ( 'NONE',  ( 0.08715574274765150453, 0.000000000000000000, 0.9961946980917461003 ) ) ;
#12942 = CIRCLE ( 'NONE', #37138, 1.499999999999990452 ) ;
#12943 = LINE ( 'NONE', #24504, #15127 ) ;
#12944 = CARTESIAN_POINT ( 'NONE',  ( 3.474262827703532341, 73.76481371789856212, -8.843639120294245259 ) ) ;
#12945 = EDGE_LOOP ( 'NONE', ( #10892, #34753, #5014, #10146 ) ) ;
#12946 = CARTESIAN_POINT ( 'NONE',  ( 18.00000000000000355, 244.2812500012290400, 5.196152422706632912 ) ) ;
#12947 = CARTESIAN_POINT ( 'NONE',  ( -12.53471296425189152, 89.57731371789856212, -2.311890736173453309 ) ) ;
#12948 = CARTESIAN_POINT ( 'NONE',  ( 19.68408634441911786, -5.407089921784861808, -4.096874999385518912 ) ) ;
#12949 = CARTESIAN_POINT ( 'NONE',  ( -6.769757451167472517, 143.0000000000000568, 10.84521838874742627 ) ) ;
#12950 = CARTESIAN_POINT ( 'NONE',  ( 26.75643035624999655, -3.323476615752267715, -4.115624999385481431 ) ) ;
#12951 = CARTESIAN_POINT ( 'NONE',  ( 0.1745138560722779009, 50.18981371789854506, 12.50000000000000355 ) ) ;
#12952 =( BOUNDED_CURVE ( )  B_SPLINE_CURVE ( 2, ( #18980, #1708, #30721, #27864, #28034, #34282, #10785 ),
 .UNSPECIFIED., .F., .F. ) 
 B_SPLINE_CURVE_WITH_KNOTS ( ( 3, 2, 2, 3 ),
 ( 0.02173913043478281973, 0.02898550724637714848, 0.03623188405797147377, 0.04347826086956579905 ),
 .UNSPECIFIED. ) 
 CURVE ( )  GEOMETRIC_REPRESENTATION_ITEM ( )  RATIONAL_B_SPLINE_CURVE ( ( 0.9999999999999961142, 0.8660254037844425934, 1.000000000000000000, 0.8660254037844387076, 1.000000000000000000, 0.8660254037844279384, 1.000000000000010658 ) ) 
 REPRESENTATION_ITEM ( '' )  );
#12953 = ORIENTED_EDGE ( 'NONE', *, *, #8031, .T. ) ;
#12954 = CARTESIAN_POINT ( 'NONE',  ( 18.12178482187499640, 4.985214923628404904, -7.865624999385478766 ) ) ;
#12955 = CARTESIAN_POINT ( 'NONE',  ( 26.75643035624999655, 244.9843750006145058, 3.323476615752267715 ) ) ;
#12956 = CARTESIAN_POINT ( 'NONE',  ( -0.1745138560725500443, 19.61018628210144144, 12.50000000000000355 ) ) ;
#12957 = CARTESIAN_POINT ( 'NONE',  ( -37.52752896937850124, 213.3500491399821613, 5.571401726697954970 ) ) ;
#12958 = CARTESIAN_POINT ( 'NONE',  ( -61.07961230271182274, 211.8571965466040297, 6.469044688360755302 ) ) ;
#12959 = AXIS2_PLACEMENT_3D ( 'NONE', #1413, #9396, #659 ) ;
#12960 = AXIS2_PLACEMENT_3D ( 'NONE', #23081, #15105, #23448 ) ;
#12961 = CARTESIAN_POINT ( 'NONE',  ( 36.60243052835136268, 7.347880794884117764E-16, 159.4943175152456831 ) ) ;
#12962 = CARTESIAN_POINT ( 'NONE',  ( 2.660918448318002838, 77.50231371789855928, 12.46528703574811558 ) ) ;
#12963 = CARTESIAN_POINT ( 'NONE',  ( -40.89955436395489841, 213.3788001182225003, -3.209657149897400252 ) ) ;
#12964 = ADVANCED_FACE ( 'NONE', ( #29655 ), #30310, .F. ) ;
#12965 = CARTESIAN_POINT ( 'NONE',  ( -61.68080436395489841, 203.5000000000000000, -0.1155267958017335561 ) ) ;
#12966 = DIRECTION ( 'NONE',  ( 1.000000000000000000, 0.000000000000000000, 0.000000000000000000 ) ) ;
#12967 = CARTESIAN_POINT ( 'NONE',  ( 20.99999999999999645, 0.000000000000000000, -8.000000000000000000 ) ) ;
#12968 = CARTESIAN_POINT ( 'NONE',  ( -13.23911966647199812, 62.55231371789854222, -8.632099005475788900 ) ) ;
#12969 = EDGE_CURVE ( 'NONE', #33229, #37335, #13608, .T. ) ;
#12970 = CARTESIAN_POINT ( 'NONE',  ( -43.66294563604516554, 216.1378603801729241, -6.307003348498026796 ) ) ;
#12971 = CARTESIAN_POINT ( 'NONE',  ( 26.99999999999999645, 7.347880794884117764E-16, -3.768749998770942966 ) ) ;
#12972 = CARTESIAN_POINT ( 'NONE',  ( -12.53471296425194836, 76.82268628210145778, 2.311890736173176641 ) ) ;
#12973 = EDGE_CURVE ( 'NONE', #483, #20369, #8549, .T. ) ;
#12974 = CARTESIAN_POINT ( 'NONE',  ( 15.46528703574804986, 26.79768628210144144, 3.257655550457285720 ) ) ;
#12975 = CARTESIAN_POINT ( 'NONE',  ( 15.02283181144952628, 7.347880794884122694E-16, 50.52293445648592751 ) ) ;
#12976 = DIRECTION ( 'NONE',  ( 0.000000000000000000, 1.000000000000000000, 0.000000000000000000 ) ) ;
#12977 = ORIENTED_EDGE ( 'NONE', *, *, #10396, .T. ) ;
#12978 = CARTESIAN_POINT ( 'NONE',  ( 2.908627838312118019, 46.92268628210143788, 15.53471296425195369 ) ) ;
#12979 = CARTESIAN_POINT ( 'NONE',  ( -13.62178482187500528, 197.0281250006145228, -23.59362340125807123 ) ) ;
#12980 = CARTESIAN_POINT ( 'NONE',  ( 0.000000000000000000, 210.0000000000000284, -27.00000000000000000 ) ) ;
#12981 = CARTESIAN_POINT ( 'NONE',  ( 25.13180852339300486, -3.464101615137899159, 166.0690670014023738 ) ) ;
#12982 = CARTESIAN_POINT ( 'NONE',  ( -42.87872103062156981, 203.4690446883607535, 1.626142955000567936 ) ) ;
#12983 = CYLINDRICAL_SURFACE ( 'NONE', #13585, 7.500000000000000000 ) ;
#12984 = CARTESIAN_POINT ( 'NONE',  ( -6.932735513423968321, 23.34768628210144570, -10.69584247140445221 ) ) ;
#12985 = DIRECTION ( 'NONE',  ( -0.000000000000000000, 1.000000000000000000, -0.000000000000000000 ) ) ;
#12986 = CARTESIAN_POINT ( 'NONE',  ( -8.843639120294245259, 135.8648137178985849, -3.474262827703533230 ) ) ;
#12987 = CARTESIAN_POINT ( 'NONE',  ( 18.12178482187500350, 244.9843750006145342, 4.985214923628407568 ) ) ;
#12988 = AXIS2_PLACEMENT_3D ( 'NONE', #17736, #3316, #14887 ) ;
#12989 = ORIENTED_EDGE ( 'NONE', *, *, #20849, .F. ) ;
#12990 =( BOUNDED_CURVE ( )  B_SPLINE_CURVE ( 2, ( #3130, #26247, #6542, #18115, #29657, #3693, #15261, #8639, #17366 ),
 .UNSPECIFIED., .F., .F. ) 
 B_SPLINE_CURVE_WITH_KNOTS ( ( 3, 2, 2, 2, 3 ),
 ( 0.7708333333333333703, 0.7777777777777777901, 0.7916666666666666297, 0.8055555555555555802, 0.8125000000000000000 ),
 .UNSPECIFIED. ) 
 CURVE ( )  GEOMETRIC_REPRESENTATION_ITEM ( )  RATIONAL_B_SPLINE_CURVE ( ( 0.9330127018922192983, 0.9330127018922198534, 1.000000000000000000, 0.8660254037844387076, 1.000000000000000000, 0.8660254037844387076, 1.000000000000000000, 0.9330127018922194093, 0.9330127018922194093 ) ) 
 REPRESENTATION_ITEM ( '' )  );
#12991 = LINE ( 'NONE', #1223, #12355 ) ;
#12992 = CARTESIAN_POINT ( 'NONE',  ( -8.962234695871565293, 136.4398137178985735, -8.715434833792128799 ) ) ;
#12993 = CARTESIAN_POINT ( 'NONE',  ( 19.68408634441910721, 5.407089921784857367, -7.940624999385553551 ) ) ;
#12994 = CARTESIAN_POINT ( 'NONE',  ( 37.25443294523552851, 7.646167579472015790E-16, 164.1520909940213642 ) ) ;
#12995 = CARTESIAN_POINT ( 'NONE',  ( 37.38029553226678559, 3.464101615137904933, 168.3853551944901596 ) ) ;
#12996 = CARTESIAN_POINT ( 'NONE',  ( 13.50000000000001421, 197.9000000000000341, 23.38268590217984055 ) ) ;
#12997 = VERTEX_POINT ( 'NONE', #7 ) ;
#12998 = CARTESIAN_POINT ( 'NONE',  ( -8.962234695871760692, 39.16018628210144215, 8.715434833791933400 ) ) ;
#12999 = VERTEX_POINT ( 'NONE', #26161 ) ;
#13000 = ORIENTED_EDGE ( 'NONE', *, *, #25210, .F. ) ;
#13001 = DIRECTION ( 'NONE',  ( 0.000000000000000000, 0.000000000000000000, 1.000000000000000000 ) ) ;
#13002 = CARTESIAN_POINT ( 'NONE',  ( 23.87821517812499650, 4.985214923628404904, -0.2906249993854803648 ) ) ;
#13003 = CARTESIAN_POINT ( 'NONE',  ( 1.069080835302379631E-14, 199.3250000012290286, 27.00000000000000000 ) ) ;
#13004 = CARTESIAN_POINT ( 'NONE',  ( 30.79194769780577445, 6.928203230275506996, 161.9224743318320634 ) ) ;
#13005 = CARTESIAN_POINT ( 'NONE',  ( 21.00000000000000000, -6.646953231504538984, -9.928124999385461891 ) ) ;
#13006 = CARTESIAN_POINT ( 'NONE',  ( -10.69584247140444866, 76.24768628210144072, 6.932735513423972762 ) ) ;
#13007 = CARTESIAN_POINT ( 'NONE',  ( -14.25334919248782306, 132.8851862821014436, -6.092822981423979378 ) ) ;
#13008 = DIRECTION ( 'NONE',  ( 0.000000000000000000, 0.000000000000000000, 1.000000000000000000 ) ) ;
#13009 = CARTESIAN_POINT ( 'NONE',  ( 19.56230152254411081, 5.196152422706631135, -4.987499998771016685 ) ) ;
#13010 = CARTESIAN_POINT ( 'NONE',  ( -56.32961230271183695, 211.3212981617417938, 4.469044688360757966 ) ) ;
#13011 = CARTESIAN_POINT ( 'NONE',  ( 25.41615413421412129, -3.464101615137772594, 169.3191522051510276 ) ) ;
#13012 = CARTESIAN_POINT ( 'NONE',  ( 25.33117728503513177, 3.464101615137752166, 168.3478623745115499 ) ) ;
#13013 = CARTESIAN_POINT ( 'NONE',  ( 9.500000000000005329, 11.08981371789854897, -0.1745138560723090149 ) ) ;
#13014 = CARTESIAN_POINT ( 'NONE',  ( -51.58705436395488420, 205.3262412349647263, -4.842901733360204020 ) ) ;
#13015 = CARTESIAN_POINT ( 'NONE',  ( -52.77455436395490551, 203.6929966515020283, 6.137860380172978303 ) ) ;
#13016 = PRODUCT_CONTEXT ( 'NONE', #346, 'mechanical' ) ;
#13017 = CARTESIAN_POINT ( 'NONE',  ( 6.123233995736766282E-16, 2.000000000000000000, 5.000000000000000000 ) ) ;
#13018 = CARTESIAN_POINT ( 'NONE',  ( 27.24356964375000345, 198.6781250006145569, -3.336375036156643733E-15 ) ) ;
#13019 = CARTESIAN_POINT ( 'NONE',  ( 8.927990412390371944, 104.5273137178985650, 13.04141134922778811 ) ) ;
#13020 = CARTESIAN_POINT ( 'NONE',  ( -50.98586230271183695, 206.8500491399821328, 5.686928522499748340 ) ) ;
#13021 = ORIENTED_EDGE ( 'NONE', *, *, #11477, .F. ) ;
#13022 = LINE ( 'NONE', #36309, #30757 ) ;
#13023 = CARTESIAN_POINT ( 'NONE',  ( 6.932735513423970097, 138.3476862821014493, 10.69584247140445044 ) ) ;
#13024 = LINE ( 'NONE', #32916, #7194 ) ;
#13025 = CARTESIAN_POINT ( 'NONE',  ( 27.81522707900330715, 5.407089921784862696, 163.7168658290902101 ) ) ;
#13026 = CARTESIAN_POINT ( 'NONE',  ( -5.770363421893818234, 106.4351862821014691, -14.38691631536207005 ) ) ;
#13027 = CARTESIAN_POINT ( 'NONE',  ( -51.58705436395489130, 205.3262412349647548, -4.842901733360204908 ) ) ;
#13028 = CARTESIAN_POINT ( 'NONE',  ( 10.31873187879411091, -3.604726614523240613, -3.703124999385514649 ) ) ;
#13029 = CARTESIAN_POINT ( 'NONE',  ( 8.710071997420127943, 45.48518628210144499, 3.796722387233375073 ) ) ;
#13030 = CARTESIAN_POINT ( 'NONE',  ( 24.00000000000000000, -5.196152422706629359, -3.450000000000008615 ) ) ;
#13031 = CARTESIAN_POINT ( 'NONE',  ( -42.28497103062156270, 202.6965474657331185, -4.350049139982091084 ) ) ;
#13032 = CARTESIAN_POINT ( 'NONE',  ( -50.22894823740647752, 235.3444610600932094, -2.499999999999996447 ) ) ;
#13033 = EDGE_CURVE ( 'NONE', #21578, #2980, #5693, .T. ) ;
#13034 = CARTESIAN_POINT ( 'NONE',  ( 0.1745138560725515708, 70.21018628210144641, -12.50000000000000355 ) ) ;
#13035 = CARTESIAN_POINT ( 'NONE',  ( 26.99999999999999645, 199.3625000000000114, -15.58845726811990495 ) ) ;
#13036 = CARTESIAN_POINT ( 'NONE',  ( 20.99999999999999645, 185.0294372515228645, 0.000000000000000000 ) ) ;
#13038 = EDGE_LOOP ( 'NONE', ( #24183, #29294, #2619, #13486 ) ) ;
#13037 = CARTESIAN_POINT ( 'NONE',  ( -3.474262827703337830, 42.03518628210144925, -8.843639120294326972 ) ) ;
#13039 = CARTESIAN_POINT ( 'NONE',  ( 20.99999999999999645, 0.000000000000000000, -8.000000000000000000 ) ) ;
#13040 = VERTEX_POINT ( 'NONE', #194 ) ;
#13041 = CARTESIAN_POINT ( 'NONE',  ( 21.00000000000000000, -6.928203230275506996, -2.587499999999983480 ) ) ;
#13042 = CARTESIAN_POINT ( 'NONE',  ( -67.81622103062156270, 211.6261429550005744, 6.530955311639227823 ) ) ;
#13043 = CARTESIAN_POINT ( 'NONE',  ( 37.08938175740716758, -3.604726614523238837, 162.2655472845101201 ) ) ;
#13044 = CARTESIAN_POINT ( 'NONE',  ( 36.82467767225077182, -3.464101615137755275, 162.0346139941553076 ) ) ;
#13045 = CARTESIAN_POINT ( 'NONE',  ( 15.00000000000000178, 245.0875000000000057, 3.464101615137757051 ) ) ;
#13046 = FACE_OUTER_BOUND ( 'NONE', #17684, .T. ) ;
#13047 = CARTESIAN_POINT ( 'NONE',  ( 4.622313124798831829, 92.16481371789855359, -11.61527771782809282 ) ) ;
#13048 = CARTESIAN_POINT ( 'NONE',  ( 4.622313124798573369, 111.0351862821014635, 11.61527771782819940 ) ) ;
#13049 = ORIENTED_EDGE ( 'NONE', *, *, #27983, .T. ) ;
#13050 = VERTEX_POINT ( 'NONE', #6264 ) ;
#13051 = CARTESIAN_POINT ( 'NONE',  ( 5.727106289114498080E-15, 197.9750000012290343, 31.17691453623979214 ) ) ;
#13052 = CARTESIAN_POINT ( 'NONE',  ( 15.00000000000000000, 248.6687500012290286, -3.464101615137752610 ) ) ;
#13053 = CARTESIAN_POINT ( 'NONE',  ( 14.25334919248795451, 65.71481371789855075, -6.092822981423661410 ) ) ;
#13054 = EDGE_CURVE ( 'NONE', #15189, #21803, #28478, .T. ) ;
#13055 = CARTESIAN_POINT ( 'NONE',  ( 26.75643035624999655, -3.323476615752267715, -6.365624999385492089 ) ) ;
#13056 = CARTESIAN_POINT ( 'NONE',  ( 21.00000000000000000, 246.1468750006145285, -6.646953231504538984 ) ) ;
#13057 = CARTESIAN_POINT ( 'NONE',  ( -58.51413769728822700, 212.1499508600178387, 3.954877714930865817 ) ) ;
#13058 = FACE_OUTER_BOUND ( 'NONE', #11816, .T. ) ;
#13059 = CARTESIAN_POINT ( 'NONE',  ( 5.233372021372610483, 64.85231371789855359, -8.152565276336593669 ) ) ;
#13060 = CARTESIAN_POINT ( 'NONE',  ( 13.44051670066910908, 5.407089921784856479, -7.865624999385534721 ) ) ;
#13061 = CARTESIAN_POINT ( 'NONE',  ( -5.233372021372612259, 106.2523137178985451, 8.152565276336593669 ) ) ;
#13062 = CARTESIAN_POINT ( 'NONE',  ( -13.62178482187500528, 199.7843750006145456, -23.59362340125807123 ) ) ;
#13063 = CARTESIAN_POINT ( 'NONE',  ( 11.48171059495408208, 28.91481371789854293, -4.944772684328420986 ) ) ;
#13064 = CARTESIAN_POINT ( 'NONE',  ( -8.962234695871760692, 85.16018628210144925, 8.715434833791933400 ) ) ;
#13065 = CARTESIAN_POINT ( 'NONE',  ( 10.56230152254410726, 0.000000000000000000, -8.887499998771003717 ) ) ;
#13066 = EDGE_CURVE ( 'NONE', #2189, #35593, #16267, .T. ) ;
#13067 = CARTESIAN_POINT ( 'NONE',  ( 26.99999999999999645, 196.2125000000000057, -15.58845726811990495 ) ) ;
#13068 = CARTESIAN_POINT ( 'NONE',  ( 30.86793661096031727, -7.209453229046475009, 162.7910315836186328 ) ) ;
#13069 = CARTESIAN_POINT ( 'NONE',  ( 19.68408634441911431, 5.407089921784862696, -6.196874999385537208 ) ) ;
#13070 = FACE_BOUND ( 'NONE', #24873, .T. ) ;
#13071 = CYLINDRICAL_SURFACE ( 'NONE', #28853, 7.500000000000000000 ) ;
#13072 = DIRECTION ( 'NONE',  ( -0.000000000000000000, -1.000000000000000000, -0.000000000000000000 ) ) ;
#13073 = CARTESIAN_POINT ( 'NONE',  ( 1.715153634034233487, 92.92268628210145209, 9.534712964251941258 ) ) ;
#13074 = CARTESIAN_POINT ( 'NONE',  ( 20.99999999999999645, 185.0294372515228645, 0.000000000000000000 ) ) ;
#13075 = ADVANCED_FACE ( 'NONE', ( #34690 ), #8920, .T. ) ;
#13076 = CARTESIAN_POINT ( 'NONE',  ( 7.228626920339068285, 135.4726862821014493, -10.49813415415989581 ) ) ;
#13077 = CARTESIAN_POINT ( 'NONE',  ( 15.00000000000000000, 0.000000000000000000, 0.000000000000000000 ) ) ;
#13078 = CARTESIAN_POINT ( 'NONE',  ( 18.12178482187500350, 240.8218750006145399, 4.985214923628407568 ) ) ;
#13079 = VERTEX_POINT ( 'NONE', #17460 ) ;
#13080 = CARTESIAN_POINT ( 'NONE',  ( 34.03340388509710834, 5.407089921784857367, 163.1540242288032232 ) ) ;
#13081 = CARTESIAN_POINT ( 'NONE',  ( 26.75643035624999655, 3.323476615752271712, -4.828124999385488003 ) ) ;
#13082 = CARTESIAN_POINT ( 'NONE',  ( 27.24356964375000345, 198.2843750006145456, -3.336375036156643733E-15 ) ) ;
#13083 = DIRECTION ( 'NONE',  ( -0.000000000000000000, 1.000000000000000000, -0.000000000000000000 ) ) ;
#13084 = CARTESIAN_POINT ( 'NONE',  ( 21.00000000000000000, 239.8187500012290059, 5.999999999999998224 ) ) ;
#13085 = CARTESIAN_POINT ( 'NONE',  ( 15.24356964375000167, 243.5968750006144887, 3.323476615752272600 ) ) ;
#13086 = CARTESIAN_POINT ( 'NONE',  ( -12.46528703574811558, 144.2023137178985621, 2.660918448318003726 ) ) ;
#13087 = CARTESIAN_POINT ( 'NONE',  ( 13.62178482187501416, 197.3093750006145513, 23.59362340125806767 ) ) ;
#13089 = ORIENTED_EDGE ( 'NONE', *, *, #198, .F. ) ;
#13088 = VERTEX_POINT ( 'NONE', #25790 ) ;
#13090 = CARTESIAN_POINT ( 'NONE',  ( 21.00000000000000000, 244.0093750006145115, 6.646953231504538984 ) ) ;
#13091 = CARTESIAN_POINT ( 'NONE',  ( -12.53471296425189152, 34.37731371789855217, -2.311890736173453309 ) ) ;
#13092 = CARTESIAN_POINT ( 'NONE',  ( 15.24356964375000167, -3.323476615752272600, -3.703124999385450700 ) ) ;
#13093 = CARTESIAN_POINT ( 'NONE',  ( 13.23911966647199812, 122.3523137178985394, 8.632099005475788900 ) ) ;
#13094 = CARTESIAN_POINT ( 'NONE',  ( 15.00000000000000178, -3.464101615137757051, -9.356249998770968190 ) ) ;
#13095 = ORIENTED_EDGE ( 'NONE', *, *, #6911, .F. ) ;
#13096 = CARTESIAN_POINT ( 'NONE',  ( 22.80587116629411781, 7.646167579472024665E-16, -5.371874999385517491 ) ) ;
#13097 = VERTEX_POINT ( 'NONE', #14058 ) ;
#13098 = CARTESIAN_POINT ( 'NONE',  ( 27.24356964375000345, 197.3281250006145342, -3.336375036156643733E-15 ) ) ;
#13099 = CARTESIAN_POINT ( 'NONE',  ( 6.932735513423970097, 138.3476862821014493, 10.69584247140445044 ) ) ;
#13100 = CARTESIAN_POINT ( 'NONE',  ( 19.68408634441910721, 5.407089921784857367, -0.7406249993855418268 ) ) ;
#13101 = CARTESIAN_POINT ( 'NONE',  ( 27.57990657358465114, 5.407089921784862696, 161.0271401442424803 ) ) ;
#13102 = AXIS2_PLACEMENT_3D ( 'NONE', #14607, #11945, #20112 ) ;
#13103 = CARTESIAN_POINT ( 'NONE',  ( -51.97544563604517265, 216.3070033484980854, 6.137860380172893926 ) ) ;
#13104 = CARTESIAN_POINT ( 'NONE',  ( 18.12178482187500350, 247.5718750006145115, 4.985214923628407568 ) ) ;
#13105 = CARTESIAN_POINT ( 'NONE',  ( 10.56230152254410903, 7.347880794884117764E-16, -10.00000000000000000 ) ) ;
#13106 = CARTESIAN_POINT ( 'NONE',  ( -47.02752896937850835, 212.3500491399821613, 3.839350919129088435 ) ) ;
#13107 = CARTESIAN_POINT ( 'NONE',  ( -77.00000000000002842, 206.0000000000000000, -2.499999999999998668 ) ) ;
#13108 = CARTESIAN_POINT ( 'NONE',  ( 10.56230152254411436, 3.464101615137752166, -1.724999998770991416 ) ) ;
#13109 = ORIENTED_EDGE ( 'NONE', *, *, #17603, .T. ) ;
#13110 = CARTESIAN_POINT ( 'NONE',  ( 26.99999999999999645, 7.347880794884117764E-16, -5.175000000000013145 ) ) ;
#13111 = CARTESIAN_POINT ( 'NONE',  ( -13.23911966647218463, 113.0476862821014663, 8.632099005475506459 ) ) ;
#13112 = CARTESIAN_POINT ( 'NONE',  ( -51.98288769728823411, 201.5309553116392181, -2.393094931466246855 ) ) ;
#13113 = VECTOR ( 'NONE', #35467, 1000.000000000000000 ) ;
#13114 = ADVANCED_FACE ( 'NONE', ( #11389 ), #29377, .F. ) ;
#13115 = CARTESIAN_POINT ( 'NONE',  ( 9.500000000000005329, 118.5101862821014720, 0.1745138560725188748 ) ) ;
#13116 = CARTESIAN_POINT ( 'NONE',  ( 20.99999999999999645, -6.928203230275506996, -2.531249998770942256 ) ) ;
#13117 = CARTESIAN_POINT ( 'NONE',  ( 8.715434833791931624, 9.260186282101429356, 8.962234695871760692 ) ) ;
#13118 = CARTESIAN_POINT ( 'NONE',  ( 10.56230152254410726, 0.000000000000000000, -8.550000000000029132 ) ) ;
#13119 = ORIENTED_EDGE ( 'NONE', *, *, #36911, .T. ) ;
#13120 = LINE ( 'NONE', #36972, #9447 ) ;
#13121 = CARTESIAN_POINT ( 'NONE',  ( 8.152565276336714462, 90.04768628210145209, -5.233372021372432847 ) ) ;
#13122 = CARTESIAN_POINT ( 'NONE',  ( 22.56230152254410370, 7.347880794884117764E-16, -5.962499998771020771 ) ) ;
#13123 = CARTESIAN_POINT ( 'NONE',  ( -1.715153634034442431, 133.2773137178985507, 9.534712964251900402 ) ) ;
#13124 = CARTESIAN_POINT ( 'NONE',  ( -27.24356964374999635, 198.4906250006145569, 15.72908226750539384 ) ) ;
#13125 = CARTESIAN_POINT ( 'NONE',  ( 16.56230152254410726, 0.000000000000000000, -10.00000000000000000 ) ) ;
#13126 = CARTESIAN_POINT ( 'NONE',  ( 13.62178482187501416, 196.8593750006145342, 23.59362340125806767 ) ) ;
#13127 = CARTESIAN_POINT ( 'NONE',  ( 2.999999999999997335, 244.5000000000000000, 2.500000000000000000 ) ) ;
#13128 = CARTESIAN_POINT ( 'NONE',  ( 19.56230152254411792, 5.196152422706637353, -3.750000000000031086 ) ) ;
#13129 = CARTESIAN_POINT ( 'NONE',  ( 3.474262827703532341, 64.56481371789854506, -8.843639120294245259 ) ) ;
#13130 = ORIENTED_EDGE ( 'NONE', *, *, #35419, .F. ) ;
#13131 = CARTESIAN_POINT ( 'NONE',  ( 15.00000000000000000, 243.3062500012290457, 0.000000000000000000 ) ) ;
#13132 = CARTESIAN_POINT ( 'NONE',  ( 4.944772684328420986, 86.41481371789855359, 11.48171059495408208 ) ) ;
#13133 = CARTESIAN_POINT ( 'NONE',  ( 19.68408634441911431, 5.407089921784862696, -6.196874999385537208 ) ) ;
#13134 = CARTESIAN_POINT ( 'NONE',  ( 15.00000000000000000, 242.7625000000000171, -3.464101615137752610 ) ) ;
#13135 = CARTESIAN_POINT ( 'NONE',  ( 26.75643035624999655, -3.323476615752267715, -5.465624999385500615 ) ) ;
#13136 = CARTESIAN_POINT ( 'NONE',  ( -12.53471296425189152, 43.57731371789855501, -2.311890736173453753 ) ) ;
#13137 = ORIENTED_EDGE ( 'NONE', *, *, #4364, .F. ) ;
#13138 = CARTESIAN_POINT ( 'NONE',  ( 26.75643035624999655, 3.323476615752271268, -6.628124999385470062 ) ) ;
#13139 = VECTOR ( 'NONE', #1435, 1000.000000000000000 ) ;
#13140 = CARTESIAN_POINT ( 'NONE',  ( 11.48171059495397728, 27.08518628210144996, 4.944772684328674117 ) ) ;
#13141 = EDGE_CURVE ( 'NONE', #11399, #3975, #26416, .T. ) ;
#13142 = EDGE_CURVE ( 'NONE', #2631, #36062, #8376, .T. ) ;
#13143 = CARTESIAN_POINT ( 'NONE',  ( 37.52080268400803931, -3.604726614523238837, 167.1967110400642866 ) ) ;
#13144 = CARTESIAN_POINT ( 'NONE',  ( -55.93377896937850124, 208.3738570449995109, 6.530955311639247363 ) ) ;
#13145 =( NAMED_UNIT ( * ) PLANE_ANGLE_UNIT ( ) SI_UNIT ( $, .RADIAN. ) );
#13146 = CARTESIAN_POINT ( 'NONE',  ( 26.99999999999999645, 7.347880794884117764E-16, -7.424999999999987388 ) ) ;
#13147 = CARTESIAN_POINT ( 'NONE',  ( -4.944772684328424539, 72.61481371789855643, -11.48171059495408031 ) ) ;
#13148 = CARTESIAN_POINT ( 'NONE',  ( -49.01413769728823411, 212.1499508600178387, 3.954877714930865817 ) ) ;
#13149 =( BOUNDED_CURVE ( )  B_SPLINE_CURVE ( 2, ( #5496, #17079, #28618, #12879, #32967, #9664, #32780 ),
 .UNSPECIFIED., .F., .F. ) 
 B_SPLINE_CURVE_WITH_KNOTS ( ( 3, 2, 2, 3 ),
 ( 0.1086956521739124576, 0.1159420289855068037, 0.1231884057971011498, 0.1304347826086954820 ),
 .UNSPECIFIED. ) 
 CURVE ( )  GEOMETRIC_REPRESENTATION_ITEM ( )  RATIONAL_B_SPLINE_CURVE ( ( 1.000000000000010658, 0.8660254037844279384, 1.000000000000000000, 0.8660254037844387076, 1.000000000000000000, 0.8660254037844418162, 0.9999999999999968914 ) ) 
 REPRESENTATION_ITEM ( '' )  );
#13150 = CARTESIAN_POINT ( 'NONE',  ( -56.93080436395490551, 203.5000000000000000, -0.1155267958017335561 ) ) ;
#13151 = CARTESIAN_POINT ( 'NONE',  ( 24.00000000000000000, -5.196152422706629359, -2.943749998770950338 ) ) ;
#13152 = CARTESIAN_POINT ( 'NONE',  ( 14.25334919248795451, 47.31481371789856638, -6.092822981423661410 ) ) ;
#13153 = CARTESIAN_POINT ( 'NONE',  ( -40.89211230271183695, 201.5309553116392181, 2.393094931466368980 ) ) ;
#13154 = DIRECTION ( 'NONE',  ( 0.000000000000000000, 0.000000000000000000, 1.000000000000000000 ) ) ;
#13155 = CARTESIAN_POINT ( 'NONE',  ( -10.69584247140444866, 76.24768628210144072, 6.932735513423972762 ) ) ;
#13156 = CARTESIAN_POINT ( 'NONE',  ( 6.092822981423978490, 24.78518628210144215, -14.25334919248782306 ) ) ;
#13157 = CARTESIAN_POINT ( 'NONE',  ( 19.56230152254411792, 5.196152422706637353, -3.300000000000025135 ) ) ;
#13158 = CARTESIAN_POINT ( 'NONE',  ( -27.88991936466936750, 208.9463986166298639, -7.947561165778700421 ) ) ;
#13159 = ORIENTED_EDGE ( 'NONE', *, *, #19130, .F. ) ;
#13160 = CARTESIAN_POINT ( 'NONE',  ( 8.927990412390657937, 25.07268628210145067, -13.04141134922759804 ) ) ;
#13161 = CARTESIAN_POINT ( 'NONE',  ( 13.62178482187499640, 196.5031250006145456, -23.59362340125807123 ) ) ;
#13162 = CARTESIAN_POINT ( 'NONE',  ( 0.000000000000000000, 141.0000000000000000, 7.500000000000000000 ) ) ;
#13163 = CARTESIAN_POINT ( 'NONE',  ( 20.99999999999999645, 0.000000000000000000, -8.000000000000000000 ) ) ;
#13164 = CARTESIAN_POINT ( 'NONE',  ( -43.27455436395490551, 205.1570982666397356, 4.673758765035198159 ) ) ;
#13165 = CARTESIAN_POINT ( 'NONE',  ( 34.07795076420737246, -5.196152422706629359, 165.0605215108271864 ) ) ;
#13166 =( BOUNDED_CURVE ( )  B_SPLINE_CURVE ( 2, ( #30498, #36726, #2415, #1673, #7741, #4519, #19134 ),
 .UNSPECIFIED., .F., .F. ) 
 B_SPLINE_CURVE_WITH_KNOTS ( ( 3, 2, 2, 3 ),
 ( 0.000000000000000000, 0.007246376811594042525, 0.01449275362318808505, 0.02173913043478212584 ),
 .UNSPECIFIED. ) 
 CURVE ( )  GEOMETRIC_REPRESENTATION_ITEM ( )  RATIONAL_B_SPLINE_CURVE ( ( 1.000000000000000000, 0.8660254037844387076, 1.000000000000000000, 0.8660254037844387076, 1.000000000000000000, 0.8660254037844475894, 0.9999999999999911182 ) ) 
 REPRESENTATION_ITEM ( '' )  );
#13167 = CARTESIAN_POINT ( 'NONE',  ( 15.24356964375000167, 248.5468750006145342, 3.323476615752272600 ) ) ;
#13168 = CARTESIAN_POINT ( 'NONE',  ( -6.840914352311947333, 127.2398137178985422, -6.594114490232462877 ) ) ;
#13169 = CARTESIAN_POINT ( 'NONE',  ( 23.87821517812500005, 244.6093750006145342, 4.985214923628404016 ) ) ;
#13170 = ORIENTED_EDGE ( 'NONE', *, *, #18282, .T. ) ;
#13171 = CARTESIAN_POINT ( 'NONE',  ( 21.00000000000000355, 0.000000000000000000, 50.00000000000001421 ) ) ;
#13172 = CARTESIAN_POINT ( 'NONE',  ( 2.999999999999997335, 244.5000000000000000, -2.499999999999999556 ) ) ;
#13173 = CARTESIAN_POINT ( 'NONE',  ( -12.53471296425189152, 135.5773137178985905, -2.311890736173453309 ) ) ;
#13174 = ADVANCED_FACE ( 'NONE', ( #37162 ), #15552, .T. ) ;
#13175 = CARTESIAN_POINT ( 'NONE',  ( 13.44051670066911441, -5.407089921784859143, -5.915624999385554972 ) ) ;
#13176 = CARTESIAN_POINT ( 'NONE',  ( 24.87690945940258302, -3.604726614523240613, 165.9502056158071355 ) ) ;
#13177 = LINE ( 'NONE', #12614, #11740 ) ;
#13178 = EDGE_CURVE ( 'NONE', #17083, #36556, #4149, .T. ) ;
#13179 = CARTESIAN_POINT ( 'NONE',  ( -1.909035429704832693E-15, 198.5374999999999943, -31.17691453623979214 ) ) ;
#13180 = VERTEX_POINT ( 'NONE', #23897 ) ;
#13181 = CARTESIAN_POINT ( 'NONE',  ( -10.69584247140444866, 30.24768628210144783, 6.932735513423972762 ) ) ;
#13182 = ORIENTED_EDGE ( 'NONE', *, *, #24015, .T. ) ;
#13183 = ORIENTED_EDGE ( 'NONE', *, *, #15057, .T. ) ;
#13184 = CARTESIAN_POINT ( 'NONE',  ( 21.00000000000000000, 6.928203230275506996, -5.456249998770962506 ) ) ;
#13185 = CARTESIAN_POINT ( 'NONE',  ( 18.12178482187499640, 4.985214923628404904, -1.115624999385472771 ) ) ;
#13186 = CARTESIAN_POINT ( 'NONE',  ( 0.000000000000000000, 210.0000000000000284, 0.000000000000000000 ) ) ;
#13187 = CARTESIAN_POINT ( 'NONE',  ( -7.234628195640316228, 196.3075961894323598, -27.00000000000000000 ) ) ;
#13188 = CARTESIAN_POINT ( 'NONE',  ( 21.00000000000000000, 6.646953231504538984, -9.703124999385480010 ) ) ;
#13189 = CARTESIAN_POINT ( 'NONE',  ( -0.1745138560725500443, 74.81018628210145494, 12.50000000000000355 ) ) ;
#13190 = EDGE_CURVE ( 'NONE', #28808, #2436, #17475, .T. ) ;
#13191 = CARTESIAN_POINT ( 'NONE',  ( -15.53471296425188442, 6.777313717898553413, -2.908627838312459080 ) ) ;
#13192 = EDGE_CURVE ( 'NONE', #9065, #19072, #34172, .T. ) ;
#13193 = CARTESIAN_POINT ( 'NONE',  ( -27.00000000000000355, 197.3000000000000114, 0.000000000000000000 ) ) ;
#13194 = CARTESIAN_POINT ( 'NONE',  ( 20.21461154673234262, 212.0943692087130614, 5.961323472697788617 ) ) ;
#13195 = CARTESIAN_POINT ( 'NONE',  ( -52.56919563604517265, 214.5000000000000284, -0.1155267958017627827 ) ) ;
#13196 = FACE_OUTER_BOUND ( 'NONE', #34630, .T. ) ;
#13197 = AXIS2_PLACEMENT_3D ( 'NONE', #17541, #3869, #23407 ) ;
#13198 = CARTESIAN_POINT ( 'NONE',  ( 37.22668353578141875, -3.464101615137751278, 166.6295620403278406 ) ) ;
#13199 = CARTESIAN_POINT ( 'NONE',  ( 4.622313124798831829, 119.7648137178985763, -11.61527771782809282 ) ) ;
#13200 = CARTESIAN_POINT ( 'NONE',  ( -53.17038769728823411, 208.1428034533959703, 6.469044688360770401 ) ) ;
#13201 = CARTESIAN_POINT ( 'NONE',  ( -51.38913769728824121, 205.8500491399820760, -7.418979330068584233 ) ) ;
#13203 = APPLICATION_CONTEXT ( 'automotive_design' ) ;
#13202 = ITEM_DEFINED_TRANSFORMATION ( 'NONE', 'NONE', #23272,  #17215 ) ;
#13204 = CARTESIAN_POINT ( 'NONE',  ( 26.75643035624999655, -3.323476615752267271, -2.765624999385494664 ) ) ;
#13205 = CARTESIAN_POINT ( 'NONE',  ( 5.778771075727756162E-15, 195.8656250006145285, 31.45816453501075927 ) ) ;
#13206 = CARTESIAN_POINT ( 'NONE',  ( 11.08355503943118769, 104.2398137178985706, 10.83675517735179028 ) ) ;
#13207 = CARTESIAN_POINT ( 'NONE',  ( -44.85044563604515133, 205.1570982666397072, -4.673758765035155527 ) ) ;
#13208 = VERTEX_POINT ( 'NONE', #36004 ) ;
#13209 = CARTESIAN_POINT ( 'NONE',  ( 37.22995187613445012, 7.347880794884117764E-16, 166.6669193415062580 ) ) ;
#13210 = CARTESIAN_POINT ( 'NONE',  ( -0.1745138560725500443, 130.0101862821014436, 12.50000000000000355 ) ) ;
#13211 = CARTESIAN_POINT ( 'NONE',  ( 11.08355503943142750, 89.76018628210145778, -10.83675517735155225 ) ) ;
#13212 = CARTESIAN_POINT ( 'NONE',  ( -7.234628195640316228, 197.6575961894323257, -27.00000000000000000 ) ) ;
#13213 = CARTESIAN_POINT ( 'NONE',  ( 27.93288733171263516, 5.407089921784862696, 165.0617286715140608 ) ) ;
#13214 = CARTESIAN_POINT ( 'NONE',  ( 14.38691631536207538, 90.33518628210144641, -5.770363421893813793 ) ) ;
#13215 =( BOUNDED_CURVE ( )  B_SPLINE_CURVE ( 2, ( #33306, #36697, #30470, #10367, #19297, #30836, #36508 ),
 .UNSPECIFIED., .F., .F. ) 
 B_SPLINE_CURVE_WITH_KNOTS ( ( 3, 2, 2, 3 ),
 ( 0.2173913043478263030, 0.2246376811594205936, 0.2318840579710149119, 0.2391304347826092025 ),
 .UNSPECIFIED. ) 
 CURVE ( )  GEOMETRIC_REPRESENTATION_ITEM ( )  RATIONAL_B_SPLINE_CURVE ( ( 0.9999999999999958922, 0.8660254037844428154, 1.000000000000000000, 0.8660254037844387076, 1.000000000000000000, 0.8660254037844294928, 1.000000000000009326 ) ) 
 REPRESENTATION_ITEM ( '' )  );
#13216 = CARTESIAN_POINT ( 'NONE',  ( -51.98288769728822700, 203.5309553116391896, -1.857196546604028997 ) ) ;
#13217 = CARTESIAN_POINT ( 'NONE',  ( 10.31873187879411269, 3.604726614523236616, -4.678124999385532945 ) ) ;
#13218 = CARTESIAN_POINT ( 'NONE',  ( 9.534712964251941258, 44.62268628210144783, -1.715153634034235708 ) ) ;
#13219 = CARTESIAN_POINT ( 'NONE',  ( 18.00000000000000355, 246.4749999999999943, 5.196152422706632912 ) ) ;
#13220 = CARTESIAN_POINT ( 'NONE',  ( -33.97247103062156270, 205.6499508600178956, 7.303452534266880569 ) ) ;
#13221 = CARTESIAN_POINT ( 'NONE',  ( 10.31873187879410736, 3.604726614523240613, -9.684374999385530813 ) ) ;
#13222 = CARTESIAN_POINT ( 'NONE',  ( -11.61527771782819940, 67.33518628210144641, 4.622313124798574258 ) ) ;
#13223 = CARTESIAN_POINT ( 'NONE',  ( -13.49999999999998401, 199.1750000000000114, 23.38268590217985476 ) ) ;
#13224 = CLOSED_SHELL ( 'NONE', ( #3888, #18471, #23841, #30820, #34941, #14472, #15637, #27001, #10100, #12500, #27031, #3044, #24022, #10573, #28705, #15630, #11196, #4699, #24570, #28797, #6100, #5643, #16968, #23276, #18656, #26137, #4095, #28777, #17379, #27683, #30228, #1250, #5082, #19452, #23498, #25921, #2780, #29928, #35543, #25131, #26830, #30969, #14207, #8986, #20258, #26605, #9174, #17710, #11910, #16228, #37364, #3675, #3373, #6240, #15340, #12712, #135, #16143 ) ) ;
#13225 = AXIS2_PLACEMENT_3D ( 'NONE', #3416, #18787, #12699 ) ;
#13226 = CARTESIAN_POINT ( 'NONE',  ( 13.49999999999999645, 199.4000000000000341, -23.38268590217984766 ) ) ;
#13228 = CARTESIAN_POINT ( 'NONE',  ( 13.44051670066911086, 5.407089921784862696, -1.171874999385535965 ) ) ;
#13227 = CARTESIAN_POINT ( 'NONE',  ( -3.796722387233375073, 47.78518628210144215, 8.710071997420127943 ) ) ;
#13229 = CARTESIAN_POINT ( 'NONE',  ( 15.00000000000000000, 241.9000000000000057, 0.000000000000000000 ) ) ;
#13230 = ORIENTED_EDGE ( 'NONE', *, *, #37470, .F. ) ;
#13231 = CARTESIAN_POINT ( 'NONE',  ( 23.99999999999999645, 5.196152422706631135, -3.299999999999997158 ) ) ;
#13232 = CARTESIAN_POINT ( 'NONE',  ( 34.02850137456756130, 5.407089921784862696, 163.0979882770355971 ) ) ;
#13233 = CARTESIAN_POINT ( 'NONE',  ( 36.83121435295684165, 3.464101615137759271, 162.1093285965121709 ) ) ;
#13234 = CARTESIAN_POINT ( 'NONE',  ( 24.00000000000000000, 246.5499999999999829, 5.196152422706629359 ) ) ;
#13235 = DIRECTION ( 'NONE',  ( 0.9961946980917462113, 0.000000000000000000, -0.08715574274765118534 ) ) ;
#13236 = CARTESIAN_POINT ( 'NONE',  ( 10.69584247140429589, 85.55231371789857064, 6.932735513424201024 ) ) ;
#13237 = CARTESIAN_POINT ( 'NONE',  ( 8.962234695871762469, 89.76018628210144357, -8.715434833791931624 ) ) ;
#13238 = ORIENTED_EDGE ( 'NONE', *, *, #25674, .F. ) ;
#13239 = VECTOR ( 'NONE', #20641, 1000.000000000000000 ) ;
#13240 = VERTEX_POINT ( 'NONE', #10041 ) ;
#13241 = CARTESIAN_POINT ( 'NONE',  ( -1.909035429704832693E-15, 199.1000000012290627, -31.17691453623979214 ) ) ;
#13242 = FACE_OUTER_BOUND ( 'NONE', #25064, .T. ) ;
#13243 = CARTESIAN_POINT ( 'NONE',  ( -5.770363421894122880, 50.76481371789856212, 14.38691631536194393 ) ) ;
#13244 = CARTESIAN_POINT ( 'NONE',  ( 23.87821517812499650, 4.985214923628404904, -7.603124999385480365 ) ) ;
#13245 = CARTESIAN_POINT ( 'NONE',  ( 18.12178482187499640, 244.3843750006145115, -4.985214923628404904 ) ) ;
#13246 = CARTESIAN_POINT ( 'NONE',  ( -60.09747103062157692, 212.3500491399821613, -3.839350919129076445 ) ) ;
#13247 = CARTESIAN_POINT ( 'NONE',  ( 2.999999999999997335, 244.5000000000000000, -5.000000000000001776 ) ) ;
#13248 = CARTESIAN_POINT ( 'NONE',  ( 0.1745138560723095977, 59.38981371789856212, 9.500000000000005329 ) ) ;
#13249 = CARTESIAN_POINT ( 'NONE',  ( 10.31873187879411091, -3.604726614523240613, -6.853124999385484806 ) ) ;
#13250 = AXIS2_PLACEMENT_3D ( 'NONE', #28209, #24987, #11151 ) ;
#13251 = CARTESIAN_POINT ( 'NONE',  ( -8.152565276336593669, 99.35231371789856780, -5.233372021372610483 ) ) ;
#13252 = CARTESIAN_POINT ( 'NONE',  ( 24.97165984609394940, 0.000000000000000000, 164.2385592436587558 ) ) ;
#13253 = CARTESIAN_POINT ( 'NONE',  ( -8.962234695871565293, 26.03981371789855359, -8.715434833792128799 ) ) ;
#13254 = CARTESIAN_POINT ( 'NONE',  ( -11.48171059495397373, 77.68518628210145494, -4.944772684328680334 ) ) ;
#13255 = CARTESIAN_POINT ( 'NONE',  ( 19.56230152254411436, -5.196152422706629359, -8.287499998771014731 ) ) ;
#13256 = LINE ( 'NONE', #9843, #29820 ) ;
#13257 = CARTESIAN_POINT ( 'NONE',  ( 27.67632261399923976, -5.407089921784859143, 162.1291805290064474 ) ) ;
#13258 = CARTESIAN_POINT ( 'NONE',  ( 22.80587116629411781, 3.604726614523243278, -6.684374999385514826 ) ) ;
#13259 = CARTESIAN_POINT ( 'NONE',  ( -13.50000000000000533, 195.5375000012290343, -23.38268590217984411 ) ) ;
#13260 = CARTESIAN_POINT ( 'NONE',  ( -5.233372021372430183, 87.74768628210144072, -8.152565276336710909 ) ) ;
#13261 = CARTESIAN_POINT ( 'NONE',  ( 10.56230152254410726, 0.000000000000000000, -5.850000000000049383 ) ) ;
#13262 = CARTESIAN_POINT ( 'NONE',  ( 2.660918448318279950, 125.6976862821014578, -12.46528703574805697 ) ) ;
#13263 = CARTESIAN_POINT ( 'NONE',  ( 16.56230152254411436, 6.928203230275514990, -3.262500000000057021 ) ) ;
#13264 = CARTESIAN_POINT ( 'NONE',  ( 18.12178482187500350, 239.9218750006145058, 4.985214923628407568 ) ) ;
#13265 = ORIENTED_EDGE ( 'NONE', *, *, #586, .F. ) ;
#13266 = CARTESIAN_POINT ( 'NONE',  ( 27.89856975800574546, 5.407089921784856479, 164.6694770091404223 ) ) ;
#13267 = CARTESIAN_POINT ( 'NONE',  ( 15.24356964374999990, 3.323476615752268604, -5.128124999385462957 ) ) ;
#13268 = CARTESIAN_POINT ( 'NONE',  ( 27.24356964375000700, 198.2468750006145513, 15.72908226750537075 ) ) ;
#13269 = DIRECTION ( 'NONE',  ( -0.000000000000000000, -1.000000000000000000, -0.000000000000000000 ) ) ;
#13270 = CARTESIAN_POINT ( 'NONE',  ( 23.87821517812500005, 243.7093750006145285, 4.985214923628404016 ) ) ;
#13271 = DIRECTION ( 'NONE',  ( -0.000000000000000000, -0.000000000000000000, 1.000000000000000000 ) ) ;
#13272 = CARTESIAN_POINT ( 'NONE',  ( -8.715434833792127023, 143.3398137178985507, 8.962234695871568846 ) ) ;
#13273 = CARTESIAN_POINT ( 'NONE',  ( -27.24356964375000345, 195.3218750006145399, -15.72908226750537786 ) ) ;
#13275 = ORIENTED_EDGE ( 'NONE', *, *, #36317, .T. ) ;
#13274 = VERTEX_POINT ( 'NONE', #26721 ) ;
#13276 = CARTESIAN_POINT ( 'NONE',  ( 26.75643035624999655, 243.6718750006145058, -7.049594010296217766E-16 ) ) ;
#13277 = CARTESIAN_POINT ( 'NONE',  ( 11.48171059495408208, 10.51481371789855856, -4.944772684328420986 ) ) ;
#13278 = CARTESIAN_POINT ( 'NONE',  ( 18.12178482187499640, 4.985214923628404904, -4.265624999385458693 ) ) ;
#13279 = CARTESIAN_POINT ( 'NONE',  ( -11.08355503943118592, 108.8398137178985507, -10.83675517735179383 ) ) ;
#13280 = CARTESIAN_POINT ( 'NONE',  ( 10.56230152254410903, 0.000000000000000000, -2.250000000000057732 ) ) ;
#13281 = CARTESIAN_POINT ( 'NONE',  ( 15.00000000000000000, 3.464101615137752166, -8.531249998770938703 ) ) ;
#13282 = CARTESIAN_POINT ( 'NONE',  ( 10.31873187879410736, 3.604726614523240613, -5.184374999385507721 ) ) ;
#13283 = ORIENTED_EDGE ( 'NONE', *, *, #12010, .T. ) ;
#13284 = CARTESIAN_POINT ( 'NONE',  ( 27.00000000000000355, 198.0875000012290457, -3.306546357697854128E-15 ) ) ;
#13285 = CARTESIAN_POINT ( 'NONE',  ( -4.944772684328673229, 139.7851862821014493, 11.48171059495397728 ) ) ;
#13286 = CARTESIAN_POINT ( 'NONE',  ( 13.44051670066910908, -5.407089921784859143, -0.5156249993855110958 ) ) ;
#13287 = CARTESIAN_POINT ( 'NONE',  ( 36.93576976081443775, 7.646167579472024665E-16, 160.5097541291234506 ) ) ;
#13288 = CARTESIAN_POINT ( 'NONE',  ( -49.00669563604517265, 209.8844732041981729, -8.500000000000003553 ) ) ;
#13289 = CARTESIAN_POINT ( 'NONE',  ( 26.75643035624999655, 246.3718750006145228, -7.049594010296217766E-16 ) ) ;
#13290 = SHAPE_REPRESENTATION_RELATIONSHIP ( 'NONE' , 'NONE' ,  #29986, #10611 ) ;
#13291 = CARTESIAN_POINT ( 'NONE',  ( 27.00000000000000000, 202.0000000000000000, 0.000000000000000000 ) ) ;
#13292 = CARTESIAN_POINT ( 'NONE',  ( -33.17336230271183695, 213.9548777149308023, 2.149950860017852960 ) ) ;
#13293 = CARTESIAN_POINT ( 'NONE',  ( -10.69584247140444866, 131.4476862821014436, 6.932735513423972762 ) ) ;
#13294 = CARTESIAN_POINT ( 'NONE',  ( 10.56230152254410903, 0.000000000000000000, -1.687499998771019305 ) ) ;
#13295 = ORIENTED_EDGE ( 'NONE', *, *, #33728, .F. ) ;
#13296 = CARTESIAN_POINT ( 'NONE',  ( 21.00000000000000355, 0.000000000000000000, 50.00000000000001421 ) ) ;
#13297 = SURFACE_STYLE_FILL_AREA ( #33943 ) ;
#13298 = CARTESIAN_POINT ( 'NONE',  ( 2.908627838312118019, 120.5226862821014322, 15.53471296425195369 ) ) ;
#13299 = LINE ( 'NONE', #31291, #7273 ) ;
#13300 = CARTESIAN_POINT ( 'NONE',  ( 4.944772684328679446, 15.58518628210145351, -11.48171059495397373 ) ) ;
#13301 = EDGE_CURVE ( 'NONE', #26963, #31128, #4396, .T. ) ;
#13302 = CARTESIAN_POINT ( 'NONE',  ( 19.56230152254411792, 5.196152422706637353, -9.600000000000052935 ) ) ;
#13303 = ORIENTED_EDGE ( 'NONE', *, *, #8939, .T. ) ;
#13304 = DIRECTION ( 'NONE',  ( 0.08715574274765150453, 0.000000000000000000, 0.9961946980917461003 ) ) ;
#13305 = CARTESIAN_POINT ( 'NONE',  ( 9.500000000000005329, 81.71018628210144641, 0.1745138560725188748 ) ) ;
#13306 = CARTESIAN_POINT ( 'NONE',  ( 8.152565276336593669, 122.3523137178985394, 5.233372021372610483 ) ) ;
#13307 = CARTESIAN_POINT ( 'NONE',  ( 27.24356964375000700, 196.8406250006145513, 15.72908226750537075 ) ) ;
#13308 = CARTESIAN_POINT ( 'NONE',  ( 18.00000000000000355, 245.1250000000000000, 5.196152422706632912 ) ) ;
#13309 = CARTESIAN_POINT ( 'NONE',  ( -13.62178482187500528, 198.4343750006145228, -23.59362340125807123 ) ) ;
#13310 = CARTESIAN_POINT ( 'NONE',  ( 18.00000000000000355, -5.196152422706632912, -1.668749998770951981 ) ) ;
#13311 = CARTESIAN_POINT ( 'NONE',  ( 24.00000000000000000, 242.0499999999999829, 5.196152422706629359 ) ) ;
#13312 = EDGE_CURVE ( 'NONE', #19909, #31630, #21619, .T. ) ;
#13313 = CARTESIAN_POINT ( 'NONE',  ( -0.1745138560723084320, 63.98981371789855643, -9.500000000000005329 ) ) ;
#13314 = CARTESIAN_POINT ( 'NONE',  ( 21.00000000000000000, 6.928203230275506996, -9.562499999999998224 ) ) ;
#13315 = ORIENTED_EDGE ( 'NONE', *, *, #12010, .F. ) ;
#13316 = CARTESIAN_POINT ( 'NONE',  ( 15.00000000000000000, 240.5687500012290343, -3.464101615137752166 ) ) ;
#13317 = CARTESIAN_POINT ( 'NONE',  ( -8.962234695871565293, 53.63981371789855501, -8.715434833792128799 ) ) ;
#13318 = CARTESIAN_POINT ( 'NONE',  ( 10.31873187879411091, 3.604726614523240613, -6.984374999385522642 ) ) ;
#13319 = DIRECTION ( 'NONE',  ( -1.000000000000000000, -6.123233995736766036E-17, 0.000000000000000000 ) ) ;
#13320 = CARTESIAN_POINT ( 'NONE',  ( 23.87821517812499650, 4.985214923628404904, -7.603124999385480365 ) ) ;
#13321 = CARTESIAN_POINT ( 'NONE',  ( 12.53471296425189330, 29.77731371789854720, 2.311890736173451977 ) ) ;
#13322 = ORIENTED_EDGE ( 'NONE', *, *, #28167, .F. ) ;
#13323 = CARTESIAN_POINT ( 'NONE',  ( 23.87821517812500005, -4.985214923628404016, -6.740624999385463667 ) ) ;
#13324 = EDGE_CURVE ( 'NONE', #27444, #8598, #511, .T. ) ;
#13325 = CARTESIAN_POINT ( 'NONE',  ( -2.311890736173176641, 23.92268628210143788, -12.53471296425194836 ) ) ;
#13326 = CARTESIAN_POINT ( 'NONE',  ( -30.20461230271182984, 208.1428034533958851, -6.469044688360754414 ) ) ;
#13327 = AXIS2_PLACEMENT_3D ( 'NONE', #28258, #25414, #27703 ) ;
#13328 = CARTESIAN_POINT ( 'NONE',  ( -52.17336230271183695, 215.6869285224997270, 3.149950860017831200 ) ) ;
#13329 = SURFACE_SIDE_STYLE ('',( #4973 ) ) ;
#13330 = CARTESIAN_POINT ( 'NONE',  ( 10.56230152254410548, 0.000000000000000000, -9.450000000000041922 ) ) ;
#13331 = CARTESIAN_POINT ( 'NONE',  ( 7.228626920338837358, 67.72731371789856780, 10.49813415416005036 ) ) ;
#13332 = CARTESIAN_POINT ( 'NONE',  ( -34.36830436395490551, 209.8844732041982297, 4.499999999999996447 ) ) ;
#13333 = CARTESIAN_POINT ( 'NONE',  ( -55.94122103062156270, 208.3738570449993404, -6.530955311639226935 ) ) ;
#13334 = CARTESIAN_POINT ( 'NONE',  ( 20.99999999999999645, 0.000000000000000000, -8.000000000000000000 ) ) ;
#13335 = CARTESIAN_POINT ( 'NONE',  ( 14.99999999999960387, -3.464101615137527457, -3.056249998770969256 ) ) ;
#13336 = CARTESIAN_POINT ( 'NONE',  ( 15.53471296425188797, 48.17731371789854222, 2.908627838312457747 ) ) ;
#13337 = CARTESIAN_POINT ( 'NONE',  ( -50.19419563604517975, 201.5000000000000000, 0.1155267958018195706 ) ) ;
#13338 = CIRCLE ( 'NONE', #34519, 7.500000000000000000 ) ;
#13339 = CARTESIAN_POINT ( 'NONE',  ( -50.22894823740646331, 235.3444610600932094, -7.500000000000000000 ) ) ;
#13340 = CARTESIAN_POINT ( 'NONE',  ( 8.962234695871762469, 62.16018628210144215, -8.715434833791931624 ) ) ;
#13341 = CARTESIAN_POINT ( 'NONE',  ( 14.38691631536207538, 7.535186282101451916, -5.770363421893813793 ) ) ;
#13342 = CARTESIAN_POINT ( 'NONE',  ( 13.56230152254410726, 5.196152422706636465, -0.9750000000000591527 ) ) ;
#13343 = CARTESIAN_POINT ( 'NONE',  ( 26.97716818855048260, 0.000000000000000000, 49.47706554351410801 ) ) ;
#13344 = VERTEX_POINT ( 'NONE', #5650 ) ;
#13345 = CARTESIAN_POINT ( 'NONE',  ( -15.50000000000000533, 31.11018628210143433, -0.1745138560725808530 ) ) ;
#13346 = CARTESIAN_POINT ( 'NONE',  ( 20.99999999999999645, 185.0294372515228645, 5.999999999999999112 ) ) ;
#13347 = EDGE_CURVE ( 'NONE', #33209, #3896, #152, .T. ) ;
#13348 = CARTESIAN_POINT ( 'NONE',  ( 5.778771075727756162E-15, 198.6218750006145513, 31.45816453501075927 ) ) ;
#13349 = CARTESIAN_POINT ( 'NONE',  ( 34.10736582727759725, -5.196152422706635576, 165.3967372202087915 ) ) ;
#13350 = FACE_OUTER_BOUND ( 'NONE', #33443, .T. ) ;
#13351 = DIRECTION ( 'NONE',  ( 0.000000000000000000, 1.000000000000000000, 0.000000000000000000 ) ) ;
#13352 = CARTESIAN_POINT ( 'NONE',  ( -0.1745138560725500443, 10.41018628210144215, 12.50000000000000355 ) ) ;
#13353 = CARTESIAN_POINT ( 'NONE',  ( 15.24356964375000167, 246.7468750006145228, 3.323476615752272600 ) ) ;
#13354 = CARTESIAN_POINT ( 'NONE',  ( -7.954856959092309943, 116.0273137178985792, 5.529263428287300108 ) ) ;
#13355 = CARTESIAN_POINT ( 'NONE',  ( 23.87821517812500005, 243.2593750006145399, 4.985214923628404016 ) ) ;
#13356 = VECTOR ( 'NONE', #27149, 1000.000000000000000 ) ;
#13357 = EDGE_LOOP ( 'NONE', ( #34103, #29203, #1088, #2545 ) ) ;
#13358 = CARTESIAN_POINT ( 'NONE',  ( 26.99999999999999645, 249.4187500012290286, -3.464101615137755275 ) ) ;
#13359 = CARTESIAN_POINT ( 'NONE',  ( 7.228626920338837358, 141.3273137178985621, 10.49813415416005036 ) ) ;
#13360 = CARTESIAN_POINT ( 'NONE',  ( 10.31873187879411269, 3.604726614523236616, -9.178124999385520510 ) ) ;
#13361 = CARTESIAN_POINT ( 'NONE',  ( 24.71349244175073778, 3.604726614523236616, 164.0823405568851570 ) ) ;
#13362 = DIRECTION ( 'NONE',  ( 0.000000000000000000, 0.000000000000000000, 1.000000000000000000 ) ) ;
#13363 = CARTESIAN_POINT ( 'NONE',  ( -1.909035429704832693E-15, 197.1875000000000284, -31.17691453623979214 ) ) ;
#13364 = ORIENTED_EDGE ( 'NONE', *, *, #25401, .T. ) ;
#13365 = CARTESIAN_POINT ( 'NONE',  ( 2.311890736173175753, 28.52268628210144641, 12.53471296425194659 ) ) ;
#13366 = ORIENTED_EDGE ( 'NONE', *, *, #8311, .T. ) ;
#13367 = ORIENTED_EDGE ( 'NONE', *, *, #31820, .F. ) ;
#13368 = CARTESIAN_POINT ( 'NONE',  ( 23.99999999999999645, 5.196152422706631135, -3.693749998770950782 ) ) ;
#13369 = CARTESIAN_POINT ( 'NONE',  ( 15.24356964374999990, 3.323476615752268604, -0.1781249993854788494 ) ) ;
#13370 = CARTESIAN_POINT ( 'NONE',  ( 18.00000000000000355, 242.0312500012290400, 5.196152422706632912 ) ) ;
#13371 = CARTESIAN_POINT ( 'NONE',  ( 18.00000000000000000, 5.196152422706630247, -5.925000000000013145 ) ) ;
#13372 = CARTESIAN_POINT ( 'NONE',  ( 15.24356964375000167, -3.323476615752272600, -7.753124999385476279 ) ) ;
#13373 = CARTESIAN_POINT ( 'NONE',  ( -11.48171059495397373, 77.68518628210145494, -4.944772684328680334 ) ) ;
#13374 = CARTESIAN_POINT ( 'NONE',  ( 10.83675517735179206, 9.939813717898537959, -11.08355503943118769 ) ) ;
#13375 =( BOUNDED_CURVE ( )  B_SPLINE_CURVE ( 3, ( #323, #6204, #35192, #14928 ),
 .UNSPECIFIED., .F., .F. ) 
 B_SPLINE_CURVE_WITH_KNOTS ( ( 4, 4 ),
 ( 1.570796326794937858, 3.141592653589793116 ),
 .UNSPECIFIED. ) 
 CURVE ( )  GEOMETRIC_REPRESENTATION_ITEM ( )  RATIONAL_B_SPLINE_CURVE ( ( 1.000000000000000000, 0.8047378541243747074, 0.8047378541243747074, 1.000000000000000000 ) ) 
 REPRESENTATION_ITEM ( '' )  );
#13376 = DIRECTION ( 'NONE',  ( -0.000000000000000000, 0.000000000000000000, 1.000000000000000000 ) ) ;
#13377 = CARTESIAN_POINT ( 'NONE',  ( 6.642437016334202582, 215.3840861188750466, 2.655215585727055849 ) ) ;
#13378 = CARTESIAN_POINT ( 'NONE',  ( -58.50669563604516554, 209.8844732041982297, -4.499999999999996447 ) ) ;
#13379 = CARTESIAN_POINT ( 'NONE',  ( 13.50000000000001421, 197.0000000000000000, 23.38268590217984055 ) ) ;
#13380 = CARTESIAN_POINT ( 'NONE',  ( 31.12531841381553477, -6.928203230275506996, 165.7329190520329973 ) ) ;
#13381 = CARTESIAN_POINT ( 'NONE',  ( 11.48171059495408208, 120.9148137178985536, -4.944772684328420986 ) ) ;
#13382 = CARTESIAN_POINT ( 'NONE',  ( -45.25372103062155560, 216.5309553116391612, -1.626142955000564383 ) ) ;
#13383 = CARTESIAN_POINT ( 'NONE',  ( -63.06622103062156270, 212.1620413398628671, 8.530955311639223382 ) ) ;
#13384 = VECTOR ( 'NONE', #486, 1000.000000000000000 ) ;
#13385 = CARTESIAN_POINT ( 'NONE',  ( 15.24356964375000167, -3.323476615752272600, -1.565624999385463179 ) ) ;
#13386 = CARTESIAN_POINT ( 'NONE',  ( 13.62178482187501416, 196.3531250006145115, 23.59362340125806767 ) ) ;
#13387 = CARTESIAN_POINT ( 'NONE',  ( -5.770363421894122880, 96.76481371789854791, 14.38691631536194393 ) ) ;
#13388 = CARTESIAN_POINT ( 'NONE',  ( -43.26711230271183695, 216.4690446883607535, -1.857196546604089393 ) ) ;
#13389 = ORIENTED_EDGE ( 'NONE', *, *, #30081, .F. ) ;
#13390 = CARTESIAN_POINT ( 'NONE',  ( 25.28542051998549667, 0.000000000000000000, 167.8248601567890432 ) ) ;
#13391 = CARTESIAN_POINT ( 'NONE',  ( -7.228626920339069173, 121.6726862821014521, 10.49813415415989581 ) ) ;
#13392 = CARTESIAN_POINT ( 'NONE',  ( 11.08355503943142750, 62.16018628210144925, -10.83675517735155225 ) ) ;
#13393 = CARTESIAN_POINT ( 'NONE',  ( 37.07307153918868181, 7.347880794884117764E-16, 164.8737688849411143 ) ) ;
#13394 =( BOUNDED_CURVE ( )  B_SPLINE_CURVE ( 2, ( #30862, #33889, #13810, #25539, #33515, #16093, #10951, #28011, #2044 ),
 .UNSPECIFIED., .F., .F. ) 
 B_SPLINE_CURVE_WITH_KNOTS ( ( 3, 2, 2, 2, 3 ),
 ( 0.06250000000000000000, 0.06944444444444444753, 0.08333333333333332871, 0.09722222222222222376, 0.1041666666666666713 ),
 .UNSPECIFIED. ) 
 CURVE ( )  GEOMETRIC_REPRESENTATION_ITEM ( )  RATIONAL_B_SPLINE_CURVE ( ( 0.9330127018922194093, 0.9330127018922194093, 1.000000000000000000, 0.8660254037844387076, 1.000000000000000000, 0.8660254037844387076, 1.000000000000000000, 0.9330127018922192983, 0.9330127018922194093 ) ) 
 REPRESENTATION_ITEM ( '' )  );
#13395 = CARTESIAN_POINT ( 'NONE',  ( 37.32797060317886917, 7.646167579472024665E-16, 164.9926302705362957 ) ) ;
#13396 = CARTESIAN_POINT ( 'NONE',  ( 14.38691631536207538, 81.13518628210145778, -5.770363421893813793 ) ) ;
#13397 = CARTESIAN_POINT ( 'NONE',  ( -50.79538769728823411, 211.8571965466040012, -6.469044688360769513 ) ) ;
#13398 = ADVANCED_FACE ( 'NONE', ( #8876 ), #17233, .F. ) ;
#13399 = CARTESIAN_POINT ( 'NONE',  ( 13.44051670066911797, -5.407089921784859143, -6.365624999385560479 ) ) ;
#13400 = CARTESIAN_POINT ( 'NONE',  ( -0.1745138560725182642, 38.01018628210144357, 9.500000000000005329 ) ) ;
#13401 = CARTESIAN_POINT ( 'NONE',  ( 21.00000000000000000, 246.5124999999999602, 5.999999999999998224 ) ) ;
#13402 = CARTESIAN_POINT ( 'NONE',  ( -66.43080436395490551, 203.5000000000000000, -0.1155267958017335561 ) ) ;
#13403 = CARTESIAN_POINT ( 'NONE',  ( 24.73960768102886121, -3.464101615138067469, 161.5861908599895003 ) ) ;
#13404 = CARTESIAN_POINT ( 'NONE',  ( -2.311890736173176641, 60.72268628210144925, -12.53471296425194836 ) ) ;
#13405 = CARTESIAN_POINT ( 'NONE',  ( 26.99999999999999289, 0.000000000000000000, -8.000000000000000000 ) ) ;
#13406 = CARTESIAN_POINT ( 'NONE',  ( 10.56230152254410548, 0.000000000000000000, -6.750000000000061284 ) ) ;
#13408 = CARTESIAN_POINT ( 'NONE',  ( 19.68408634441912142, -5.407089921784861808, -2.296874999385551064 ) ) ;
#13407 = CARTESIAN_POINT ( 'NONE',  ( -5.529263428287477744, 20.47268628210143859, 7.954856959092191815 ) ) ;
#13409 = CARTESIAN_POINT ( 'NONE',  ( -3.253724281355068545E-15, 198.6500000012290172, -27.00000000000000000 ) ) ;
#13410 = EDGE_CURVE ( 'NONE', #29886, #7355, #19921, .T. ) ;
#13411 = VERTEX_POINT ( 'NONE', #11164 ) ;
#13412 = CARTESIAN_POINT ( 'NONE',  ( 24.00000000000000000, -5.196152422706629359, -1.650000000000012568 ) ) ;
#13413 = CARTESIAN_POINT ( 'NONE',  ( 34.01542801315541453, -5.407089921784861808, 162.9485590723218422 ) ) ;
#13414 = CARTESIAN_POINT ( 'NONE',  ( 27.87526709119022783, 5.196152422706636465, 163.0058021847763712 ) ) ;
#13415 = CARTESIAN_POINT ( 'NONE',  ( 23.99999999999999645, 243.1000000000000227, -5.196152422706631135 ) ) ;
#13416 = CARTESIAN_POINT ( 'NONE',  ( 22.56230152254410015, 7.347880794884117764E-16, -2.812499998771006204 ) ) ;
#13417 = CARTESIAN_POINT ( 'NONE',  ( -2.311890736173448424, 87.27731371789856496, 12.53471296425189330 ) ) ;
#13418 = CARTESIAN_POINT ( 'NONE',  ( -4.944772684328673229, 84.58518628210146062, 11.48171059495397728 ) ) ;
#13419 = EDGE_LOOP ( 'NONE', ( #29394, #5164, #11944, #37187 ) ) ;
#13420 = EDGE_LOOP ( 'NONE', ( #5611, #9108, #9613, #31690 ) ) ;
#13421 = CARTESIAN_POINT ( 'NONE',  ( 5.727106289114498080E-15, 198.4250000012290229, 31.17691453623979214 ) ) ;
#13422 = CARTESIAN_POINT ( 'NONE',  ( 25.24946877610227958, -3.464101615137868073, 167.4139298438261676 ) ) ;
#13423 = CARTESIAN_POINT ( 'NONE',  ( -8.927990412390371944, 53.92731371789854222, -13.04141134922778988 ) ) ;
#13424 = CARTESIAN_POINT ( 'NONE',  ( 21.00000000000000000, -6.646953231504538984, -9.590624999385488181 ) ) ;
#13425 = CARTESIAN_POINT ( 'NONE',  ( 23.87821517812500005, 245.9593750006145569, 4.985214923628404016 ) ) ;
#13426 = CARTESIAN_POINT ( 'NONE',  ( -60.49330436395489130, 210.1155267958017703, -4.499999999999996447 ) ) ;
#13427 = CARTESIAN_POINT ( 'NONE',  ( 0.000000000000000000, 0.000000000000000000, 2.500000000000000000 ) ) ;
#13428 = CARTESIAN_POINT ( 'NONE',  ( -3.796722387233185003, 35.81481371789853796, -8.710071997420207879 ) ) ;
#13429 = CARTESIAN_POINT ( 'NONE',  ( 10.31873187879410914, 0.000000000000000000, -8.690624999385526905 ) ) ;
#13430 = CARTESIAN_POINT ( 'NONE',  ( 0.1745138560723095977, 96.18981371789855928, 9.500000000000005329 ) ) ;
#13431 = CARTESIAN_POINT ( 'NONE',  ( 13.62178482187501416, 197.7593750006145399, 23.59362340125806767 ) ) ;
#13432 = CARTESIAN_POINT ( 'NONE',  ( 4.622313124798831829, 9.364813717898545775, -11.61527771782809282 ) ) ;
#13433 =( BOUNDED_CURVE ( )  B_SPLINE_CURVE ( 2, ( #3730, #9798, #21189, #9615, #21376, #15492, #18155 ),
 .UNSPECIFIED., .F., .F. ) 
 B_SPLINE_CURVE_WITH_KNOTS ( ( 3, 2, 2, 3 ),
 ( 0.7391304347826078702, 0.7463768115942021053, 0.7536231884057964514, 0.7608695652173906865 ),
 .UNSPECIFIED. ) 
 CURVE ( )  GEOMETRIC_REPRESENTATION_ITEM ( )  RATIONAL_B_SPLINE_CURVE ( ( 1.000000000000014433, 0.8660254037844243857, 1.000000000000000000, 0.8660254037844387076, 1.000000000000000000, 0.8660254037844510311, 0.9999999999999876765 ) ) 
 REPRESENTATION_ITEM ( '' )  );
#13434 = EDGE_CURVE ( 'NONE', #33087, #31762, #24983, .T. ) ;
#13435 = CARTESIAN_POINT ( 'NONE',  ( -6.932735513423968321, 69.34768628210143504, -10.69584247140445221 ) ) ;
#13436 = CARTESIAN_POINT ( 'NONE',  ( 16.56230152254410015, -6.928203230275506996, -7.874999998770975118 ) ) ;
#13437 = CARTESIAN_POINT ( 'NONE',  ( 37.02731477413858130, 3.464101615138035051, 164.3507666672186929 ) ) ;
#13438 = CARTESIAN_POINT ( 'NONE',  ( 27.63710252976279591, -5.407089921784859143, 161.6808929148651828 ) ) ;
#13439 = CARTESIAN_POINT ( 'NONE',  ( 26.99999999999999645, 3.464101615137755275, -1.031249998770967347 ) ) ;
#13440 = VECTOR ( 'NONE', #8454, 1000.000000000000000 ) ;
#13441 = CARTESIAN_POINT ( 'NONE',  ( 16.56230152254411436, -7.209453229046482114, -7.284374999385498484 ) ) ;
#13442 = CARTESIAN_POINT ( 'NONE',  ( 10.56230152254410903, 0.000000000000000000, -1.800000000000051559 ) ) ;
#13443 = LINE ( 'NONE', #33717, #3014 ) ;
#13444 = CARTESIAN_POINT ( 'NONE',  ( -9.500000000000005329, 95.51018628210147199, -0.1745138560725176813 ) ) ;
#13445 = DIRECTION ( 'NONE',  ( -0.000000000000000000, -0.000000000000000000, -1.000000000000000000 ) ) ;
#13446 = EDGE_CURVE ( 'NONE', #21774, #25338, #6219, .T. ) ;
#13447 = CARTESIAN_POINT ( 'NONE',  ( 10.49813415415989581, 119.3726862821014549, 7.228626920339068285 ) ) ;
#13448 = CARTESIAN_POINT ( 'NONE',  ( 19.56230152254411792, 5.196152422706637353, -3.300000000000025135 ) ) ;
#13449 = DIRECTION ( 'NONE',  ( 0.000000000000000000, 0.000000000000000000, -1.000000000000000000 ) ) ;
#13450 = ORIENTED_EDGE ( 'NONE', *, *, #5092, .F. ) ;
#13451 = CARTESIAN_POINT ( 'NONE',  ( 24.79193261022362549, 3.604726614523236616, 164.9789157851677146 ) ) ;
#13452 = CARTESIAN_POINT ( 'NONE',  ( 26.75643035624999655, 7.049594010296217766E-16, -5.315624999385482496 ) ) ;
#13453 = CARTESIAN_POINT ( 'NONE',  ( 13.62178482187501416, 196.8593750006145342, 23.59362340125806767 ) ) ;
#13454 = FACE_BOUND ( 'NONE', #4038, .T. ) ;
#13455 = CARTESIAN_POINT ( 'NONE',  ( 31.31161381383153497, -6.928203230275514990, 167.8622852179797462 ) ) ;
#13456 = FACE_OUTER_BOUND ( 'NONE', #31538, .T. ) ;
#13457 = CARTESIAN_POINT ( 'NONE',  ( 26.75643035624999655, 243.7468750006145228, 3.323476615752267715 ) ) ;
#13458 = CARTESIAN_POINT ( 'NONE',  ( 29.49486714975617474, 6.148716665048037378, 159.5363409456820136 ) ) ;
#13459 = CARTESIAN_POINT ( 'NONE',  ( 2.660918448318002838, 141.9023137178985792, 12.46528703574811558 ) ) ;
#13460 = CARTESIAN_POINT ( 'NONE',  ( -27.24356964375000345, 194.9093750006145456, 0.000000000000000000 ) ) ;
#13462 = ORIENTED_EDGE ( 'NONE', *, *, #3572, .F. ) ;
#13461 = ORIENTED_EDGE ( 'NONE', *, *, #17015, .T. ) ;
#13463 = CARTESIAN_POINT ( 'NONE',  ( 15.24356964375000167, 244.3843750006145115, 3.323476615752272600 ) ) ;
#13464 = CARTESIAN_POINT ( 'NONE',  ( 6.932735513424201024, 9.652313717898541867, -10.69584247140429412 ) ) ;
#13465 = CARTESIAN_POINT ( 'NONE',  ( 23.87821517812500005, -4.985214923628404016, -4.040624999385455496 ) ) ;
#13466 = CARTESIAN_POINT ( 'NONE',  ( 5.770363421894130873, 119.7648137178985905, -14.38691631536193860 ) ) ;
#13467 = CARTESIAN_POINT ( 'NONE',  ( 26.99999999999999645, 244.3374999999999773, 3.464101615137751278 ) ) ;
#13468 = CARTESIAN_POINT ( 'NONE',  ( 15.00000000000000178, -3.464101615137757051, -10.25624999877095966 ) ) ;
#13469 = CARTESIAN_POINT ( 'NONE',  ( 10.31873187879410736, 0.000000000000000000, -7.846874999385494931 ) ) ;
#13470 = ORIENTED_EDGE ( 'NONE', *, *, #4155, .F. ) ;
#13471 = CARTESIAN_POINT ( 'NONE',  ( 27.00000000000000355, 198.9875000012290229, -3.306546357697854128E-15 ) ) ;
#13472 = CARTESIAN_POINT ( 'NONE',  ( 0.1745138560725515708, 116.2101862821014606, -12.50000000000000355 ) ) ;
#13473 = CARTESIAN_POINT ( 'NONE',  ( 22.80587116629410716, 7.646167579472015790E-16, -1.265624999385539518 ) ) ;
#13474 = CARTESIAN_POINT ( 'NONE',  ( -37.92336230271182984, 217.4189793300686233, 4.149950860017807663 ) ) ;
#13475 = CARTESIAN_POINT ( 'NONE',  ( 20.99999999999999645, 243.3343750006145285, -6.646953231504538984 ) ) ;
#13476 = CARTESIAN_POINT ( 'NONE',  ( -13.49999999999998401, 197.4875000012290229, 23.38268590217985476 ) ) ;
#13477 = CARTESIAN_POINT ( 'NONE',  ( -65.23586230271183695, 206.8500491399821328, 5.686928522499748340 ) ) ;
#13478 = CARTESIAN_POINT ( 'NONE',  ( 0.1745138560725515708, 134.6101862821014663, -12.50000000000000355 ) ) ;
#13479 = CARTESIAN_POINT ( 'NONE',  ( 16.56230152254411081, -6.928203230275506996, -1.574999998771003495 ) ) ;
#13480 = ORIENTED_EDGE ( 'NONE', *, *, #3812, .F. ) ;
#13481 = DIRECTION ( 'NONE',  ( 0.000000000000000000, 1.000000000000000000, 0.000000000000000000 ) ) ;
#13482 = CARTESIAN_POINT ( 'NONE',  ( -15.50000000000000533, 123.1101862821014663, -0.1745138560725808530 ) ) ;
#13483 = CARTESIAN_POINT ( 'NONE',  ( 27.00000000000000355, 199.3249999999999886, -3.306546357697854128E-15 ) ) ;
#13484 = CARTESIAN_POINT ( 'NONE',  ( -10.49813415415989581, 4.372686282101440725, -7.228626920339068285 ) ) ;
#13485 = CARTESIAN_POINT ( 'NONE',  ( 10.56230152254410726, 0.000000000000000000, -9.900000000000048317 ) ) ;
#13486 = ORIENTED_EDGE ( 'NONE', *, *, #24306, .T. ) ;
#13487 = CARTESIAN_POINT ( 'NONE',  ( -89.83814373643217266, 60.44923248139874516, -5.000000000000000000 ) ) ;
#13488 = CARTESIAN_POINT ( 'NONE',  ( -9.500000000000005329, 77.11018628210145209, -0.1745138560725176813 ) ) ;
#13489 = CARTESIAN_POINT ( 'NONE',  ( 13.56230152254410548, 5.196152422706630247, -2.212499998771017218 ) ) ;
#13490 = CARTESIAN_POINT ( 'NONE',  ( 8.710071997420211432, 130.1148137178985564, -3.796722387233181895 ) ) ;
#13491 = CARTESIAN_POINT ( 'NONE',  ( -27.24356964374999990, 197.0656250006145171, -15.72908226750537786 ) ) ;
#13492 = DIRECTION ( 'NONE',  ( 1.000000000000000000, 0.000000000000000000, 0.000000000000000000 ) ) ;
#13493 = CARTESIAN_POINT ( 'NONE',  ( -1.926257025242585782E-15, 198.8468750006145740, -31.45816453501075927 ) ) ;
#13494 = CARTESIAN_POINT ( 'NONE',  ( 15.00000000000000000, 0.000000000000000000, -1.743749998770943721 ) ) ;
#13495 = DIRECTION ( 'NONE',  ( 0.08715574274765150453, 0.000000000000000000, 0.9961946980917461003 ) ) ;
#13496 =( BOUNDED_CURVE ( )  B_SPLINE_CURVE ( 2, ( #17423, #342, #23294, #31444, #28404, #25567, #17614 ),
 .UNSPECIFIED., .F., .F. ) 
 B_SPLINE_CURVE_WITH_KNOTS ( ( 3, 2, 2, 3 ),
 ( 0.8695652173913026584, 0.8768115942028961163, 0.8840579710144895742, 0.8913043478260829211 ),
 .UNSPECIFIED. ) 
 CURVE ( )  GEOMETRIC_REPRESENTATION_ITEM ( )  RATIONAL_B_SPLINE_CURVE ( ( 1.000000000000030864, 0.8660254037844079544, 1.000000000000000000, 0.8660254037844387076, 1.000000000000000000, 0.8660254037845126485, 0.9999999999999260591 ) ) 
 REPRESENTATION_ITEM ( '' )  );
#13497 = CARTESIAN_POINT ( 'NONE',  ( -9.534712964251895073, 61.97731371789853938, -1.715153634034446428 ) ) ;
#13498 = VERTEX_POINT ( 'NONE', #12280 ) ;
#13499 = CIRCLE ( 'NONE', #18441, 5.999999999999999112 ) ;
#13500 = CARTESIAN_POINT ( 'NONE',  ( 18.00000000000000355, 242.0312500012290400, 5.196152422706632912 ) ) ;
#13501 = CARTESIAN_POINT ( 'NONE',  ( 12.53471296425189330, 66.57731371789856212, 2.311890736173451533 ) ) ;
#13502 = CARTESIAN_POINT ( 'NONE',  ( 10.31873187879411091, 3.604726614523240613, -6.534374999385494043 ) ) ;
#13503 = CARTESIAN_POINT ( 'NONE',  ( 5.778771075727756162E-15, 198.5656250006145171, 31.45816453501075927 ) ) ;
#13504 = CARTESIAN_POINT ( 'NONE',  ( 15.24356964374999990, 3.323476615752268604, -7.040624999385501681 ) ) ;
#13505 = CARTESIAN_POINT ( 'NONE',  ( -11.61527771782809282, 34.66481371789854649, -4.622313124798832717 ) ) ;
#13506 = AXIS2_PLACEMENT_3D ( 'NONE', #12277, #18355, #29904 ) ;
#13507 = EDGE_LOOP ( 'NONE', ( #15171, #32913, #21591, #27413 ) ) ;
#13508 = UNCERTAINTY_MEASURE_WITH_UNIT (LENGTH_MEASURE( 1.000000000000000082E-05 ), #28887, 'distance_accuracy_value', 'NONE');
#13509 = CARTESIAN_POINT ( 'NONE',  ( 19.68408634441911076, 5.407089921784862696, -2.146874999385511629 ) ) ;
#13510 = DIRECTION ( 'NONE',  ( -0.000000000000000000, -0.000000000000000000, 1.000000000000000000 ) ) ;
#13511 = EDGE_CURVE ( 'NONE', #3008, #2146, #27652, .T. ) ;
#13512 = CARTESIAN_POINT ( 'NONE',  ( 31.41211527974097706, -7.209453229046482114, 169.0110222298289671 ) ) ;
#13513 = CARTESIAN_POINT ( 'NONE',  ( -54.74627896937848703, 203.4690446883607535, -1.626142955000504209 ) ) ;
#13514 = APPLICATION_PROTOCOL_DEFINITION ( 'draft international standard', 'automotive_design', 1998, #9320 ) ;
#13515 = DIRECTION ( 'NONE',  ( -0.000000000000000000, 0.000000000000000000, -1.000000000000000000 ) ) ;
#13516 = CARTESIAN_POINT ( 'NONE',  ( -10.49813415416004858, 60.82731371789855501, 7.228626920338839135 ) ) ;
#13517 = CARTESIAN_POINT ( 'NONE',  ( -66.81919563604516554, 214.5000000000000284, -0.1155267958017627827 ) ) ;
#13518 = CARTESIAN_POINT ( 'NONE',  ( -62.67038769728823411, 208.1428034533959703, 6.469044688360770401 ) ) ;
#13519 = CARTESIAN_POINT ( 'NONE',  ( 23.99999999999999645, 5.196152422706631135, -6.899999999999989697 ) ) ;
#13520 = CARTESIAN_POINT ( 'NONE',  ( -14.50000000000000000, 215.7563705986615901, -5.555555555555558023 ) ) ;
#13521 = CARTESIAN_POINT ( 'NONE',  ( 5.770363421894130873, 46.16481371789854649, -14.38691631536193860 ) ) ;
#13522 = CARTESIAN_POINT ( 'NONE',  ( -34.95461230271183695, 207.6069050685336492, -8.469044688360751749 ) ) ;
#13523 =( GEOMETRIC_REPRESENTATION_CONTEXT ( 3 ) GLOBAL_UNCERTAINTY_ASSIGNED_CONTEXT ( ( #27908 ) ) GLOBAL_UNIT_ASSIGNED_CONTEXT ( ( #34024, #30449, #8618 ) ) REPRESENTATION_CONTEXT ( 'NONE', 'WORKASPACE' ) );
#13524 = CARTESIAN_POINT ( 'NONE',  ( 0.1745138560725515708, 33.41018628210144925, -12.50000000000000355 ) ) ;
#13525 = CARTESIAN_POINT ( 'NONE',  ( 21.00000000000000355, 0.000000000000000000, 50.00000000000001421 ) ) ;
#13526 = CARTESIAN_POINT ( 'NONE',  ( -11.48171059495397373, 59.28518628210144215, -4.944772684328680334 ) ) ;
#13527 = CARTESIAN_POINT ( 'NONE',  ( -14.25334919248782306, 13.28518628210143149, -6.092822981423979378 ) ) ;
#13528 = ADVANCED_FACE ( 'NONE', ( #6408 ), #26871, .F. ) ;
#13529 = CARTESIAN_POINT ( 'NONE',  ( 10.56230152254410548, 3.464101615137757051, -2.737500000000003375 ) ) ;
#13530 = CARTESIAN_POINT ( 'NONE',  ( -26.99999999999999645, 197.4500000012290002, 15.58845726811991561 ) ) ;
#13531 = EDGE_LOOP ( 'NONE', ( #20706, #28086, #22199, #20132 ) ) ;
#13532 = CARTESIAN_POINT ( 'NONE',  ( -0.1745138560725817967, 28.81018628210143717, 15.50000000000000533 ) ) ;
#13533 = CARTESIAN_POINT ( 'NONE',  ( 13.62178482187499640, 195.6031250006145115, -23.59362340125807123 ) ) ;
#13534 = CARTESIAN_POINT ( 'NONE',  ( 13.62178482187501416, 198.6593750006145456, 23.59362340125806767 ) ) ;
#13535 = CARTESIAN_POINT ( 'NONE',  ( 0.000000000000000000, 200.0000000000000000, 0.000000000000000000 ) ) ;
#13536 = CARTESIAN_POINT ( 'NONE',  ( 27.00000000000000355, 195.3875000012290286, -3.306546357697854128E-15 ) ) ;
#13537 = DIRECTION ( 'NONE',  ( 0.000000000000000000, -1.000000000000000000, 0.000000000000000000 ) ) ;
#13538 = EDGE_CURVE ( 'NONE', #24506, #17676, #20131, .T. ) ;
#13539 = CARTESIAN_POINT ( 'NONE',  ( 12.50000000000000355, 8.110186282101444988, 0.1745138560725507937 ) ) ;
#13540 = VECTOR ( 'NONE', #27934, 1000.000000000000000 ) ;
#13541 = CARTESIAN_POINT ( 'NONE',  ( 26.75643035624999655, 248.7343750006145342, -7.049594010296217766E-16 ) ) ;
#13542 = CARTESIAN_POINT ( 'NONE',  ( -2.064181346179062349, 109.7023137178985479, -9.465287035748106703 ) ) ;
#13543 = CARTESIAN_POINT ( 'NONE',  ( 20.99999999999999645, 242.9968750006145513, -6.646953231504538984 ) ) ;
#13544 = EDGE_LOOP ( 'NONE', ( #34434, #13183, #23862, #5719 ) ) ;
#13545 = FILL_AREA_STYLE ('',( #7302 ) ) ;
#13546 = CARTESIAN_POINT ( 'NONE',  ( 15.00000000000000000, 248.2187500012290684, -3.464101615137752166 ) ) ;
#13547 = CARTESIAN_POINT ( 'NONE',  ( 10.69584247140429589, 113.1523137178985650, 6.932735513424201024 ) ) ;
#13548 = CARTESIAN_POINT ( 'NONE',  ( 19.83830452692373925, 6.917534487978453051, -10.19247752355789416 ) ) ;
#13549 = CARTESIAN_POINT ( 'NONE',  ( 33.99418380086066804, 5.407089921784857367, 162.7057366146619586 ) ) ;
#13550 = CARTESIAN_POINT ( 'NONE',  ( 26.75643035624999655, -3.323476615752267715, -0.5156249993854836733 ) ) ;
#13551 = CARTESIAN_POINT ( 'NONE',  ( -1.909035429704832693E-15, 196.7374999999999829, -31.17691453623979214 ) ) ;
#13552 = ORIENTED_EDGE ( 'NONE', *, *, #18146, .F. ) ;
#13553 = CARTESIAN_POINT ( 'NONE',  ( 12.50000000000000355, 26.51018628210144357, 0.1745138560725507937 ) ) ;
#13554 = ORIENTED_EDGE ( 'NONE', *, *, #2188, .T. ) ;
#13555 = VERTEX_POINT ( 'NONE', #23662 ) ;
#13556 = CARTESIAN_POINT ( 'NONE',  ( 26.99999999999999645, 3.464101615137755275, -4.181249998770937282 ) ) ;
#13558 = AXIS2_PLACEMENT_3D ( 'NONE', #17446, #14409, #14971 ) ;
#13557 = CARTESIAN_POINT ( 'NONE',  ( 18.12178482187500350, -4.985214923628407568, -0.9656249993854615354 ) ) ;
#13559 = CARTESIAN_POINT ( 'NONE',  ( 17.48528137423856066, 206.4852813742385820, -5.999999999999995559 ) ) ;
#13560 = LINE ( 'NONE', #22099, #10550 ) ;
#13561 = CARTESIAN_POINT ( 'NONE',  ( 26.75643035624999655, 248.6593750006145171, -3.323476615752271712 ) ) ;
#13562 = CARTESIAN_POINT ( 'NONE',  ( 6.932735513423970097, 64.74768628210145494, 10.69584247140445044 ) ) ;
#13563 = CARTESIAN_POINT ( 'NONE',  ( -2.908627838312119351, 134.3226862821014436, -15.53471296425195369 ) ) ;
#13564 = CIRCLE ( 'NONE', #36544, 7.500000000000000000 ) ;
#13565 = CARTESIAN_POINT ( 'NONE',  ( -60.88169563604516554, 210.1155267958017703, 6.500000000000000888 ) ) ;
#13566 = CARTESIAN_POINT ( 'NONE',  ( 15.00000000000045119, 215.9999999999999716, 0.1308996912579823979 ) ) ;
#13567 = CARTESIAN_POINT ( 'NONE',  ( -59.89211230271182274, 205.5309553116392465, 1.321298161741817356 ) ) ;
#13568 = CARTESIAN_POINT ( 'NONE',  ( 7.234628195640322446, 196.9825961894323427, 26.99999999999999645 ) ) ;
#13569 = CARTESIAN_POINT ( 'NONE',  ( 27.92429219659289785, 5.196152422706630247, 163.5661617036773237 ) ) ;
#13570 = CARTESIAN_POINT ( 'NONE',  ( -12.50000000000000355, 126.0898137178985650, 0.1745138560722786503 ) ) ;
#13571 = EDGE_CURVE ( 'NONE', #8055, #26185, #28847, .T. ) ;
#13572 = CARTESIAN_POINT ( 'NONE',  ( -38.32663769728824121, 204.3130714775002730, 3.149950860017883603 ) ) ;
#13573 = CARTESIAN_POINT ( 'NONE',  ( -57.92038769728823411, 207.6069050685337913, 8.469044688360781947 ) ) ;
#13574 = CARTESIAN_POINT ( 'NONE',  ( 20.99999999999999645, -6.646953231504538984, -1.040624999385473481 ) ) ;
#13575 = CARTESIAN_POINT ( 'NONE',  ( -27.24356964375000345, 196.6531250006145513, 0.000000000000000000 ) ) ;
#13576 = CARTESIAN_POINT ( 'NONE',  ( 15.53471296425188797, 94.17731371789857064, 2.908627838312457747 ) ) ;
#13577 = CARTESIAN_POINT ( 'NONE',  ( -67.80877896937849414, 212.1620413398627534, -8.530955311639255356 ) ) ;
#13578 = EDGE_CURVE ( 'NONE', #21882, #6071, #14942, .T. ) ;
#13579 = VERTEX_POINT ( 'NONE', #21019 ) ;
#13580 = DIRECTION ( 'NONE',  ( -0.9925324990730152175, 0.1219804832088933616, 0.000000000000000000 ) ) ;
#13581 = CARTESIAN_POINT ( 'NONE',  ( 0.1745138560725515708, 116.2101862821014606, -12.50000000000000355 ) ) ;
#13582 = CARTESIAN_POINT ( 'NONE',  ( 15.50000000000000533, 72.51018628210145778, 0.1745138560725827404 ) ) ;
#13583 = DIRECTION ( 'NONE',  ( 1.000000000000000000, 0.000000000000000000, 0.000000000000000000 ) ) ;
#13584 = CARTESIAN_POINT ( 'NONE',  ( 24.71512661192725702, -3.604726614523244610, 164.1010192074743657 ) ) ;
#13585 = AXIS2_PLACEMENT_3D ( 'NONE', #21706, #18495, #33256 ) ;
#13586 = CARTESIAN_POINT ( 'NONE',  ( 0.1745138560725837118, 79.41018628210144925, -15.50000000000000533 ) ) ;
#13587 = AXIS2_PLACEMENT_3D ( 'NONE', #20057, #20616, #31783 ) ;
#13588 = CARTESIAN_POINT ( 'NONE',  ( -47.23288769728823411, 203.5309553116391896, -1.857196546604028997 ) ) ;
#13589 = EDGE_CURVE ( 'NONE', #29332, #31166, #22996, .T. ) ;
#13590 = VECTOR ( 'NONE', #35076, 1000.000000000000000 ) ;
#13591 = CARTESIAN_POINT ( 'NONE',  ( 19.68408634441910721, -5.407089921784855591, -7.190624999385525129 ) ) ;
#13592 = CARTESIAN_POINT ( 'NONE',  ( -9.534712964251941258, 21.62268628210143717, 1.715153634034234154 ) ) ;
#13593 = CARTESIAN_POINT ( 'NONE',  ( 27.00000000000047251, -3.464101615137475942, -3.412500000000007194 ) ) ;
#13594 = CARTESIAN_POINT ( 'NONE',  ( -64.64955436395490551, 214.8429017333601792, -4.673758765035196383 ) ) ;
#13595 = CARTESIAN_POINT ( 'NONE',  ( 0.3500000000000065281, 244.5000000000000000, 5.000000000000000000 ) ) ;
#13596 = CARTESIAN_POINT ( 'NONE',  ( -4.622313124798576922, 51.23518628210143788, -11.61527771782819762 ) ) ;
#13597 = CARTESIAN_POINT ( 'NONE',  ( -27.00000000000000355, 198.6500000000000341, 0.000000000000000000 ) ) ;
#13598 = CARTESIAN_POINT ( 'NONE',  ( 13.50000000000001421, 197.5625000012290400, 23.38268590217984055 ) ) ;
#13600 = CARTESIAN_POINT ( 'NONE',  ( 22.80587116629411426, -3.604726614523238837, -1.809374999385491511 ) ) ;
#13599 = CARTESIAN_POINT ( 'NONE',  ( -6.594114490232312775, 23.06018628210144783, -6.840914352312096547 ) ) ;
#13601 = CARTESIAN_POINT ( 'NONE',  ( 7.234628195640322446, 198.4450961906613600, 26.99999999999999645 ) ) ;
#13602 = ORIENTED_EDGE ( 'NONE', *, *, #17246, .F. ) ;
#13603 = CARTESIAN_POINT ( 'NONE',  ( 26.99999999999999645, 7.347880794884117764E-16, -1.124999999999987121 ) ) ;
#13604 = CARTESIAN_POINT ( 'NONE',  ( 23.73600959472706506, -5.270316205469181448, -7.999999999999998224 ) ) ;
#13605 = CARTESIAN_POINT ( 'NONE',  ( 24.43731768191911513, 0.000000000000000000, 160.9256486073069539 ) ) ;
#13606 = CARTESIAN_POINT ( 'NONE',  ( 10.31873187879411269, -3.604726614523240613, -1.003124999385540450 ) ) ;
#13607 = CARTESIAN_POINT ( 'NONE',  ( 27.84912036836594140, -5.196152422706638241, 162.7069437753488046 ) ) ;
#13608 =( BOUNDED_CURVE ( )  B_SPLINE_CURVE ( 2, ( #22962, #11573, #31480, #34509, #14241, #17089, #5505 ),
 .UNSPECIFIED., .F., .F. ) 
 B_SPLINE_CURVE_WITH_KNOTS ( ( 3, 2, 2, 3 ),
 ( 0.4782608695652184050, 0.4855072463768126956, 0.4927536231884070417, 0.5000000000000013323 ),
 .UNSPECIFIED. ) 
 CURVE ( )  GEOMETRIC_REPRESENTATION_ITEM ( )  RATIONAL_B_SPLINE_CURVE ( ( 0.9999999999999815703, 0.8660254037844571373, 1.000000000000000000, 0.8660254037844387076, 1.000000000000000000, 0.8660254037844140607, 1.000000000000024647 ) ) 
 REPRESENTATION_ITEM ( '' )  );
#13609 = CARTESIAN_POINT ( 'NONE',  ( 23.99999999999999645, 242.6500000000000057, -5.196152422706631135 ) ) ;
#13610 = CARTESIAN_POINT ( 'NONE',  ( 10.56230152254377153, 3.464101615137553658, -3.974999998771030274 ) ) ;
#13611 = EDGE_CURVE ( 'NONE', #37310, #19674, #3172, .T. ) ;
#13612 = CARTESIAN_POINT ( 'NONE',  ( -6.932735513424201912, 87.85231371789855359, 10.69584247140429412 ) ) ;
#13613 = CARTESIAN_POINT ( 'NONE',  ( -8.962234695871760692, 94.36018628210145209, 8.715434833791933400 ) ) ;
#13614 = EDGE_LOOP ( 'NONE', ( #20061, #17519, #32892, #4125 ) ) ;
#13615 = VERTEX_POINT ( 'NONE', #29526 ) ;
#13616 = CARTESIAN_POINT ( 'NONE',  ( 13.50000000000001421, 197.5625000012290400, 23.38268590217984055 ) ) ;
#13617 = CARTESIAN_POINT ( 'NONE',  ( -27.24356964375000345, 199.8031250006145285, 0.000000000000000000 ) ) ;
#13618 = CARTESIAN_POINT ( 'NONE',  ( -6.092822981423666739, 54.21481371789855785, -14.25334919248795096 ) ) ;
#13619 = CARTESIAN_POINT ( 'NONE',  ( 23.87821517812499650, 4.985214923628404904, -9.853124999385482141 ) ) ;
#13620 = CARTESIAN_POINT ( 'NONE',  ( 26.75643035624999655, 243.7468750006145228, 3.323476615752267715 ) ) ;
#13621 = CARTESIAN_POINT ( 'NONE',  ( -54.75372103062156270, 214.5309553116392749, -1.090244570138262148 ) ) ;
#13622 = DIRECTION ( 'NONE',  ( -0.000000000000000000, -1.000000000000000000, -0.000000000000000000 ) ) ;
#13623 = EDGE_CURVE ( 'NONE', #16919, #20032, #3565, .T. ) ;
#13624 = CARTESIAN_POINT ( 'NONE',  ( 9.534712964251900402, 38.97731371789853938, 1.715153634034445540 ) ) ;
#13625 = CARTESIAN_POINT ( 'NONE',  ( 12.11180837762981533, -4.639959813803625543, -9.981585920767699349 ) ) ;
#13626 = CARTESIAN_POINT ( 'NONE',  ( 9.534712964251900402, 94.17731371789857064, 1.715153634034445540 ) ) ;
#13627 = CARTESIAN_POINT ( 'NONE',  ( -27.24356964374999635, 198.9968750006145228, 15.72908226750539384 ) ) ;
#13628 = CARTESIAN_POINT ( 'NONE',  ( 8.715434833792128799, 9.939813717898537959, -8.962234695871567070 ) ) ;
#13629 = B_SPLINE_CURVE_WITH_KNOTS ( 'NONE', 3,
 ( #34868, #8541, #8910, #20107 ),
 .UNSPECIFIED., .F., .F.,
 ( 4, 4 ),
 ( 0.000000000000000000, 1.000000000000000000 ),
 .UNSPECIFIED. ) ;
#13630 = CARTESIAN_POINT ( 'NONE',  ( 4.622313124798573369, 55.83518628210144641, 11.61527771782819940 ) ) ;
#13631 = CARTESIAN_POINT ( 'NONE',  ( 22.56230152254410726, 7.347880794884117764E-16, -9.562499998771039955 ) ) ;
#13632 = DIRECTION ( 'NONE',  ( 4.818676322157800087E-17, -1.000000000000000000, 5.329070518200755338E-15 ) ) ;
#13633 = CARTESIAN_POINT ( 'NONE',  ( 37.09428426793671463, -3.604726614523235284, 162.3215832362777746 ) ) ;
#13634 = EDGE_CURVE ( 'NONE', #15181, #17150, #37022, .T. ) ;
#13635 = CARTESIAN_POINT ( 'NONE',  ( 22.80587116629411781, 7.646167579472024665E-16, -9.871874999385521932 ) ) ;
#13636 = CARTESIAN_POINT ( 'NONE',  ( 16.56230152254411436, 7.209453229046482114, -7.509374999385480365 ) ) ;
#13637 = CARTESIAN_POINT ( 'NONE',  ( 24.74287602148785581, 3.464101615137384904, 161.6235481623923249 ) ) ;
#13638 = CARTESIAN_POINT ( 'NONE',  ( -0.1745138560725182642, 102.4101862821014493, 9.500000000000005329 ) ) ;
#13639 = CARTESIAN_POINT ( 'NONE',  ( -6.932735513423968321, 115.3476862821014635, -10.69584247140445221 ) ) ;
#13640 = CARTESIAN_POINT ( 'NONE',  ( 20.99999999999999645, 249.6625000000000512, 5.999999999999998224 ) ) ;
#13641 = ORIENTED_EDGE ( 'NONE', *, *, #16190, .T. ) ;
#13642 = CARTESIAN_POINT ( 'NONE',  ( 34.13799077639428958, -5.407089921784855591, 164.3494578665133474 ) ) ;
#13643 = CARTESIAN_POINT ( 'NONE',  ( 18.12178482187499640, 4.985214923628404904, -5.615624999385476990 ) ) ;
#13644 = CARTESIAN_POINT ( 'NONE',  ( -13.62178482187500528, 197.9843750006145626, -23.59362340125807123 ) ) ;
#13645 = CARTESIAN_POINT ( 'NONE',  ( 16.07192114941521766, -3.422577806627481234, -8.000000000000001776 ) ) ;
#13646 = CARTESIAN_POINT ( 'NONE',  ( 28.42434827050043467, 5.196152422706636465, 169.2818287827543600 ) ) ;
#13647 = DIRECTION ( 'NONE',  ( 0.000000000000000000, 1.000000000000000000, 0.000000000000000000 ) ) ;
#13648 = CARTESIAN_POINT ( 'NONE',  ( 21.00000000000000000, 249.6625000000000227, 6.928203230275506996 ) ) ;
#13649 = CARTESIAN_POINT ( 'NONE',  ( 22.56230152254400068, -3.464101615137812562, -6.899999998771023435 ) ) ;
#13650 = VECTOR ( 'NONE', #8141, 1000.000000000000114 ) ;
#13651 = CARTESIAN_POINT ( 'NONE',  ( 10.69584247140429589, 140.7523137178985735, 6.932735513424201024 ) ) ;
#13652 = CARTESIAN_POINT ( 'NONE',  ( 11.48171059495397728, 137.4851862821014663, 4.944772684328674117 ) ) ;
#13654 = ORIENTED_EDGE ( 'NONE', *, *, #28096, .T. ) ;
#13653 = ORIENTED_EDGE ( 'NONE', *, *, #33199, .T. ) ;
#13655 = CARTESIAN_POINT ( 'NONE',  ( 26.75643035624999655, 244.5718750006145115, -7.049594010296217766E-16 ) ) ;
#13656 = CARTESIAN_POINT ( 'NONE',  ( 16.56230152254410726, 0.000000000000000000, -10.00000000000000000 ) ) ;
#13657 = ADVANCED_FACE ( 'NONE', ( #34001 ), #2158, .F. ) ;
#13658 = CARTESIAN_POINT ( 'NONE',  ( 18.12178482187499640, 4.985214923628404904, -4.715624999385465088 ) ) ;
#13659 = CARTESIAN_POINT ( 'NONE',  ( -10.83675517735179028, 115.7398137178985564, 11.08355503943118947 ) ) ;
#13660 = EDGE_CURVE ( 'NONE', #36103, #9886, #7861, .T. ) ;
#13661 = CARTESIAN_POINT ( 'NONE',  ( 24.85399959338462139, 0.000000000000000000, 162.8936964012349051 ) ) ;
#13662 = CARTESIAN_POINT ( 'NONE',  ( 21.00000000000000000, 6.646953231504538984, -2.165624999385510563 ) ) ;
#13663 = CARTESIAN_POINT ( 'NONE',  ( 19.68408634441912142, -5.407089921784861808, -7.696874999385511451 ) ) ;
#13664 =( BOUNDED_CURVE ( )  B_SPLINE_CURVE ( 2, ( #14191, #28764, #11343, #5642, #11708, #14934, #11526 ),
 .UNSPECIFIED., .F., .F. ) 
 B_SPLINE_CURVE_WITH_KNOTS ( ( 3, 2, 2, 3 ),
 ( 0.06521739130435129372, 0.07246376811594562595, 0.07971014492753994429, 0.08695652173913427652 ),
 .UNSPECIFIED. ) 
 CURVE ( )  GEOMETRIC_REPRESENTATION_ITEM ( )  RATIONAL_B_SPLINE_CURVE ( ( 0.9999999999999359401, 0.8660254037845028785, 1.000000000000000000, 0.8660254037844387076, 1.000000000000000000, 0.8660254037843676533, 1.000000000000071054 ) ) 
 REPRESENTATION_ITEM ( '' )  );
#13665 = ORIENTED_EDGE ( 'NONE', *, *, #9024, .F. ) ;
#13666 = CARTESIAN_POINT ( 'NONE',  ( -26.99999999999998934, 197.9000000012290172, 15.58845726811991561 ) ) ;
#13667 = CARTESIAN_POINT ( 'NONE',  ( -12.53471296425194836, 122.8226862821014720, 2.311890736173176641 ) ) ;
#13668 = DIRECTION ( 'NONE',  ( -0.5887012860850802110, 0.8083506638593009885, 0.000000000000000000 ) ) ;
#13669 = EDGE_CURVE ( 'NONE', #15843, #29332, #1468, .T. ) ;
#13670 = CARTESIAN_POINT ( 'NONE',  ( -39.70461230271183695, 207.6069050685336492, -8.469044688360751749 ) ) ;
#13671 = CARTESIAN_POINT ( 'NONE',  ( 26.75643035624999655, 245.0593750006144944, -3.323476615752271268 ) ) ;
#13672 = VECTOR ( 'NONE', #34605, 1000.000000000000000 ) ;
#13673 = PRODUCT_DEFINITION ( 'UNKNOWN', '', #15999, #24042 ) ;
#13674 = CARTESIAN_POINT ( 'NONE',  ( -7.234628195640316228, 197.3200961906614168, -27.00000000000000000 ) ) ;
#13675 = CARTESIAN_POINT ( 'NONE',  ( -31.98586230271182984, 207.8500491399821613, 3.954877714930852495 ) ) ;
#13676 = CARTESIAN_POINT ( 'NONE',  ( -2.311890736173176641, 115.9226862821014521, -12.53471296425194836 ) ) ;
#13677 = CARTESIAN_POINT ( 'NONE',  ( 16.56230152254411081, 6.928203230275506996, -1.799999998770985377 ) ) ;
#13678 = VECTOR ( 'NONE', #1616, 1000.000000000000000 ) ;
#13679 = CARTESIAN_POINT ( 'NONE',  ( -37.53497103062156981, 204.4285982733020148, -3.350049139982115509 ) ) ;
#13680 = CARTESIAN_POINT ( 'NONE',  ( 1.069080835302379631E-14, 195.2750000012290457, 27.00000000000000000 ) ) ;
#13681 = CARTESIAN_POINT ( 'NONE',  ( 21.00000000000000355, 0.000000000000000000, 50.00000000000001421 ) ) ;
#13682 = CARTESIAN_POINT ( 'NONE',  ( -10.83675517735155047, 115.0601862821014691, -11.08355503943142750 ) ) ;
#13683 = CARTESIAN_POINT ( 'NONE',  ( -4.694659320240884604E-14, 197.8625000000000114, 27.00000000000000000 ) ) ;
#13684 = CARTESIAN_POINT ( 'NONE',  ( -11.61527771782819940, 12.13518628210144534, 4.622313124798574258 ) ) ;
#13685 = CARTESIAN_POINT ( 'NONE',  ( 19.56230152254411792, 5.196152422706637353, -8.250000000000062172 ) ) ;
#13686 = ORIENTED_EDGE ( 'NONE', *, *, #22429, .T. ) ;
#13687 = DIRECTION ( 'NONE',  ( -0.000000000000000000, 1.000000000000000000, -0.000000000000000000 ) ) ;
#13688 = CARTESIAN_POINT ( 'NONE',  ( -1.715153634034234598, 79.12268628210145494, -9.534712964251941258 ) ) ;
#13689 = CARTESIAN_POINT ( 'NONE',  ( -27.24356964374999990, 196.6156250006145285, -15.72908226750537786 ) ) ;
#13690 = CARTESIAN_POINT ( 'NONE',  ( 27.00000000000052580, 3.464101615137448409, -2.887499999999997513 ) ) ;
#13691 = CARTESIAN_POINT ( 'NONE',  ( -1.926257025242585782E-15, 197.9468750006145399, -31.45816453501075927 ) ) ;
#13692 = CARTESIAN_POINT ( 'NONE',  ( 5.438367727407757775E-14, 198.2000000012290002, -27.00000000000000355 ) ) ;
#13693 = CARTESIAN_POINT ( 'NONE',  ( -7.954856959092309943, 51.62731371789855928, 5.529263428287300108 ) ) ;
#13694 = CARTESIAN_POINT ( 'NONE',  ( 26.99999999999999645, 7.347880794884117764E-16, -8.775000000000005684 ) ) ;
#13695 = ORIENTED_EDGE ( 'NONE', *, *, #1699, .F. ) ;
#13696 = CARTESIAN_POINT ( 'NONE',  ( 15.00000000000000000, 241.5062500012290627, 0.000000000000000000 ) ) ;
#13697 = CARTESIAN_POINT ( 'NONE',  ( 2.311890736173452421, 55.07731371789854791, -12.53471296425189152 ) ) ;
#13698 = CARTESIAN_POINT ( 'NONE',  ( 10.31873187879411091, -3.604726614523244610, -5.559374999385509497 ) ) ;
#13699 = CARTESIAN_POINT ( 'NONE',  ( -27.24356964375000345, 198.9031250006145228, 0.000000000000000000 ) ) ;
#13700 = CARTESIAN_POINT ( 'NONE',  ( 23.87821517812499650, 4.985214923628404904, -5.803124999385484095 ) ) ;
#13701 = CARTESIAN_POINT ( 'NONE',  ( -2.660918448318004614, 26.90231371789854364, -12.46528703574811558 ) ) ;
#13702 = COLOUR_RGB ( '',0.8941176470588234615, 0.8941176470588234615, 0.8941176470588234615 ) ;
#13703 = ORIENTED_EDGE ( 'NONE', *, *, #4266, .F. ) ;
#13704 = CARTESIAN_POINT ( 'NONE',  ( 13.44051670066911086, 5.407089921784862696, -1.171874999385535965 ) ) ;
#13705 = CARTESIAN_POINT ( 'NONE',  ( 24.86380461455084756, 0.000000000000000000, 163.0057683059945930 ) ) ;
#13706 =( BOUNDED_CURVE ( )  B_SPLINE_CURVE ( 2, ( #28027, #13637, #2060, #25187, #25370, #22353, #36740 ),
 .UNSPECIFIED., .F., .T. ) 
 B_SPLINE_CURVE_WITH_KNOTS ( ( 3, 2, 2, 3 ),
 ( 0.7826086956521726146, 0.7898550724637666276, 0.7971014492753608627, 0.8043478260869549867 ),
 .UNSPECIFIED. ) 
 CURVE ( )  GEOMETRIC_REPRESENTATION_ITEM ( )  RATIONAL_B_SPLINE_CURVE ( ( 1.000000000000024647, 0.8660254037844140607, 1.000000000000000000, 0.8660254037844387076, 1.000000000000000000, 0.8660254037844674624, 0.9999999999999712452 ) ) 
 REPRESENTATION_ITEM ( '' )  );
#13707 = CARTESIAN_POINT ( 'NONE',  ( 25.22171936664797798, 0.000000000000000000, 169.8914008901326724 ) ) ;
#13708 = CARTESIAN_POINT ( 'NONE',  ( -42.07961230271182984, 211.8571965466040297, 6.469044688360755302 ) ) ;
#13709 = FACE_OUTER_BOUND ( 'NONE', #15135, .T. ) ;
#13710 =( LENGTH_UNIT ( ) NAMED_UNIT ( * ) SI_UNIT ( .MILLI., .METRE. ) );
#13711 = VECTOR ( 'NONE', #9230, 1000.000000000000000 ) ;
#13712 = PLANE ( 'NONE',  #33355 ) ;
#13713 = CARTESIAN_POINT ( 'NONE',  ( 10.49813415416005213, 74.62731371789855928, -7.228626920338837358 ) ) ;
#13714 = CARTESIAN_POINT ( 'NONE',  ( -64.44419563604517975, 205.4999999999999716, 0.1155267958017633378 ) ) ;
#13715 = CARTESIAN_POINT ( 'NONE',  ( -42.28497103062156270, 204.4285982733020148, -3.350049139982115509 ) ) ;
#13716 = ADVANCED_FACE ( 'NONE', ( #5001 ), #14813, .T. ) ;
#13717 = DIRECTION ( 'NONE',  ( 0.000000000000000000, 0.000000000000000000, 1.000000000000000000 ) ) ;
#13718 = CARTESIAN_POINT ( 'NONE',  ( 20.99999999999999645, -6.928203230275506996, -2.981249998770937992 ) ) ;
#13719 = CARTESIAN_POINT ( 'NONE',  ( -11.08355503943118592, 35.23981371789855643, -10.83675517735179383 ) ) ;
#13720 = CARTESIAN_POINT ( 'NONE',  ( -34.75669563604515844, 209.8844732041981729, -8.500000000000003553 ) ) ;
#13721 = CARTESIAN_POINT ( 'NONE',  ( -4.944772684328673229, 20.18518628210144783, 11.48171059495397728 ) ) ;
#13722 = CARTESIAN_POINT ( 'NONE',  ( 4.944772684328679446, 61.58518628210145351, -11.48171059495397373 ) ) ;
#13723 = CARTESIAN_POINT ( 'NONE',  ( -13.04141134922759804, 4.372686282101438948, -8.927990412390657937 ) ) ;
#13724 = CARTESIAN_POINT ( 'NONE',  ( 10.56230152254411259, -3.464101615137761048, -2.212500000000045652 ) ) ;
#13725 =( BOUNDED_CURVE ( )  B_SPLINE_CURVE ( 2, ( #23151, #20311, #17276, #31484, #11206, #34693, #5884, #11392, #9116 ),
 .UNSPECIFIED., .F., .F. ) 
 B_SPLINE_CURVE_WITH_KNOTS ( ( 3, 2, 2, 2, 3 ),
 ( 0.3586956521739130266, 0.3623188405797101441, 0.3695652173913043237, 0.3768115942028985588, 0.3804347826086956763 ),
 .UNSPECIFIED. ) 
 CURVE ( )  GEOMETRIC_REPRESENTATION_ITEM ( )  RATIONAL_B_SPLINE_CURVE ( ( 0.9330127018922191873, 0.9330127018922187432, 1.000000000000000000, 0.8660254037844387076, 1.000000000000000000, 0.8660254037844387076, 1.000000000000000000, 0.9330127018922188542, 0.9330127018922194093 ) ) 
 REPRESENTATION_ITEM ( '' )  );
#13726 = FACE_OUTER_BOUND ( 'NONE', #5340, .T. ) ;
#13727 = ORIENTED_EDGE ( 'NONE', *, *, #33000, .T. ) ;
#13728 = CARTESIAN_POINT ( 'NONE',  ( 11.08355503943142750, 25.36018628210144854, -10.83675517735155225 ) ) ;
#13729 = CARTESIAN_POINT ( 'NONE',  ( -13.62178482187498396, 194.9281250006145569, 23.59362340125808188 ) ) ;
#13730 = CARTESIAN_POINT ( 'NONE',  ( 13.62178482187499640, 199.2593750006145399, -23.59362340125807123 ) ) ;
#13731 = DIRECTION ( 'NONE',  ( -0.000000000000000000, -0.000000000000000000, -1.000000000000000000 ) ) ;
#13732 = CARTESIAN_POINT ( 'NONE',  ( 20.99999999999999645, 250.0000000000000000, 0.000000000000000000 ) ) ;
#13733 = CARTESIAN_POINT ( 'NONE',  ( -69.00000000000002842, 209.9999999999999716, -6.500000000000000888 ) ) ;
#13734 = CARTESIAN_POINT ( 'NONE',  ( 20.99999999999998579, 247.6374999999999886, -5.999999999999997335 ) ) ;
#13735 = CARTESIAN_POINT ( 'NONE',  ( 26.75643035624999655, 247.8343750006145285, -7.049594010296217766E-16 ) ) ;
#13736 = CARTESIAN_POINT ( 'NONE',  ( -8.710071997420207879, 116.3148137178985735, 3.796722387233182339 ) ) ;
#13737 = CARTESIAN_POINT ( 'NONE',  ( 15.24356964375000167, 242.6968750006145399, 3.323476615752272600 ) ) ;
#13738 = ORIENTED_EDGE ( 'NONE', *, *, #7478, .T. ) ;
#13739 = CARTESIAN_POINT ( 'NONE',  ( -69.39955436395486288, 214.8429017333601792, -4.673758765035196383 ) ) ;
#13740 =( NAMED_UNIT ( * ) SI_UNIT ( $, .STERADIAN. ) SOLID_ANGLE_UNIT ( ) );
#13741 = AXIS2_PLACEMENT_3D ( 'NONE', #15717, #15337, #26890 ) ;
#13742 = CARTESIAN_POINT ( 'NONE',  ( 15.00000000000000178, 247.8437500012290684, 3.464101615137757051 ) ) ;
#13743 = CARTESIAN_POINT ( 'NONE',  ( 2.660918448318003282, 114.3023137178985564, 12.46528703574811558 ) ) ;
#13744 = CARTESIAN_POINT ( 'NONE',  ( 16.56230152254411081, -7.209453229046475009, -9.478124999385530103 ) ) ;
#13745 = CARTESIAN_POINT ( 'NONE',  ( 27.62402916835064559, 5.407089921784856479, 161.5314637101514279 ) ) ;
#13746 = CARTESIAN_POINT ( 'NONE',  ( 21.00000000000000000, -6.646953231504538984, -0.5906249993854776337 ) ) ;
#13747 = CARTESIAN_POINT ( 'NONE',  ( 27.00000000000001066, 195.2375000000000114, 15.58845726811988897 ) ) ;
#13748 = ORIENTED_EDGE ( 'NONE', *, *, #11515, .F. ) ;
#13749 = ORIENTED_EDGE ( 'NONE', *, *, #22810, .F. ) ;
#13750 = ORIENTED_EDGE ( 'NONE', *, *, #22645, .F. ) ;
#13751 = CARTESIAN_POINT ( 'NONE',  ( 26.99999999999999645, 3.464101615137755275, -3.731249998770941545 ) ) ;
#13752 = CARTESIAN_POINT ( 'NONE',  ( 15.24356964374999990, 3.323476615752268604, -1.528124999385497729 ) ) ;
#13753 = CYLINDRICAL_SURFACE ( 'NONE', #19131, 5.999999999999999112 ) ;
#13754 = CARTESIAN_POINT ( 'NONE',  ( 26.99999999999999645, 247.9375000000000000, 3.464101615137751278 ) ) ;
#13755 = CARTESIAN_POINT ( 'NONE',  ( 18.12178482187500350, 248.9218750006145342, 4.985214923628407568 ) ) ;
#13756 = CARTESIAN_POINT ( 'NONE',  ( -0.1745138560725500443, 65.61018628210145209, 12.50000000000000355 ) ) ;
#13757 = DIRECTION ( 'NONE',  ( 1.000000000000000000, 0.000000000000000000, 0.000000000000000000 ) ) ;
#13758 = CARTESIAN_POINT ( 'NONE',  ( 14.82946893053495252, 216.1705310694576099, -0.5774388102985152926 ) ) ;
#13759 = CARTESIAN_POINT ( 'NONE',  ( -47.02752896937850835, 212.3500491399821613, 3.839350919129088435 ) ) ;
#13760 = AXIS2_PLACEMENT_3D ( 'NONE', #10868, #21798, #12691 ) ;
#13761 = CARTESIAN_POINT ( 'NONE',  ( 28.09424589495082714, -5.196152422706632912, 165.5087413649561938 ) ) ;
#13762 = CARTESIAN_POINT ( 'NONE',  ( -0.1745138560722763466, 119.1898137178985593, -12.50000000000000355 ) ) ;
#13763 = CARTESIAN_POINT ( 'NONE',  ( -35.75372103062156981, 216.5309553116391612, -1.626142955000564383 ) ) ;
#13764 = CARTESIAN_POINT ( 'NONE',  ( -54.55580436395489841, 218.5000000000000000, 0.1155267958017064944 ) ) ;
#13765 = CARTESIAN_POINT ( 'NONE',  ( 26.75643035624999655, 7.049594010296217766E-16, -0.9281249993854934210 ) ) ;
#13766 = CARTESIAN_POINT ( 'NONE',  ( 5.778771075727756162E-15, 196.3156250006145171, 31.45816453501075927 ) ) ;
#13767 = CARTESIAN_POINT ( 'NONE',  ( -15.50000000000000533, 98.48981371789855643, 0.1745138560722471477 ) ) ;
#13768 = CARTESIAN_POINT ( 'NONE',  ( -39.11086230271183695, 213.1499508600178387, -5.686928522499747451 ) ) ;
#13769 = VECTOR ( 'NONE', #16737, 1000.000000000000000 ) ;
#13770 = ORIENTED_EDGE ( 'NONE', *, *, #19911, .T. ) ;
#13771 = CARTESIAN_POINT ( 'NONE',  ( 24.00000000000000000, 248.8562500012290570, 5.196152422706629359 ) ) ;
#13772 = CARTESIAN_POINT ( 'NONE',  ( 12.50000000000000355, 127.7101862821014606, 0.1745138560725507937 ) ) ;
#13773 = CARTESIAN_POINT ( 'NONE',  ( -15.53471296425195369, 58.42268628210145209, 2.908627838312118019 ) ) ;
#13774 = FACE_OUTER_BOUND ( 'NONE', #12696, .T. ) ;
#13775 = CARTESIAN_POINT ( 'NONE',  ( 37.21357869082257253, 3.604726614523243278, 163.6851247292908909 ) ) ;
#13776 = CARTESIAN_POINT ( 'NONE',  ( 5.770363421893814682, 83.43518628210145494, 14.38691631536207183 ) ) ;
#13777 = CARTESIAN_POINT ( 'NONE',  ( -48.22247103062156270, 206.6499508600178672, 5.571401726697986057 ) ) ;
#13778 = CARTESIAN_POINT ( 'NONE',  ( 13.44051670066911441, -5.407089921784859143, -5.915624999385554972 ) ) ;
#13779 = CARTESIAN_POINT ( 'NONE',  ( -9.534712964251941258, 12.42268628210144144, 1.715153634034234154 ) ) ;
#13780 = DIRECTION ( 'NONE',  ( -1.000000000000000000, 0.000000000000000000, 0.000000000000000000 ) ) ;
#13781 = CARTESIAN_POINT ( 'NONE',  ( -64.45163769728823411, 215.6869285224996986, -3.149950860017881382 ) ) ;
#13782 = EDGE_CURVE ( 'NONE', #36867, #12908, #3815, .T. ) ;
#13783 = CARTESIAN_POINT ( 'NONE',  ( 15.00000000000000000, 0.000000000000000000, -5.793749998770941545 ) ) ;
#13784 = CARTESIAN_POINT ( 'NONE',  ( -10.69584247140444866, 67.04768628210145209, 6.932735513423972762 ) ) ;
#13785 = CARTESIAN_POINT ( 'NONE',  ( 13.50000000000001421, 197.9000000000000341, 23.38268590217984055 ) ) ;
#13786 = LINE ( 'NONE', #11303, #18417 ) ;
#13788 = CARTESIAN_POINT ( 'NONE',  ( 10.31873187879410558, 0.000000000000000000, -1.546874999385550176 ) ) ;
#13787 = CARTESIAN_POINT ( 'NONE',  ( 9.465287035748067623, 26.79768628210144144, 2.064181346179272847 ) ) ;
#13789 = CARTESIAN_POINT ( 'NONE',  ( -29.00000000000002487, 210.0000000000000284, -8.000000000000000000 ) ) ;
#13790 = ORIENTED_EDGE ( 'NONE', *, *, #7799, .T. ) ;
#13791 = CARTESIAN_POINT ( 'NONE',  ( 26.99999999999999645, -3.464101615137751278, -3.412500000000012967 ) ) ;
#13793 = CARTESIAN_POINT ( 'NONE',  ( 26.72225775819230975, -1.093967549749166102, -8.000000000000003553 ) ) ;
#13792 = PRODUCT_DEFINITION_SHAPE ( 'NONE', 'NONE',  #37503 ) ;
#13794 = CARTESIAN_POINT ( 'NONE',  ( 33.85854767620964623, -5.407089921784861808, 161.1554086157566985 ) ) ;
#13795 = CARTESIAN_POINT ( 'NONE',  ( 19.68408634441910721, 5.407089921784857367, -2.090624999385559679 ) ) ;
#13796 = CARTESIAN_POINT ( 'NONE',  ( 36.62857725106855611, -3.464101615137755275, 159.7931759234488425 ) ) ;
#13797 = CARTESIAN_POINT ( 'NONE',  ( 24.00000000000000000, 244.2999999999999829, 5.196152422706629359 ) ) ;
#13798 = CARTESIAN_POINT ( 'NONE',  ( 20.99999999999999645, 246.1187500012290457, 5.999999999999998224 ) ) ;
#13799 = CARTESIAN_POINT ( 'NONE',  ( 7.228626920339069173, 80.27268628210146062, -10.49813415415989404 ) ) ;
#13800 = ORIENTED_EDGE ( 'NONE', *, *, #33199, .F. ) ;
#13801 = ORIENTED_EDGE ( 'NONE', *, *, #29389, .T. ) ;
#13802 = CARTESIAN_POINT ( 'NONE',  ( -27.00000000000000355, 195.6125000012290513, 0.000000000000000000 ) ) ;
#13803 = CARTESIAN_POINT ( 'NONE',  ( 15.00000000000000000, 0.000000000000000000, -0.9000000000000119016 ) ) ;
#13804 = CARTESIAN_POINT ( 'NONE',  ( -14.25334919248795096, 51.91481371789856070, 6.092822981423662299 ) ) ;
#13805 = CARTESIAN_POINT ( 'NONE',  ( 18.12178482187499640, 4.985214923628404904, -9.778124999385489957 ) ) ;
#13806 = CARTESIAN_POINT ( 'NONE',  ( 26.75643035624999655, 242.0218750006145285, -3.323476615752271712 ) ) ;
#13807 = CIRCLE ( 'NONE', #11967, 5.000000000000000000 ) ;
#13808 = CARTESIAN_POINT ( 'NONE',  ( -52.57663769728824832, 206.0451222850691408, 2.149950860017832532 ) ) ;
#13809 = EDGE_CURVE ( 'NONE', #19565, #32257, #32735, .T. ) ;
#13810 = CARTESIAN_POINT ( 'NONE',  ( -13.49999999999998401, 199.6250000000000284, 23.38268590217985476 ) ) ;
#13811 = CARTESIAN_POINT ( 'NONE',  ( -8.843639120294245259, 34.66481371789854649, -3.474262827703533230 ) ) ;
#13812 = CARTESIAN_POINT ( 'NONE',  ( 10.31873187879410914, 0.000000000000000000, -9.590624999385537919 ) ) ;
#13813 = CARTESIAN_POINT ( 'NONE',  ( -9.534712964251895073, 98.77731371789855075, -1.715153634034446428 ) ) ;
#13814 = CARTESIAN_POINT ( 'NONE',  ( 27.24356964375000345, 199.1843750006145228, -3.336375036156643733E-15 ) ) ;
#13815 = CARTESIAN_POINT ( 'NONE',  ( 12.53471296425189330, 11.37731371789854506, 2.311890736173451977 ) ) ;
#13816 = CARTESIAN_POINT ( 'NONE',  ( -10.69584247140444866, 67.04768628210145209, 6.932735513423972762 ) ) ;
#13817 = CARTESIAN_POINT ( 'NONE',  ( 0.000000000000000000, 210.0000000000000284, 0.000000000000000000 ) ) ;
#13818 = CARTESIAN_POINT ( 'NONE',  ( 22.60769515458672174, 245.1825961894323314, 6.000000000000004441 ) ) ;
#13819 = CARTESIAN_POINT ( 'NONE',  ( 27.74168942105997360, 5.407089921784856479, 162.8763265525752786 ) ) ;
#13820 = DIRECTION ( 'NONE',  ( -0.000000000000000000, 1.000000000000000000, -0.000000000000000000 ) ) ;
#13821 = CARTESIAN_POINT ( 'NONE',  ( 16.56230152254411436, 7.209453229046482114, -6.159374999385525129 ) ) ;
#13822 = DIRECTION ( 'NONE',  ( 0.000000000000000000, 0.000000000000000000, 1.000000000000000000 ) ) ;
#13823 = DIRECTION ( 'NONE',  ( -1.000000000000000000, 0.000000000000000000, 0.000000000000000000 ) ) ;
#13824 = CARTESIAN_POINT ( 'NONE',  ( -6.594114490232312775, 69.06018628210144072, -6.840914352312096547 ) ) ;
#13825 = CARTESIAN_POINT ( 'NONE',  ( -66.61573224020317241, 223.4103818930302054, -7.500000000000000000 ) ) ;
#13826 = CARTESIAN_POINT ( 'NONE',  ( 2.660918448318279950, 107.2976862821014521, -12.46528703574805697 ) ) ;
#13827 = CARTESIAN_POINT ( 'NONE',  ( 6.000769315822030740E-16, 148.0000000000000000, -4.899999999999999467 ) ) ;
#13828 = CARTESIAN_POINT ( 'NONE',  ( 26.99999999999999645, 248.4437500012290343, 3.464101615137751278 ) ) ;
#13829 = ORIENTED_EDGE ( 'NONE', *, *, #5043, .T. ) ;
#13830 = CARTESIAN_POINT ( 'NONE',  ( 37.21521286099908110, 7.646167579472015790E-16, 163.7038033798800711 ) ) ;
#13831 = CIRCLE ( 'NONE', #34994, 2.649999999999992806 ) ;
#13832 = CARTESIAN_POINT ( 'NONE',  ( 23.87821517812499650, 4.985214923628404904, -4.790624999385456384 ) ) ;
#13833 = CARTESIAN_POINT ( 'NONE',  ( -13.62178482187498396, 196.7843750006145456, 23.59362340125808188 ) ) ;
#13834 = CARTESIAN_POINT ( 'NONE',  ( 37.44889919624123564, 3.604726614523243278, 166.3748504141385638 ) ) ;
#13835 = CARTESIAN_POINT ( 'NONE',  ( 25.24946877610209128, -3.464101615137761048, 167.4139298438261960 ) ) ;
#13836 = DIRECTION ( 'NONE',  ( -1.000000000000000000, -0.000000000000000000, -0.000000000000000000 ) ) ;
#13837 = CARTESIAN_POINT ( 'NONE',  ( 18.12178482187499640, 240.7843750006145171, -4.985214923628404904 ) ) ;
#13838 = CARTESIAN_POINT ( 'NONE',  ( 15.02283181144952628, 7.347880794884122694E-16, 50.52293445648592751 ) ) ;
#13839 = CARTESIAN_POINT ( 'NONE',  ( 10.69584247140429589, 131.5523137178985564, 6.932735513424201024 ) ) ;
#13840 = CARTESIAN_POINT ( 'NONE',  ( 0.1745138560725515708, 134.6101862821014663, -12.50000000000000355 ) ) ;
#13842 = ORIENTED_EDGE ( 'NONE', *, *, #6346, .F. ) ;
#13841 = ORIENTED_EDGE ( 'NONE', *, *, #6679, .T. ) ;
#13843 = CARTESIAN_POINT ( 'NONE',  ( 15.24356964374999990, 244.3093750006145228, -3.323476615752268604 ) ) ;
#13844 = CARTESIAN_POINT ( 'NONE',  ( 26.99999999999999645, 7.347880794884117764E-16, -1.518749998770940746 ) ) ;
#13845 = CARTESIAN_POINT ( 'NONE',  ( 15.24356964375000167, -3.323476615752272600, -4.603124999385474148 ) ) ;
#13846 = CARTESIAN_POINT ( 'NONE',  ( -0.1745138560722442889, 109.9898137178985706, -15.50000000000000533 ) ) ;
#13847 = CARTESIAN_POINT ( 'NONE',  ( 22.56230152254411792, 7.347880794884125653E-16, -9.675000000000045119 ) ) ;
#13848 = CARTESIAN_POINT ( 'NONE',  ( 15.24356964374999990, 0.000000000000000000, -2.953124999385492444 ) ) ;
#13849 = VECTOR ( 'NONE', #9816, 1000.000000000000000 ) ;
#13850 = CARTESIAN_POINT ( 'NONE',  ( 10.31873187879410736, 3.604726614523240613, -8.784374999385505589 ) ) ;
#13851 = CARTESIAN_POINT ( 'NONE',  ( 27.00000000000001066, 198.9500000012290570, 15.58845726811988897 ) ) ;
#13852 = CARTESIAN_POINT ( 'NONE',  ( -2.311890736173176641, 115.9226862821014521, -12.53471296425194836 ) ) ;
#13853 = CARTESIAN_POINT ( 'NONE',  ( 10.31873187879411091, -3.604726614523240613, -3.703124999385514649 ) ) ;
#13854 = CARTESIAN_POINT ( 'NONE',  ( -36.73586230271183695, 205.8500491399821613, 7.418979330068642852 ) ) ;
#13855 = CARTESIAN_POINT ( 'NONE',  ( 18.12178482187499640, 244.2718750006145001, -4.985214923628404904 ) ) ;
#13856 = DIRECTION ( 'NONE',  ( -1.000000000000000000, -4.130293990420971855E-17, 0.000000000000000000 ) ) ;
#13857 = CARTESIAN_POINT ( 'NONE',  ( -33.56919563604517265, 214.5000000000000284, -0.1155267958017627827 ) ) ;
#13858 = CARTESIAN_POINT ( 'NONE',  ( 12.50000000000000355, 118.5101862821014578, 0.1745138560725507937 ) ) ;
#13859 = CARTESIAN_POINT ( 'NONE',  ( 19.56230152254411081, -5.196152422706629359, -1.087499998771029874 ) ) ;
#13860 = CARTESIAN_POINT ( 'NONE',  ( -40.89955436395488420, 214.8429017333601792, -4.673758765035196383 ) ) ;
#13861 = DIRECTION ( 'NONE',  ( -0.000000000000000000, -1.000000000000000000, -0.000000000000000000 ) ) ;
#13862 = CARTESIAN_POINT ( 'NONE',  ( -13.50000000000000533, 199.4750000000000227, -23.38268590217984411 ) ) ;
#13863 = CARTESIAN_POINT ( 'NONE',  ( 5.770363421893814682, 111.0351862821014635, 14.38691631536207183 ) ) ;
#13864 = CARTESIAN_POINT ( 'NONE',  ( -0.1745138560725500443, 10.41018628210144215, 12.50000000000000355 ) ) ;
#13865 = CARTESIAN_POINT ( 'NONE',  ( 7.234628195640337545, 198.0674038105676971, -26.99999999999999289 ) ) ;
#13866 = CARTESIAN_POINT ( 'NONE',  ( -0.1745138560725182642, 139.2101862821014890, 9.500000000000005329 ) ) ;
#13867 = CARTESIAN_POINT ( 'NONE',  ( 22.80587116629410716, 3.604726614523238837, -0.3281249993855308578 ) ) ;
#13868 = CARTESIAN_POINT ( 'NONE',  ( -69.00000000000002842, 206.0000000000000000, -2.499999999999998668 ) ) ;
#13869 = ORIENTED_EDGE ( 'NONE', *, *, #27231, .F. ) ;
#13870 = LINE ( 'NONE', #1736, #17950 ) ;
#13871 = CARTESIAN_POINT ( 'NONE',  ( 9.465287035748067623, 72.79768628210145209, 2.064181346179272847 ) ) ;
#13872 = CARTESIAN_POINT ( 'NONE',  ( 3.306546357697854128E-15, 200.0000000000000000, 27.00000000000000355 ) ) ;
#13873 = EDGE_CURVE ( 'NONE', #16548, #25843, #22344, .T. ) ;
#13874 = CARTESIAN_POINT ( 'NONE',  ( -13.62178482187498396, 196.7281250006145399, 23.59362340125808188 ) ) ;
#13875 = CARTESIAN_POINT ( 'NONE',  ( 15.00000000000039613, 3.464101615137982204, -2.737500000000008260 ) ) ;
#13876 = CARTESIAN_POINT ( 'NONE',  ( 27.24356964374999635, 195.1718750006145342, -15.72908226750539029 ) ) ;
#13877 = DIRECTION ( 'NONE',  ( -0.000000000000000000, -0.000000000000000000, 1.000000000000000000 ) ) ;
#13878 = ADVANCED_FACE ( 'NONE', ( #9515 ), #21088, .F. ) ;
#13879 = CARTESIAN_POINT ( 'NONE',  ( 13.56230152254410548, 5.196152422706630247, -6.712499998771020771 ) ) ;
#13880 = CARTESIAN_POINT ( 'NONE',  ( 3.796722387233182339, 49.61481371789856354, 8.710071997420207879 ) ) ;
#13881 = CARTESIAN_POINT ( 'NONE',  ( 15.00000000000000000, 3.464101615137752166, -9.037500000000006750 ) ) ;
#13882 = EDGE_LOOP ( 'NONE', ( #17930, #14347, #1656, #13749 ) ) ;
#13883 = CARTESIAN_POINT ( 'NONE',  ( 21.00000000000000000, 242.7437500012290457, -6.928203230275506996 ) ) ;
#13884 = CARTESIAN_POINT ( 'NONE',  ( 4.944772684328420986, 68.01481371789854791, 11.48171059495408208 ) ) ;
#13885 = CARTESIAN_POINT ( 'NONE',  ( 22.80587116629411426, 3.604726614523243278, -7.134374999385543425 ) ) ;
#13886 = CARTESIAN_POINT ( 'NONE',  ( 15.24356964375000167, -3.323476615752272600, -6.965624999385507721 ) ) ;
#13887 = CARTESIAN_POINT ( 'NONE',  ( -12.50000000000000355, 24.88981371789854435, 0.1745138560722786503 ) ) ;
#13888 = EDGE_CURVE ( 'NONE', #13555, #2263, #4839, .T. ) ;
#13889 = ORIENTED_EDGE ( 'NONE', *, *, #10802, .F. ) ;
#13890 = CARTESIAN_POINT ( 'NONE',  ( 10.31873187879410736, 0.000000000000000000, -0.6468749993855105185 ) ) ;
#13891 = DIRECTION ( 'NONE',  ( 0.000000000000000000, 0.000000000000000000, 1.000000000000000000 ) ) ;
#13892 = CARTESIAN_POINT ( 'NONE',  ( 34.42070221693199272, 5.407089921784862696, 167.5808644184484706 ) ) ;
#13893 = CARTESIAN_POINT ( 'NONE',  ( -42.87127896937850124, 216.5309553116391612, 1.626142955000506873 ) ) ;
#13894 = CARTESIAN_POINT ( 'NONE',  ( 31.39985900347063819, -6.928203230275506996, 168.8709323510219917 ) ) ;
#13895 =( LENGTH_UNIT ( ) NAMED_UNIT ( * ) SI_UNIT ( .MILLI., .METRE. ) );
#13896 = DIRECTION ( 'NONE',  ( 0.000000000000000000, -1.000000000000000000, 0.000000000000000000 ) ) ;
#13897 = CARTESIAN_POINT ( 'NONE',  ( -36.74330436395489130, 210.1155267958017703, -4.499999999999996447 ) ) ;
#13898 = CARTESIAN_POINT ( 'NONE',  ( -42.48288769728824121, 203.5309553116391612, -1.857196546604028775 ) ) ;
#13899 = VERTEX_POINT ( 'NONE', #35655 ) ;
#13900 = DIRECTION ( 'NONE',  ( 1.000000000000000000, 0.000000000000000000, -0.000000000000000000 ) ) ;
#13901 = DIRECTION ( 'NONE',  ( 0.000000000000000000, -0.000000000000000000, -1.000000000000000000 ) ) ;
#13902 = CARTESIAN_POINT ( 'NONE',  ( 5.770363421894130873, 36.96481371789853654, -14.38691631536193860 ) ) ;
#13903 = CARTESIAN_POINT ( 'NONE',  ( -38.91294563604516554, 216.1378603801729241, -6.307003348498026796 ) ) ;
#13904 = CARTESIAN_POINT ( 'NONE',  ( -4.944772684328673229, 10.98518628210143433, 11.48171059495397728 ) ) ;
#13905 = CARTESIAN_POINT ( 'NONE',  ( -11.61527771782819940, 58.13518628210144357, 4.622313124798574258 ) ) ;
#13906 = CARTESIAN_POINT ( 'NONE',  ( -0.1745138560725817967, 10.41018628210144037, 15.50000000000000533 ) ) ;
#13907 = CARTESIAN_POINT ( 'NONE',  ( 10.56230152254410903, 0.000000000000000000, -2.250000000000057732 ) ) ;
#13908 = DIRECTION ( 'NONE',  ( 0.000000000000000000, 0.000000000000000000, 1.000000000000000000 ) ) ;
#13909 = ORIENTED_EDGE ( 'NONE', *, *, #9234, .F. ) ;
#13910 = CARTESIAN_POINT ( 'NONE',  ( 14.38691631536207538, 35.13518628210143646, -5.770363421893813793 ) ) ;
#13911 = CARTESIAN_POINT ( 'NONE',  ( -13.62178482187498396, 196.2781250006145228, 23.59362340125808188 ) ) ;
#13912 = CARTESIAN_POINT ( 'NONE',  ( -27.24356964374999635, 198.5468750006145626, 15.72908226750539384 ) ) ;
#13913 = CARTESIAN_POINT ( 'NONE',  ( 22.56230152254410370, 7.347880794884117764E-16, -6.412499998770998744 ) ) ;
#13914 = DIRECTION ( 'NONE',  ( -0.000000000000000000, -0.000000000000000000, 1.000000000000000000 ) ) ;
#13915 = CARTESIAN_POINT ( 'NONE',  ( 13.49999999999999645, 195.8000000000000114, -23.38268590217984766 ) ) ;
#13916 = CARTESIAN_POINT ( 'NONE',  ( 37.06980319883601283, -3.464101615137536783, 164.8364115837626684 ) ) ;
#13917 =( REPRESENTATION_RELATIONSHIP ('NONE','NONE', #4304, #10397 ) REPRESENTATION_RELATIONSHIP_WITH_TRANSFORMATION ( #10350 )SHAPE_REPRESENTATION_RELATIONSHIP( ) );
#13918 = CARTESIAN_POINT ( 'NONE',  ( 26.75643035624999655, 246.9343750006145228, -7.049594010296217766E-16 ) ) ;
#13919 = CARTESIAN_POINT ( 'NONE',  ( 5.529263428287300108, 113.7273137178985678, 7.954856959092309943 ) ) ;
#13920 = CARTESIAN_POINT ( 'NONE',  ( 20.99999999999999645, 242.3218750006145399, 6.646953231504538984 ) ) ;
#13921 = ORIENTED_EDGE ( 'NONE', *, *, #7419, .F. ) ;
#13922 = CARTESIAN_POINT ( 'NONE',  ( -69.79538769728823411, 211.8571965466039444, -6.469044688360768625 ) ) ;
#13923 = CARTESIAN_POINT ( 'NONE',  ( 15.00000000000000000, 249.6062500012290570, 0.000000000000000000 ) ) ;
#13924 = CARTESIAN_POINT ( 'NONE',  ( -12.46528703574811558, 116.6023137178985536, 2.660918448318004170 ) ) ;
#13925 = CARTESIAN_POINT ( 'NONE',  ( 16.56230152254410726, 7.209453229046475009, -9.253124999385514471 ) ) ;
#13926 = CARTESIAN_POINT ( 'NONE',  ( 24.67427235751429393, 3.604726614523236616, 163.6340529427438639 ) ) ;
#13927 =( BOUNDED_CURVE ( )  B_SPLINE_CURVE ( 2, ( #7389, #33721, #36367, #13263, #13448, #36181, #18591 ),
 .UNSPECIFIED., .F., .F. ) 
 B_SPLINE_CURVE_WITH_KNOTS ( ( 3, 2, 2, 3 ),
 ( 0.3043478260869552643, 0.3115942028985494994, 0.3188405797101437900, 0.3260869565217380805 ),
 .UNSPECIFIED. ) 
 CURVE ( )  GEOMETRIC_REPRESENTATION_ITEM ( )  RATIONAL_B_SPLINE_CURVE ( ( 1.000000000000023759, 0.8660254037844151709, 1.000000000000000000, 0.8660254037844387076, 1.000000000000000000, 0.8660254037844582475, 0.9999999999999804601 ) ) 
 REPRESENTATION_ITEM ( '' )  );
#13928 = CARTESIAN_POINT ( 'NONE',  ( 5.649999999999987921, 244.5000000000000000, 5.000000000000000000 ) ) ;
#13929 = CARTESIAN_POINT ( 'NONE',  ( -13.50000000000000533, 195.8750000000000284, -23.38268590217984411 ) ) ;
#13930 = ORIENTED_EDGE ( 'NONE', *, *, #25674, .T. ) ;
#13931 = VERTEX_POINT ( 'NONE', #21645 ) ;
#13932 = VECTOR ( 'NONE', #7385, 1000.000000000000000 ) ;
#13933 = ORIENTED_EDGE ( 'NONE', *, *, #25413, .F. ) ;
#13934 = CARTESIAN_POINT ( 'NONE',  ( 15.00000000000000178, -3.464101615137757051, -5.306249998770942611 ) ) ;
#13935 = CARTESIAN_POINT ( 'NONE',  ( 20.99999999999999645, -6.646953231504538984, -3.178124999385461003 ) ) ;
#13936 = CARTESIAN_POINT ( 'NONE',  ( 15.00000000000000178, 241.9937500012290457, 3.464101615137757051 ) ) ;
#13937 = CARTESIAN_POINT ( 'NONE',  ( 18.12178482187499640, 249.2218750006145171, -4.985214923628404904 ) ) ;
#13938 = CARTESIAN_POINT ( 'NONE',  ( 11.61527771782819940, 53.53518628210144925, -4.622313124798573369 ) ) ;
#13939 = CARTESIAN_POINT ( 'NONE',  ( -63.65252896937849414, 206.6499508600178387, -5.571401726697954970 ) ) ;
#13940 = CARTESIAN_POINT ( 'NONE',  ( 6.017554903305174285, 215.6184169112604536, -2.114697272285170460 ) ) ;
#13941 = CARTESIAN_POINT ( 'NONE',  ( -37.92336230271182984, 213.9548777149308023, 2.149950860017852960 ) ) ;
#13942 = CARTESIAN_POINT ( 'NONE',  ( 20.99999999999999645, 185.0294372515228645, 0.000000000000000000 ) ) ;
#13943 = CIRCLE ( 'NONE', #2430, 7.500000000000000000 ) ;
#13944 = CARTESIAN_POINT ( 'NONE',  ( 24.98146486726017912, 0.000000000000000000, 164.3506311484184437 ) ) ;
#13945 = CARTESIAN_POINT ( 'NONE',  ( 10.49813415416005213, 120.6273137178985735, -7.228626920338837358 ) ) ;
#13946 = CARTESIAN_POINT ( 'NONE',  ( -37.53497103062156981, 204.4285982733020148, -3.350049139982115509 ) ) ;
#13947 = CARTESIAN_POINT ( 'NONE',  ( -49.60788769728823411, 218.4690446883607535, 2.393094931466250408 ) ) ;
#13948 =( BOUNDED_CURVE ( )  B_SPLINE_CURVE ( 2, ( #22379, #33927, #25578, #28241, #1896, #13467, #10617, #22196, #33744 ),
 .UNSPECIFIED., .F., .F. ) 
 B_SPLINE_CURVE_WITH_KNOTS ( ( 3, 2, 2, 2, 3 ),
 ( 0.5326086956521739468, 0.5362318840579710644, 0.5434782608695651884, 0.5507246376811594235, 0.5543478260869565410 ),
 .UNSPECIFIED. ) 
 CURVE ( )  GEOMETRIC_REPRESENTATION_ITEM ( )  RATIONAL_B_SPLINE_CURVE ( ( 0.9330127018922194093, 0.9330127018922194093, 1.000000000000000000, 0.8660254037844387076, 1.000000000000000000, 0.8660254037844387076, 1.000000000000000000, 0.9330127018922194093, 0.9330127018922194093 ) ) 
 REPRESENTATION_ITEM ( '' )  );
#13949 = CARTESIAN_POINT ( 'NONE',  ( 23.87821517812500005, -4.985214923628404016, -1.453124999385491112 ) ) ;
#13950 = CARTESIAN_POINT ( 'NONE',  ( -27.24356964374999635, 195.3406250006145513, 15.72908226750539384 ) ) ;
#13951 = CARTESIAN_POINT ( 'NONE',  ( 8.927990412390371944, 86.12731371789853085, 13.04141134922778811 ) ) ;
#13952 = CARTESIAN_POINT ( 'NONE',  ( -37.72544563604515844, 214.8429017333602360, 4.673758765035156415 ) ) ;
#13953 = VERTEX_POINT ( 'NONE', #10628 ) ;
#13954 = CARTESIAN_POINT ( 'NONE',  ( 22.60769515458672885, 240.8674038105676516, -5.999999999999998224 ) ) ;
#13955 = CARTESIAN_POINT ( 'NONE',  ( 2.311890736173175753, 129.7226862821014777, 12.53471296425194836 ) ) ;
#13956 = CARTESIAN_POINT ( 'NONE',  ( -3.257655550457281723, 56.69768628210144357, 15.46528703574804986 ) ) ;
#13957 = CARTESIAN_POINT ( 'NONE',  ( 36.97498984505087805, 7.646167579472024665E-16, 160.9580417432647153 ) ) ;
#13958=STYLED_ITEM('',(#37535),#20157);
#13959 = CARTESIAN_POINT ( 'NONE',  ( 8.927990412390657937, 80.27268628210143220, -13.04141134922759804 ) ) ;
#13960 = CARTESIAN_POINT ( 'NONE',  ( 13.44051670066911619, -5.407089921784859143, -5.465624999385548577 ) ) ;
#13961 = CARTESIAN_POINT ( 'NONE',  ( -6.840914352312096547, 29.96018628210143575, 6.594114490232313663 ) ) ;
#13962 = DIRECTION ( 'NONE',  ( 1.000000000000000000, 0.000000000000000000, 0.000000000000000000 ) ) ;
#13963 = CARTESIAN_POINT ( 'NONE',  ( -63.85788769728821279, 216.4690446883607535, 1.857196546604031662 ) ) ;
#13964 = CARTESIAN_POINT ( 'NONE',  ( 10.56230152254410903, 0.000000000000000000, -7.200000000000040146 ) ) ;
#13965 = CARTESIAN_POINT ( 'NONE',  ( 2.311890736173175753, 56.12268628210144072, 12.53471296425194836 ) ) ;
#13966 = CARTESIAN_POINT ( 'NONE',  ( 26.99999999999999645, 197.1125000000000398, -15.58845726811990495 ) ) ;
#13967 = FACE_OUTER_BOUND ( 'NONE', #16034, .T. ) ;
#13969 = CARTESIAN_POINT ( 'NONE',  ( 10.31873187879410736, -3.604726614523244610, -2.409374999385539340 ) ) ;
#13968 = CARTESIAN_POINT ( 'NONE',  ( 9.534712964251941258, 26.22268628210144925, -1.715153634034235708 ) ) ;
#13970 = CARTESIAN_POINT ( 'NONE',  ( 15.24356964374999990, 248.9218750006145626, -3.323476615752268604 ) ) ;
#13971 = VERTEX_POINT ( 'NONE', #19185 ) ;
#13972 = CARTESIAN_POINT ( 'NONE',  ( 21.00000000000000000, -6.928203230275506996, -4.387499999999998401 ) ) ;
#13973 = CARTESIAN_POINT ( 'NONE',  ( 21.00000000000000355, 0.000000000000000000, 50.00000000000001421 ) ) ;
#13974 = CARTESIAN_POINT ( 'NONE',  ( 33.81932759197320593, -5.407089921784861808, 160.7071210016154055 ) ) ;
#13975 = CARTESIAN_POINT ( 'NONE',  ( 16.56230152254411081, -7.209453229046475009, -2.278124999385533478 ) ) ;
#13976 = CARTESIAN_POINT ( 'NONE',  ( 37.64336544724691436, -3.604726614523235284, 168.5976098342557918 ) ) ;
#13977 = CARTESIAN_POINT ( 'NONE',  ( 23.99999999999999645, 243.5499999999999829, -5.196152422706631135 ) ) ;
#13978 = CARTESIAN_POINT ( 'NONE',  ( 10.49813415415989581, 73.37268628210144072, 7.228626920339069173 ) ) ;
#13979 = VERTEX_POINT ( 'NONE', #33006 ) ;
#13980 = ORIENTED_EDGE ( 'NONE', *, *, #29782, .T. ) ;
#13981 = CARTESIAN_POINT ( 'NONE',  ( 5.727106289114498080E-15, 195.2750000012290172, 31.17691453623979214 ) ) ;
#13982 = CARTESIAN_POINT ( 'NONE',  ( -3.253724281355068545E-15, 195.9500000012290002, -27.00000000000000355 ) ) ;
#13983 = CARTESIAN_POINT ( 'NONE',  ( -15.46528703574811736, 43.00231371789853796, 3.257655550456946436 ) ) ;
#13984 = CARTESIAN_POINT ( 'NONE',  ( 26.75643035624999655, 7.049594010296217766E-16, -8.578124999385483562 ) ) ;
#13985 = CARTESIAN_POINT ( 'NONE',  ( 21.00000000000000000, 243.6718750006145058, 6.646953231504538984 ) ) ;
#13986 = AXIS2_PLACEMENT_3D ( 'NONE', #23540, #32245, #6285 ) ;
#13987 = CARTESIAN_POINT ( 'NONE',  ( -47.62872103062157692, 205.4690446883607535, 1.090244570138264368 ) ) ;
#13988 = CARTESIAN_POINT ( 'NONE',  ( 20.00041297495057080, 239.8598985277379256, -5.668978411116884608 ) ) ;
#13989 = CARTESIAN_POINT ( 'NONE',  ( 37.05016167317072728, -3.604726614523238837, 161.8172596703688555 ) ) ;
#13990 = CARTESIAN_POINT ( 'NONE',  ( -8.152565276336593669, 44.15231371789854364, -5.233372021372610483 ) ) ;
#13991 = CARTESIAN_POINT ( 'NONE',  ( 10.31873187879410736, 3.604726614523236616, -9.628124999385549998 ) ) ;
#13992 = EDGE_CURVE ( 'NONE', #14430, #2262, #7239, .T. ) ;
#13993 = CARTESIAN_POINT ( 'NONE',  ( -3.796722387233185003, 100.2148137178985650, -8.710071997420207879 ) ) ;
#13994 = CARTESIAN_POINT ( 'NONE',  ( -13.62178482187500528, 198.8843750006145399, -23.59362340125807123 ) ) ;
#13995 = CARTESIAN_POINT ( 'NONE',  ( 3.257655550456945548, 141.9023137178985507, 15.46528703574811736 ) ) ;
#13996 = CARTESIAN_POINT ( 'NONE',  ( -4.622313124798576922, 69.63518628210145778, -11.61527771782819762 ) ) ;
#13997 = DIRECTION ( 'NONE',  ( -0.000000000000000000, 1.000000000000000000, -0.000000000000000000 ) ) ;
#13998 = CARTESIAN_POINT ( 'NONE',  ( 26.99999999999967670, 3.464101615137938683, -1.931249998770954823 ) ) ;
#13999 = CARTESIAN_POINT ( 'NONE',  ( 24.44222019244867283, 0.000000000000000000, 160.9816845590745800 ) ) ;
#14000 = CARTESIAN_POINT ( 'NONE',  ( 21.00000000000000000, 6.928203230275506996, -0.5062499987709455640 ) ) ;
#14001 = CARTESIAN_POINT ( 'NONE',  ( 10.31873187879410736, -3.604726614523244610, -8.709374999385511629 ) ) ;
#14002 = CARTESIAN_POINT ( 'NONE',  ( 22.56230152254411792, 7.347880794884125653E-16, -0.2250000000000584865 ) ) ;
#14003 = CARTESIAN_POINT ( 'NONE',  ( -3.474262827703337830, 78.83518628210146062, -8.843639120294326972 ) ) ;
#14004 = DIRECTION ( 'NONE',  ( -0.000000000000000000, -0.000000000000000000, 1.000000000000000000 ) ) ;
#14005 = EDGE_CURVE ( 'NONE', #32985, #17695, #33954, .T. ) ;
#14006 = CARTESIAN_POINT ( 'NONE',  ( -8.715434833791929847, 115.0601862821014549, -8.962234695871762469 ) ) ;
#14007 = FACE_OUTER_BOUND ( 'NONE', #36146, .T. ) ;
#14008 = CARTESIAN_POINT ( 'NONE',  ( 22.56230152254410370, 7.347880794884117764E-16, -3.712499998771018106 ) ) ;
#14009 = EDGE_LOOP ( 'NONE', ( #20570, #33017, #18224, #30435 ) ) ;
#14010 = VECTOR ( 'NONE', #6054, 1000.000000000000000 ) ;
#14011 = CARTESIAN_POINT ( 'NONE',  ( 24.48470861703815515, -3.604726614523240613, 161.4673294743943188 ) ) ;
#14012 = CARTESIAN_POINT ( 'NONE',  ( 18.12178482187499640, 4.985214923628404904, -8.765624999385462246 ) ) ;
#14013 = ADVANCED_FACE ( 'NONE', ( #36030 ), #294, .T. ) ;
#14014 = CARTESIAN_POINT ( 'NONE',  ( 20.99999999999999645, 185.0294372515228645, 0.000000000000000000 ) ) ;
#14015 = CARTESIAN_POINT ( 'NONE',  ( 31.33367511126808935, -7.209453229046482114, 168.1144470015463810 ) ) ;
#14016 = CARTESIAN_POINT ( 'NONE',  ( 37.09921826190588234, -3.464101615137755275, 165.1726272931442452 ) ) ;
#14017 = DIRECTION ( 'NONE',  ( -0.000000000000000000, 1.000000000000000000, -0.000000000000000000 ) ) ;
#14018 = CARTESIAN_POINT ( 'NONE',  ( 18.12178482187499640, 240.3343750006145285, -4.985214923628404904 ) ) ;
#14019 = CARTESIAN_POINT ( 'NONE',  ( 13.62178482187499640, 198.7531250006145456, -23.59362340125807123 ) ) ;
#14020 = EDGE_CURVE ( 'NONE', #36971, #34798, #4183, .T. ) ;
#14021 = CARTESIAN_POINT ( 'NONE',  ( -12.46528703574811558, 116.6023137178985678, 2.660918448318003726 ) ) ;
#14022 = CARTESIAN_POINT ( 'NONE',  ( -10.49813415415989404, 133.1726862821014663, -7.228626920339069173 ) ) ;
#14024 = VERTEX_POINT ( 'NONE', #33818 ) ;
#14023 = ORIENTED_EDGE ( 'NONE', *, *, #23631, .T. ) ;
#14025 = CARTESIAN_POINT ( 'NONE',  ( 26.75643035624999655, 241.3843750006145399, 3.323476615752267715 ) ) ;
#14026 = DIRECTION ( 'NONE',  ( 0.000000000000000000, 0.000000000000000000, 1.000000000000000000 ) ) ;
#14027 = CARTESIAN_POINT ( 'NONE',  ( 10.83675517735179206, 101.9398137178985735, -11.08355503943118769 ) ) ;
#14028 = CARTESIAN_POINT ( 'NONE',  ( 12.31958322920955062, -4.655204641349882877, -9.999999999999996447 ) ) ;
#14029 = CARTESIAN_POINT ( 'NONE',  ( 26.75643035624999655, 7.049594010296217766E-16, -1.828124999385477567 ) ) ;
#14030 = CARTESIAN_POINT ( 'NONE',  ( 22.80587116629411426, 3.604726614523243278, -7.584374999385507188 ) ) ;
#14031 = CARTESIAN_POINT ( 'NONE',  ( 13.50000000000001421, 198.9125000012290343, 23.38268590217984055 ) ) ;
#14032 = AXIS2_PLACEMENT_3D ( 'NONE', #28306, #13351, #19614 ) ;
#14033 = CARTESIAN_POINT ( 'NONE',  ( 7.228626920339068285, 117.0726862821014720, -10.49813415415989581 ) ) ;
#14034 = CARTESIAN_POINT ( 'NONE',  ( 22.80587116629411426, 3.604726614523238837, -3.928124999385560923 ) ) ;
#14035 = CARTESIAN_POINT ( 'NONE',  ( -38.91294563604516554, 216.1378603801729241, -6.307003348498026796 ) ) ;
#14036 = CARTESIAN_POINT ( 'NONE',  ( 18.12178482187500350, 243.5218750006145001, 4.985214923628407568 ) ) ;
#14037 = VECTOR ( 'NONE', #21522, 1000.000000000000000 ) ;
#14038 = EDGE_CURVE ( 'NONE', #12999, #29663, #24008, .T. ) ;
#14039 = CARTESIAN_POINT ( 'NONE',  ( -67.41294563604516554, 214.6737587650350747, -4.842901733360249317 ) ) ;
#14040 = CARTESIAN_POINT ( 'NONE',  ( -6.932735513423968321, 124.5476862821014663, -10.69584247140445221 ) ) ;
#14041 = CARTESIAN_POINT ( 'NONE',  ( 19.56230152254411436, -5.196152422706629359, -3.787499998771037824 ) ) ;
#14042 = CARTESIAN_POINT ( 'NONE',  ( -49.60788769728823411, 216.4690446883607535, 1.857196546604031662 ) ) ;
#14043 = CARTESIAN_POINT ( 'NONE',  ( 23.99999999999999645, 240.0062500012290627, -5.196152422706631135 ) ) ;
#14044 = CARTESIAN_POINT ( 'NONE',  ( 19.39230484541324273, 244.6924038105676686, 5.999999999999987566 ) ) ;
#14045 = CARTESIAN_POINT ( 'NONE',  ( -0.1745138560725817967, 102.4101862821014493, 15.50000000000000533 ) ) ;
#14046 = CARTESIAN_POINT ( 'NONE',  ( 8.715434833791931624, 18.46018628210144286, 8.962234695871760692 ) ) ;
#14047 = EDGE_CURVE ( 'NONE', #29619, #2209, #19615, .T. ) ;
#14048 = LINE ( 'NONE', #22768, #33301 ) ;
#14049 = CARTESIAN_POINT ( 'NONE',  ( -5.529263428287477744, 140.0726862821014151, 7.954856959092191815 ) ) ;
#14050 = CARTESIAN_POINT ( 'NONE',  ( 22.80587116629410716, 3.604726614523238837, -2.578124999385541738 ) ) ;
#14051 = CARTESIAN_POINT ( 'NONE',  ( 24.90302469878729141, 0.000000000000000000, 163.4540559201358576 ) ) ;
#14052 = ORIENTED_EDGE ( 'NONE', *, *, #6243, .F. ) ;
#14053 = CARTESIAN_POINT ( 'NONE',  ( 22.56230152254410370, 7.347880794884117764E-16, -4.612499998771030008 ) ) ;
#14054 = CARTESIAN_POINT ( 'NONE',  ( 0.1745138560725194299, 61.01018628210145067, -9.500000000000005329 ) ) ;
#14055 = AXIS2_PLACEMENT_3D ( 'NONE', #34089, #37109, #8139 ) ;
#14056 = CARTESIAN_POINT ( 'NONE',  ( 20.99999999999999289, 244.0937500012290116, -5.999999999999997335 ) ) ;
#14057 = EDGE_CURVE ( 'NONE', #4178, #5932, #18711, .T. ) ;
#14058 = CARTESIAN_POINT ( 'NONE',  ( -38.47274018782781013, 246.3803829651731121, 0.5000000000000000000 ) ) ;
#14059 = DIRECTION ( 'NONE',  ( 0.000000000000000000, 0.000000000000000000, -1.000000000000000000 ) ) ;
#14060 = CARTESIAN_POINT ( 'NONE',  ( 13.62178482187501416, 196.4093750006145456, 23.59362340125806767 ) ) ;
#14061 = CARTESIAN_POINT ( 'NONE',  ( 20.99999999999999289, 244.5437500012290286, -5.999999999999997335 ) ) ;
#14062 = CARTESIAN_POINT ( 'NONE',  ( 9.465287035748106703, 38.40231371789853654, -2.064181346179063237 ) ) ;
#14063 = CARTESIAN_POINT ( 'NONE',  ( 26.99999999999999645, -3.464101615137751278, -9.712500000000016342 ) ) ;
#14064 = ORIENTED_EDGE ( 'NONE', *, *, #1589, .T. ) ;
#14065 = CARTESIAN_POINT ( 'NONE',  ( 15.00000000000000000, 241.9562500012290513, 0.000000000000000000 ) ) ;
#14066 = CARTESIAN_POINT ( 'NONE',  ( 2.311890736173452421, 64.27731371789855075, -12.53471296425189152 ) ) ;
#14067 = CARTESIAN_POINT ( 'NONE',  ( 16.56230152254411436, 7.209453229046482114, -8.409374999385503813 ) ) ;
#14068 = CARTESIAN_POINT ( 'NONE',  ( 26.75643035624999655, 3.323476615752271712, -8.990624999385502747 ) ) ;
#14069 = CARTESIAN_POINT ( 'NONE',  ( 4.944772684328420986, 22.01481371789855501, 11.48171059495408208 ) ) ;
#14070 = ORIENTED_EDGE ( 'NONE', *, *, #9163, .F. ) ;
#14071 = CARTESIAN_POINT ( 'NONE',  ( 10.31873187879410736, 0.000000000000000000, -1.096874999385516469 ) ) ;
#14072 = CARTESIAN_POINT ( 'NONE',  ( 10.69584247140445221, 7.247686282101428290, -6.932735513423970097 ) ) ;
#14073 = CARTESIAN_POINT ( 'NONE',  ( 28.02440086159767674, -5.407089921784865361, 166.1077331045103733 ) ) ;
#14074 = CARTESIAN_POINT ( 'NONE',  ( -39.11086230271183695, 213.1499508600178387, -5.686928522499747451 ) ) ;
#14075 = LINE ( 'NONE', #36995, #13769 ) ;
#14076 = LINE ( 'NONE', #5348, #23030 ) ;
#14077 = EDGE_CURVE ( 'NONE', #4638, #23066, #8064, .T. ) ;
#14078 = CARTESIAN_POINT ( 'NONE',  ( -32.19122103062156270, 208.9097554298617752, -4.530955311639240257 ) ) ;
#14079 = CARTESIAN_POINT ( 'NONE',  ( -48.42038769728821990, 208.1428034533959703, 6.469044688360770401 ) ) ;
#14080 = CARTESIAN_POINT ( 'NONE',  ( 34.50404489593442747, 5.407089921784857367, 168.5334755984986828 ) ) ;
#14081 = ORIENTED_EDGE ( 'NONE', *, *, #31453, .T. ) ;
#14082 = DIRECTION ( 'NONE',  ( 0.08715574274765150453, 0.000000000000000000, 0.9961946980917461003 ) ) ;
#14083 = CARTESIAN_POINT ( 'NONE',  ( 14.99999999999941380, -3.464101615137419543, -7.162500000000004974 ) ) ;
#14084 = CARTESIAN_POINT ( 'NONE',  ( 10.83675517735179206, 19.13981371789855146, -11.08355503943118769 ) ) ;
#14085 = CARTESIAN_POINT ( 'NONE',  ( -31.98586230271182984, 205.8500491399821613, 7.418979330068642852 ) ) ;
#14086 = CARTESIAN_POINT ( 'NONE',  ( 3.474262827703335166, 138.6351862821014720, 8.843639120294326972 ) ) ;
#14087 = CARTESIAN_POINT ( 'NONE',  ( 7.228626920339068285, 43.47268628210144925, -10.49813415415989581 ) ) ;
#14088 = CARTESIAN_POINT ( 'NONE',  ( 19.56230152254412147, -5.196152422706635576, -5.700000000000065903 ) ) ;
#14089 = CARTESIAN_POINT ( 'NONE',  ( 13.49999999999999645, 195.0125000012290570, -23.38268590217984766 ) ) ;
#14090 = EDGE_LOOP ( 'NONE', ( #19838, #13461 ) ) ;
#14091 = CARTESIAN_POINT ( 'NONE',  ( 11.08355503943142750, 16.16018628210144570, -10.83675517735155225 ) ) ;
#14092 = CARTESIAN_POINT ( 'NONE',  ( -27.24356964375000345, 196.2031250006145342, 0.000000000000000000 ) ) ;
#14093 = CARTESIAN_POINT ( 'NONE',  ( -13.62178482187498396, 198.5843750006145569, 23.59362340125808188 ) ) ;
#14094 = CARTESIAN_POINT ( 'NONE',  ( 16.56230152254411081, -6.928203230275506996, -6.524999998771020771 ) ) ;
#14095 = CARTESIAN_POINT ( 'NONE',  ( -47.00000000000000711, 244.5000000000000000, 5.000000000000000000 ) ) ;
#14096 = CARTESIAN_POINT ( 'NONE',  ( 7.234628195640363302, 195.8174038105676402, -26.99999999999996803 ) ) ;
#14097 = CARTESIAN_POINT ( 'NONE',  ( 15.00000000000000000, 240.1187500012290741, -3.464101615137752610 ) ) ;
#14098 = CARTESIAN_POINT ( 'NONE',  ( 15.24356964374999990, 245.3218750006145399, -3.323476615752268604 ) ) ;
#14099 = CARTESIAN_POINT ( 'NONE',  ( 2.064181346179061460, 114.3023137178985422, 9.465287035748106703 ) ) ;
#14100 = CARTESIAN_POINT ( 'NONE',  ( 15.24356964374999990, 241.3093750006145228, 0.000000000000000000 ) ) ;
#14101 = ORIENTED_EDGE ( 'NONE', *, *, #22629, .T. ) ;
#14102 = CARTESIAN_POINT ( 'NONE',  ( -64.64955436395490551, 214.8429017333601792, -4.673758765035196383 ) ) ;
#14103 = LINE ( 'NONE', #14289, #6899 ) ;
#14104 = CARTESIAN_POINT ( 'NONE',  ( 15.00000000000000178, 248.2937500012290286, 3.464101615137757051 ) ) ;
#14105 = ORIENTED_EDGE ( 'NONE', *, *, #8631, .T. ) ;
#14106 = CARTESIAN_POINT ( 'NONE',  ( -10.69584247140429412, 117.7523137178986019, -6.932735513424201024 ) ) ;
#14107 = CARTESIAN_POINT ( 'NONE',  ( 13.44051670066911264, 5.407089921784862696, -0.2718749993855240632 ) ) ;
#14108 = CARTESIAN_POINT ( 'NONE',  ( 37.05833252405330569, 7.646167579472015790E-16, 161.9106529233149274 ) ) ;
#14109 = CARTESIAN_POINT ( 'NONE',  ( 18.12178482187499640, 4.985214923628404904, -0.3281249993854762348 ) ) ;
#14110 = CARTESIAN_POINT ( 'NONE',  ( -27.00000000000000355, 195.9125000000000796, -15.58845726811989429 ) ) ;
#14111 = ORIENTED_EDGE ( 'NONE', *, *, #22391, .F. ) ;
#14112 = ORIENTED_EDGE ( 'NONE', *, *, #2926, .T. ) ;
#14113 = EDGE_LOOP ( 'NONE', ( #34477, #29010, #3098, #16351 ) ) ;
#14114 = CARTESIAN_POINT ( 'NONE',  ( 18.00000000000000355, -5.196152422706632912, -8.418749998770957532 ) ) ;
#14115 = CARTESIAN_POINT ( 'NONE',  ( 15.24356964375000167, -3.323476615752272600, -1.903124999385467753 ) ) ;
#14116 = DIRECTION ( 'NONE',  ( -0.000000000000000000, 1.000000000000000000, -0.000000000000000000 ) ) ;
#14117 = CARTESIAN_POINT ( 'NONE',  ( 25.28868886033866659, -3.464101615137837431, 167.8622174579674606 ) ) ;
#14118 = CARTESIAN_POINT ( 'NONE',  ( 15.24356964374999990, 247.9468750006145115, 0.000000000000000000 ) ) ;
#14119 = CARTESIAN_POINT ( 'NONE',  ( -12.50000000000000355, 49.51018628210145067, -0.1745138560725492671 ) ) ;
#14120 = ADVANCED_FACE ( 'NONE', ( #5736 ), #11247, .F. ) ;
#14121 = CARTESIAN_POINT ( 'NONE',  ( -60.28794563604516554, 205.3262412349648116, 4.842901733360249317 ) ) ;
#14122 = CARTESIAN_POINT ( 'NONE',  ( 15.31535524866706233, 225.1590526702200634, 1.929602858955283162 ) ) ;
#14123 = CARTESIAN_POINT ( 'NONE',  ( -39.70461230271183695, 208.6787018382582346, -4.469044688360757966 ) ) ;
#14124 = EDGE_CURVE ( 'NONE', #14430, #37491, #31894, .T. ) ;
#14125 = CARTESIAN_POINT ( 'NONE',  ( 36.91619120224290640, 7.347880794884117764E-16, 163.0806184283759706 ) ) ;
#14126 = CARTESIAN_POINT ( 'NONE',  ( 12.53471296425189330, 103.3773137178985735, 2.311890736173451977 ) ) ;
#14127 = CARTESIAN_POINT ( 'NONE',  ( -40.30580436395489841, 216.5000000000000000, 0.1155267958017343610 ) ) ;
#14129 = ADVANCED_FACE ( 'NONE', ( #20351, #31708 ), #3082, .F. ) ;
#14128 = CARTESIAN_POINT ( 'NONE',  ( -44.46205436395490551, 216.1378603801730094, 6.307003348497944195 ) ) ;
#14130 = CARTESIAN_POINT ( 'NONE',  ( 18.12178482187499640, 4.985214923628404904, -3.928124999385496086 ) ) ;
#14131 = CARTESIAN_POINT ( 'NONE',  ( 16.56230152254410726, -6.928203230275506996, -4.274999998770978138 ) ) ;
#14132 = CARTESIAN_POINT ( 'NONE',  ( 13.04141134922778988, 102.2273137178985678, -8.927990412390371944 ) ) ;
#14133 = CARTESIAN_POINT ( 'NONE',  ( -34.55877896937847993, 211.6261429550004607, -6.530955311639245586 ) ) ;
#14134 = ORIENTED_EDGE ( 'NONE', *, *, #10824, .F. ) ;
#14135 = CARTESIAN_POINT ( 'NONE',  ( 20.99999999999999289, 248.8187500012290911, 5.999999999999999112 ) ) ;
#14136 = CARTESIAN_POINT ( 'NONE',  ( 12.53471296425194836, 99.82268628210144357, -2.311890736173178418 ) ) ;
#14137 = CARTESIAN_POINT ( 'NONE',  ( 15.53471296425195369, 72.22268628210143504, -2.908627838312120684 ) ) ;
#14138 = CARTESIAN_POINT ( 'NONE',  ( 15.00000000000000000, 250.0000000000000000, 0.000000000000000000 ) ) ;
#14139 = AXIS2_PLACEMENT_3D ( 'NONE', #33815, #15825, #7667 ) ;
#14140 = CARTESIAN_POINT ( 'NONE',  ( 30.78459393195788607, -7.209453229046482114, 161.8384204035683922 ) ) ;
#14141 = CARTESIAN_POINT ( 'NONE',  ( 15.50000000000000533, 63.31018628210144783, 0.1745138560725827404 ) ) ;
#14142 = CARTESIAN_POINT ( 'NONE',  ( 22.80587116629410360, 3.604726614523238837, -7.078124999385530636 ) ) ;
#14143 =( BOUNDED_CURVE ( )  B_SPLINE_CURVE ( 2, ( #29189, #22780, #29000, #14425, #31853, #26165, #3231, #200, #20120 ),
 .UNSPECIFIED., .F., .F. ) 
 B_SPLINE_CURVE_WITH_KNOTS ( ( 3, 2, 2, 2, 3 ),
 ( 0.4791666666666666852, 0.4861111111111111049, 0.5000000000000000000, 0.5138888888888888395, 0.5208333333333333703 ),
 .UNSPECIFIED. ) 
 CURVE ( )  GEOMETRIC_REPRESENTATION_ITEM ( )  RATIONAL_B_SPLINE_CURVE ( ( 0.9330127018922194093, 0.9330127018922196314, 1.000000000000000000, 0.8660254037844387076, 1.000000000000000000, 0.8660254037844387076, 1.000000000000000000, 0.9330127018922187432, 0.9330127018922192983 ) ) 
 REPRESENTATION_ITEM ( '' )  );
#14144 = CARTESIAN_POINT ( 'NONE',  ( 7.954856959092191815, 27.37268628210144428, 5.529263428287477744 ) ) ;
#14145 = CARTESIAN_POINT ( 'NONE',  ( 20.99999999999999645, 6.928203230275506996, -4.162500000000016520 ) ) ;
#14146 = CARTESIAN_POINT ( 'NONE',  ( -57.72247103062156270, 206.6499508600178672, 5.571401726697986057 ) ) ;
#14147 = CARTESIAN_POINT ( 'NONE',  ( -8.715434833791929847, 50.66018628210144925, -8.962234695871762469 ) ) ;
#14148 = CARTESIAN_POINT ( 'NONE',  ( 5.727106289114498080E-15, 197.8625000000000114, 31.17691453623979214 ) ) ;
#14149 = CARTESIAN_POINT ( 'NONE',  ( 10.56230152254447852, 3.464101615137971546, -6.787500000000034284 ) ) ;
#14150 = CARTESIAN_POINT ( 'NONE',  ( 9.465287035748067623, 17.59768628210143504, 2.064181346179272847 ) ) ;
#14151 = CARTESIAN_POINT ( 'NONE',  ( 23.87821517812499650, 248.3593750006145342, -4.985214923628404904 ) ) ;
#14152 = ORIENTED_EDGE ( 'NONE', *, *, #23212, .F. ) ;
#14153 = CARTESIAN_POINT ( 'NONE',  ( 15.00000000000000178, -3.464101615137757051, -4.912499999999988098 ) ) ;
#14154 = DIRECTION ( 'NONE',  ( 0.9961946980917462113, 0.000000000000000000, -0.08715574274765118534 ) ) ;
#14155 = CARTESIAN_POINT ( 'NONE',  ( 36.97172150469784668, -3.604726614523238837, 160.9206844420862694 ) ) ;
#14156 = CARTESIAN_POINT ( 'NONE',  ( 16.56230152254411081, 7.209453229046475009, -2.953124999385511096 ) ) ;
#14157 = CARTESIAN_POINT ( 'NONE',  ( 28.22540379330944660, -5.407089921784859143, 168.4052071269844930 ) ) ;
#14158 = CARTESIAN_POINT ( 'NONE',  ( 21.00000000000000000, 242.9124999999999943, 6.928203230275506996 ) ) ;
#14159 = CYLINDRICAL_SURFACE ( 'NONE', #4547, 5.999999999999994671 ) ;
#14160 = AXIS2_PLACEMENT_3D ( 'NONE', #21203, #24221, #12841 ) ;
#14161 = CARTESIAN_POINT ( 'NONE',  ( 12.46528703574805874, 72.79768628210145209, 2.660918448318279950 ) ) ;
#14162 = VERTEX_POINT ( 'NONE', #20538 ) ;
#14163 = VERTEX_POINT ( 'NONE', #5923 ) ;
#14164 = CARTESIAN_POINT ( 'NONE',  ( -13.50000000000000533, 196.4375000012290400, -23.38268590217984411 ) ) ;
#14165 = CARTESIAN_POINT ( 'NONE',  ( 20.99999999999999645, 202.0000000000000000, -5.999999999999999112 ) ) ;
#14166 = CARTESIAN_POINT ( 'NONE',  ( 2.908627838312458636, 36.67731371789854933, -15.53471296425188442 ) ) ;
#14167 = CARTESIAN_POINT ( 'NONE',  ( 18.12178482187499640, 4.985214923628404904, -8.878124999385478944 ) ) ;
#14168 = CARTESIAN_POINT ( 'NONE',  ( 26.75643035624999655, 242.4718750006145456, -3.323476615752271712 ) ) ;
#14169 =( BOUNDED_CURVE ( )  B_SPLINE_CURVE ( 2, ( #30619, #8052, #34381, #31174, #24917, #1978, #10510 ),
 .UNSPECIFIED., .F., .F. ) 
 B_SPLINE_CURVE_WITH_KNOTS ( ( 3, 2, 2, 3 ),
 ( 0.5869565217391291556, 0.5942028985507233907, 0.6014492753623178478, 0.6086956521739121939 ),
 .UNSPECIFIED. ) 
 CURVE ( )  GEOMETRIC_REPRESENTATION_ITEM ( )  RATIONAL_B_SPLINE_CURVE ( ( 1.000000000000024647, 0.8660254037844140607, 1.000000000000000000, 0.8660254037844387076, 1.000000000000000000, 0.8660254037844551389, 0.9999999999999835687 ) ) 
 REPRESENTATION_ITEM ( '' )  );
#14170 = CARTESIAN_POINT ( 'NONE',  ( -46.63913769728824121, 207.8500491399821613, -3.954877714930864485 ) ) ;
#14171 = DIRECTION ( 'NONE',  ( 0.9961946980917462113, 0.000000000000000000, -0.08715574274765118534 ) ) ;
#14172 = CARTESIAN_POINT ( 'NONE',  ( 37.01420992928731835, 7.646167579472024665E-16, 161.4063293574060083 ) ) ;
#14173 = CARTESIAN_POINT ( 'NONE',  ( 1.715153634034445762, 27.47731371789854649, -9.534712964251895073 ) ) ;
#14174 = SURFACE_STYLE_FILL_AREA ( #11329 ) ;
#14175 = CARTESIAN_POINT ( 'NONE',  ( 23.35209618661503583, 3.999999999999908962, 50.00000000000000000 ) ) ;
#14176 = CARTESIAN_POINT ( 'NONE',  ( -27.24356964374999990, 196.6718750006145342, -15.72908226750537786 ) ) ;
#14177 = CARTESIAN_POINT ( 'NONE',  ( -4.622313124798826500, 13.96481371789853831, 11.61527771782809637 ) ) ;
#14178 = CARTESIAN_POINT ( 'NONE',  ( -45.64955436395490551, 214.8429017333601792, -4.673758765035196383 ) ) ;
#14179 = AXIS2_PLACEMENT_3D ( 'NONE', #20257, #3738, #514 ) ;
#14180 = ORIENTED_EDGE ( 'NONE', *, *, #4835, .F. ) ;
#14181 = CARTESIAN_POINT ( 'NONE',  ( 8.962234695871762469, 62.16018628210144215, -8.715434833791931624 ) ) ;
#14182 = CARTESIAN_POINT ( 'NONE',  ( 28.31649303895732928, 5.196152422706630247, 168.0490378450901687 ) ) ;
#14183 =( GEOMETRIC_REPRESENTATION_CONTEXT ( 3 ) GLOBAL_UNCERTAINTY_ASSIGNED_CONTEXT ( ( #7827 ) ) GLOBAL_UNIT_ASSIGNED_CONTEXT ( ( #25280, #8227, #31337 ) ) REPRESENTATION_CONTEXT ( 'NONE', 'WORKASPACE' ) );
#14184 = ADVANCED_FACE ( 'NONE', ( #14282 ), #37381, .T. ) ;
#14185 = DIRECTION ( 'NONE',  ( 0.000000000000000000, 0.000000000000000000, -1.000000000000000000 ) ) ;
#14186 = CARTESIAN_POINT ( 'NONE',  ( 25.14654753852813229, -3.604726614523244610, 169.0321829630285322 ) ) ;
#14187 = CARTESIAN_POINT ( 'NONE',  ( 26.99999999999999645, -3.464101615137751278, -1.556249998770957044 ) ) ;
#14188 = CARTESIAN_POINT ( 'NONE',  ( 22.80587116629411781, 7.646167579472024665E-16, -9.871874999385521932 ) ) ;
#14189 = CARTESIAN_POINT ( 'NONE',  ( 10.56230152254410370, 3.464101615137757051, -0.03749999999999697325 ) ) ;
#14190 = CARTESIAN_POINT ( 'NONE',  ( 9.534712964251941258, 81.42268628210145209, -1.715153634034235708 ) ) ;
#14191 = CARTESIAN_POINT ( 'NONE',  ( 22.56230152254410370, 7.347880794884117764E-16, -1.012499998771038134 ) ) ;
#14192 = CARTESIAN_POINT ( 'NONE',  ( -11.48171059495397373, 105.2851862821014493, -4.944772684328680334 ) ) ;
#14193 = CARTESIAN_POINT ( 'NONE',  ( 23.99999999999999645, 249.8499999999999943, -5.196152422706631135 ) ) ;
#14194 = FACE_OUTER_BOUND ( 'NONE', #8937, .T. ) ;
#14195 = ORIENTED_EDGE ( 'NONE', *, *, #195, .T. ) ;
#14196 = CARTESIAN_POINT ( 'NONE',  ( 37.01584409946383403, -3.604726614523235284, 161.4250080079951886 ) ) ;
#14197 = CARTESIAN_POINT ( 'NONE',  ( 23.87821517812500005, -4.985214923628404016, -7.190624999385470062 ) ) ;
#14198 = CARTESIAN_POINT ( 'NONE',  ( 27.24356964375000345, 195.1343750006145399, -3.336375036156643733E-15 ) ) ;
#14199 = CARTESIAN_POINT ( 'NONE',  ( 25.14327919817509027, 0.000000000000000000, 168.9948256618500864 ) ) ;
#14200 = CARTESIAN_POINT ( 'NONE',  ( 34.14658591151403755, -5.196152422706635576, 165.8450248343500562 ) ) ;
#14201 = CARTESIAN_POINT ( 'NONE',  ( 0.000000000000000000, 210.0000000000000284, 0.000000000000000000 ) ) ;
#14202 = CARTESIAN_POINT ( 'NONE',  ( 24.00000000000000000, 249.7000000000000171, 5.196152422706629359 ) ) ;
#14203 = CARTESIAN_POINT ( 'NONE',  ( -27.24356964375000345, 198.0031250006145456, 0.000000000000000000 ) ) ;
#14204 = EDGE_CURVE ( 'NONE', #3698, #7363, #28487, .T. ) ;
#14205 = CARTESIAN_POINT ( 'NONE',  ( -11.48171059495408208, 125.5148137178985763, 4.944772684328421875 ) ) ;
#14206 = CARTESIAN_POINT ( 'NONE',  ( -2.311890736173176641, 125.1226862821014691, -12.53471296425194659 ) ) ;
#14207 = ADVANCED_FACE ( 'NONE', ( #23001 ), #34550, .F. ) ;
#14209 = VERTEX_POINT ( 'NONE', #2530 ) ;
#14208 = ORIENTED_EDGE ( 'NONE', *, *, #6109, .T. ) ;
#14210 =( BOUNDED_CURVE ( )  B_SPLINE_CURVE ( 2, ( #2943, #35333, #31756, #9389, #20963, #29276, #32496 ),
 .UNSPECIFIED., .F., .F. ) 
 B_SPLINE_CURVE_WITH_KNOTS ( ( 3, 2, 2, 3 ),
 ( 0.08695652173913033522, 0.09420289855072437601, 0.1014492753623184307, 0.1086956521739124576 ),
 .UNSPECIFIED. ) 
 CURVE ( )  GEOMETRIC_REPRESENTATION_ITEM ( )  RATIONAL_B_SPLINE_CURVE ( ( 1.000000000000001776, 0.8660254037844368202, 1.000000000000000000, 0.8660254037844387076, 1.000000000000000000, 0.8660254037844494768, 0.9999999999999892308 ) ) 
 REPRESENTATION_ITEM ( '' )  );
#14211 = CARTESIAN_POINT ( 'NONE',  ( 26.75643035624999655, 241.0093750006144830, -3.323476615752271712 ) ) ;
#14212 = CARTESIAN_POINT ( 'NONE',  ( 18.00000000000000355, -5.196152422706632912, -2.624999999999988454 ) ) ;
#14213 = CARTESIAN_POINT ( 'NONE',  ( 0.1745138560722461762, 96.18981371789855928, 15.50000000000000533 ) ) ;
#14214 = CARTESIAN_POINT ( 'NONE',  ( -11.48171059495397373, 96.08518628210146062, -4.944772684328680334 ) ) ;
#14215 = CARTESIAN_POINT ( 'NONE',  ( 18.12178482187500350, -4.985214923628407568, -1.078124999385476901 ) ) ;
#14216 = CARTESIAN_POINT ( 'NONE',  ( 5.727106289114498080E-15, 197.5250000012290457, 31.17691453623979214 ) ) ;
#14217 = CARTESIAN_POINT ( 'NONE',  ( 11.48171059495397728, 119.0851862821014606, 4.944772684328674117 ) ) ;
#14218 = CARTESIAN_POINT ( 'NONE',  ( 22.80587116629410716, 7.646167579472015790E-16, -3.965624999385547689 ) ) ;
#14219 = CARTESIAN_POINT ( 'NONE',  ( 15.24356964374999990, 243.4468750006145115, 0.000000000000000000 ) ) ;
#14220 = CARTESIAN_POINT ( 'NONE',  ( 26.99999999999946354, -3.464101615138058143, -2.962500000000024336 ) ) ;
#14221 = CARTESIAN_POINT ( 'NONE',  ( -53.95461230271181563, 208.1428034533959135, -6.469044688360754414 ) ) ;
#14222 = CARTESIAN_POINT ( 'NONE',  ( 4.944772684328679446, 125.9851862821014521, -11.48171059495397373 ) ) ;
#14223 = CARTESIAN_POINT ( 'NONE',  ( 16.56230152254411081, -6.928203230275506996, -3.824999998771013932 ) ) ;
#14224 = EDGE_CURVE ( 'NONE', #22557, #22802, #8289, .T. ) ;
#14225 = CARTESIAN_POINT ( 'NONE',  ( -42.87872103062156981, 203.4690446883607535, 1.626142955000567936 ) ) ;
#14226 = DIRECTION ( 'NONE',  ( 0.000000000000000000, 0.000000000000000000, 1.000000000000000000 ) ) ;
#14227 = CARTESIAN_POINT ( 'NONE',  ( 23.34314575050772333, 3.999999999999902744, 49.89769604716121876 ) ) ;
#14228 = CARTESIAN_POINT ( 'NONE',  ( -15.53471296425195369, 95.22268628210143504, 2.908627838312118019 ) ) ;
#14229 = CARTESIAN_POINT ( 'NONE',  ( -8.715434833791929847, 23.06018628210145138, -8.962234695871762469 ) ) ;
#14230 = DIRECTION ( 'NONE',  ( -0.000000000000000000, -0.000000000000000000, 1.000000000000000000 ) ) ;
#14232 = CARTESIAN_POINT ( 'NONE',  ( 20.99999999999995381, 244.3187500012290627, 5.999999999999998224 ) ) ;
#14231 = VECTOR ( 'NONE', #6502, 1000.000000000000000 ) ;
#14233 = CARTESIAN_POINT ( 'NONE',  ( 6.594114490232313663, 138.0601862821014549, 6.840914352312096547 ) ) ;
#14234 = CARTESIAN_POINT ( 'NONE',  ( 19.68408634441910721, 5.407089921784857367, -2.540624999385538096 ) ) ;
#14235 = CARTESIAN_POINT ( 'NONE',  ( 23.99999999999999645, 245.8562500012290570, -5.196152422706631135 ) ) ;
#14236 = ORIENTED_EDGE ( 'NONE', *, *, #1063, .T. ) ;
#14237 = CARTESIAN_POINT ( 'NONE',  ( 34.49097153452227360, -5.407089921784855591, 168.3840463937848995 ) ) ;
#14238 = ADVANCED_BREP_SHAPE_REPRESENTATION ( '', ( #7513, #17215 ), #16540 ) ;
#14239 = CARTESIAN_POINT ( 'NONE',  ( 5.529263428287477744, 71.07268628210144357, -7.954856959092191815 ) ) ;
#14240 = CARTESIAN_POINT ( 'NONE',  ( 23.87821517812499650, 4.985214923628404904, -0.7406249993854585600 ) ) ;
#14241 = CARTESIAN_POINT ( 'NONE',  ( 23.99999999999999645, 5.196152422706631135, -5.099999999999993427 ) ) ;
#14242 = CARTESIAN_POINT ( 'NONE',  ( -27.24356964374999635, 196.2968750006145342, 15.72908226750539384 ) ) ;
#14243 = FACE_BOUND ( 'NONE', #10148, .T. ) ;
#14244 = EDGE_CURVE ( 'NONE', #11807, #23273, #15811, .T. ) ;
#14245 = DIRECTION ( 'NONE',  ( -1.000000000000000000, -6.123233995736766036E-17, -0.000000000000000000 ) ) ;
#14246 = CARTESIAN_POINT ( 'NONE',  ( 3.796722387233182339, 31.21481371789855430, 8.710071997420207879 ) ) ;
#14247 = CARTESIAN_POINT ( 'NONE',  ( 5.778771075727756162E-15, 198.6218750006145513, 31.45816453501076637 ) ) ;
#14248 = ORIENTED_EDGE ( 'NONE', *, *, #30942, .F. ) ;
#14249 = ORIENTED_EDGE ( 'NONE', *, *, #12641, .F. ) ;
#14250 = CARTESIAN_POINT ( 'NONE',  ( 18.12178482187499640, 249.2218750006145171, -4.985214923628404904 ) ) ;
#14251 = CARTESIAN_POINT ( 'NONE',  ( 4.944772684328420986, 40.41481371789855359, 11.48171059495408208 ) ) ;
#14252 = CARTESIAN_POINT ( 'NONE',  ( 16.56230152254411081, -7.209453229046482114, -8.184374999385489957 ) ) ;
#14253 = CARTESIAN_POINT ( 'NONE',  ( 21.00000000000000000, 6.646953231504538984, -8.465624999385484628 ) ) ;
#14254 = CARTESIAN_POINT ( 'NONE',  ( -8.632099005475794229, 143.0523137178985280, 13.23911966647199812 ) ) ;
#14255 = ORIENTED_EDGE ( 'NONE', *, *, #18908, .F. ) ;
#14256 = CARTESIAN_POINT ( 'NONE',  ( 16.56230152254411792, 7.209453229046482114, -1.659374999385503591 ) ) ;
#14257 = VECTOR ( 'NONE', #14895, 1000.000000000000000 ) ;
#14258 = CARTESIAN_POINT ( 'NONE',  ( -11.61527771782819940, 12.13518628210144534, 4.622313124798574258 ) ) ;
#14259 = CARTESIAN_POINT ( 'NONE',  ( 37.32470226282583781, -3.604726614523238837, 164.9552729693578215 ) ) ;
#14260 = AXIS2_PLACEMENT_3D ( 'NONE', #2729, #8248, #37224 ) ;
#14261 = CARTESIAN_POINT ( 'NONE',  ( -37.72544563604515844, 214.8429017333602360, 4.673758765035156415 ) ) ;
#14262 = FACE_OUTER_BOUND ( 'NONE', #15657, .T. ) ;
#14263 = EDGE_CURVE ( 'NONE', #8199, #17429, #34401, .T. ) ;
#14264 = CARTESIAN_POINT ( 'NONE',  ( -14.96731853674933888, 195.0000000000000853, 22.75028941543422079 ) ) ;
#14265 = CARTESIAN_POINT ( 'NONE',  ( -55.93377896937850124, 208.9097554298617183, 4.530955311639234040 ) ) ;
#14266 = CARTESIAN_POINT ( 'NONE',  ( -41.49330436395490551, 210.1155267958017134, -6.500000000000000888 ) ) ;
#14267 = CARTESIAN_POINT ( 'NONE',  ( 28.30384396178233075, -5.407089921784859143, 169.3017823552670507 ) ) ;
#14268 = ORIENTED_EDGE ( 'NONE', *, *, #27779, .T. ) ;
#14269 = LINE ( 'NONE', #11599, #14305 ) ;
#14270 = CARTESIAN_POINT ( 'NONE',  ( 25.32137226386879902, 3.464101615137695767, 168.2357904697519473 ) ) ;
#14271 = CARTESIAN_POINT ( 'NONE',  ( 13.23911966647199812, 30.35231371789855359, 8.632099005475788900 ) ) ;
#14272 = CARTESIAN_POINT ( 'NONE',  ( -33.17336230271183695, 217.4189793300686233, 4.149950860017807663 ) ) ;
#14273 = CARTESIAN_POINT ( 'NONE',  ( 12.46528703574805874, 17.59768628210143859, 2.660918448318279950 ) ) ;
#14274 = CARTESIAN_POINT ( 'NONE',  ( -8.962234695871760692, 48.36018628210145209, 8.715434833791933400 ) ) ;
#14275 = CARTESIAN_POINT ( 'NONE',  ( 16.56230152254411436, 6.928203230275514990, -4.162500000000017408 ) ) ;
#14276 = ORIENTED_EDGE ( 'NONE', *, *, #27619, .F. ) ;
#14277 = CARTESIAN_POINT ( 'NONE',  ( 27.00000000000001421, 195.2375000000000114, 15.58845726811988897 ) ) ;
#14278 = CARTESIAN_POINT ( 'NONE',  ( -27.24356964374999990, 195.3218750006145399, -15.72908226750537786 ) ) ;
#14279 = CARTESIAN_POINT ( 'NONE',  ( 22.56230152254427779, 3.464101615137667789, -6.487500000000022915 ) ) ;
#14280 = CYLINDRICAL_SURFACE ( 'NONE', #18049, 6.000000000000001776 ) ;
#14281 = CARTESIAN_POINT ( 'NONE',  ( -20.68320042480036491, 194.9994763866750134, -17.35526491262920246 ) ) ;
#14282 = FACE_OUTER_BOUND ( 'NONE', #24556, .T. ) ;
#14283 = AXIS2_PLACEMENT_3D ( 'NONE', #20816, #12077, #20628 ) ;
#14284 = CARTESIAN_POINT ( 'NONE',  ( 26.75643035624999655, 245.1718750006145058, -3.323476615752271712 ) ) ;
#14285 = CARTESIAN_POINT ( 'NONE',  ( 2.064181346179061460, 95.90231371789855075, 9.465287035748106703 ) ) ;
#14286 = CARTESIAN_POINT ( 'NONE',  ( 15.24356964374999990, 240.8593750006145342, 0.000000000000000000 ) ) ;
#14287 = ORIENTED_EDGE ( 'NONE', *, *, #37043, .F. ) ;
#14288 = CARTESIAN_POINT ( 'NONE',  ( -62.27455436395490551, 205.1570982666397356, 4.673758765035198159 ) ) ;
#14289 = CARTESIAN_POINT ( 'NONE',  ( 20.99999999999999645, 185.0294372515228645, -5.999999999999999112 ) ) ;
#14290 = CARTESIAN_POINT ( 'NONE',  ( 15.00000000000000178, 245.5937500012290400, 3.464101615137757051 ) ) ;
#14291 = ORIENTED_EDGE ( 'NONE', *, *, #8678, .T. ) ;
#14292 = CARTESIAN_POINT ( 'NONE',  ( -2.660918448318005058, 109.7023137178985763, -12.46528703574811558 ) ) ;
#14293 = CARTESIAN_POINT ( 'NONE',  ( 10.31873187879411091, -3.604726614523244610, -0.6093749993855241964 ) ) ;
#14294 = CARTESIAN_POINT ( 'NONE',  ( 33.94189035521207387, -5.407089921784855591, 162.1080197958069107 ) ) ;
#14295 = CARTESIAN_POINT ( 'NONE',  ( 15.24356964374999990, 0.000000000000000000, -2.953124999385492444 ) ) ;
#14296 = CARTESIAN_POINT ( 'NONE',  ( -12.50000000000000355, 70.88981371789856212, 0.1745138560722786503 ) ) ;
#14297 = CARTESIAN_POINT ( 'NONE',  ( 13.62178482187499640, 199.2593750006145399, -23.59362340125807123 ) ) ;
#14298 = VERTEX_POINT ( 'NONE', #9534 ) ;
#14299 = ORIENTED_EDGE ( 'NONE', *, *, #10299, .F. ) ;
#14300 = VERTEX_POINT ( 'NONE', #3651 ) ;
#14301 = CARTESIAN_POINT ( 'NONE',  ( 18.00000000000000000, 5.196152422706630247, -6.768749998770945631 ) ) ;
#14302 = CARTESIAN_POINT ( 'NONE',  ( 15.24356964374999990, 3.323476615752268604, -3.328124999385480898 ) ) ;
#14303 = CARTESIAN_POINT ( 'NONE',  ( 26.99999999999999645, 7.347880794884117764E-16, -6.525000000000003020 ) ) ;
#14304 = FACE_OUTER_BOUND ( 'NONE', #20043, .T. ) ;
#14305 = VECTOR ( 'NONE', #23174, 1000.000000000000000 ) ;
#14306 = CARTESIAN_POINT ( 'NONE',  ( -2.660918448318275509, 56.69768628210145067, 12.46528703574805874 ) ) ;
#14307 = CARTESIAN_POINT ( 'NONE',  ( -51.77752896937849414, 213.3500491399821613, 5.571401726697954970 ) ) ;
#14308 = CARTESIAN_POINT ( 'NONE',  ( 14.95628864315848183, 216.0437113568656287, -2.958957796642720961 ) ) ;
#14309 = CARTESIAN_POINT ( 'NONE',  ( -45.44419563604516554, 205.4999999999999716, 0.1155267958017633378 ) ) ;
#14310 = CARTESIAN_POINT ( 'NONE',  ( 33.77726345172796840, 5.196152422706631135, 161.6236498024106822 ) ) ;
#14311 = CARTESIAN_POINT ( 'NONE',  ( -8.715434833792127023, 97.33981371789855075, 8.962234695871568846 ) ) ;
#14312 = CARTESIAN_POINT ( 'NONE',  ( -32.78497103062156981, 204.4285982733020148, -3.350049139982115509 ) ) ;
#14313 = CARTESIAN_POINT ( 'NONE',  ( -47.82663769728823411, 202.5810206699313767, 4.149950860017909804 ) ) ;
#14314 = AXIS2_PLACEMENT_3D ( 'NONE', #6312, #29429, #34925 ) ;
#14315 = CARTESIAN_POINT ( 'NONE',  ( 15.24356964375000167, -3.323476615752272600, -4.715624999385497063 ) ) ;
#14316 = CARTESIAN_POINT ( 'NONE',  ( -27.12178482187499995, 199.7328125009217956, 0.000000000000000000 ) ) ;
#14317 = CARTESIAN_POINT ( 'NONE',  ( -5.770363421894122880, 69.16481371789853938, 14.38691631536194393 ) ) ;
#14318 = CARTESIAN_POINT ( 'NONE',  ( -30.20461230271182274, 208.1428034533959135, -6.469044688360754414 ) ) ;
#14319 = ORIENTED_EDGE ( 'NONE', *, *, #33589, .F. ) ;
#14320 = CARTESIAN_POINT ( 'NONE',  ( 24.94224478302373527, 0.000000000000000000, 163.9023435342771506 ) ) ;
#14321 = CARTESIAN_POINT ( 'NONE',  ( 8.715434833791931624, 110.4601862821014606, 8.962234695871760692 ) ) ;
#14322 = CARTESIAN_POINT ( 'NONE',  ( 13.23911966647218996, 53.24768628210144783, -8.632099005475504683 ) ) ;
#14323 = DIRECTION ( 'NONE',  ( 0.000000000000000000, 0.000000000000000000, 1.000000000000000000 ) ) ;
#14324 = CARTESIAN_POINT ( 'NONE',  ( 24.63341810310133084, 0.000000000000000000, 163.1670866780133906 ) ) ;
#14325 = CARTESIAN_POINT ( 'NONE',  ( -14.38691631536207183, 58.13518628210145067, 5.770363421893814682 ) ) ;
#14326 = VECTOR ( 'NONE', #13510, 1000.000000000000000 ) ;
#14327 = CARTESIAN_POINT ( 'NONE',  ( 16.56230152254411081, -7.209453229046475009, -9.478124999385530103 ) ) ;
#14328 = FACE_OUTER_BOUND ( 'NONE', #15276, .T. ) ;
#14329 = CARTESIAN_POINT ( 'NONE',  ( -54.15997103062156981, 215.5714017266979852, 3.350049139982118618 ) ) ;
#14330 = CARTESIAN_POINT ( 'NONE',  ( 20.99999999999999645, 0.000000000000000000, 50.00000000000000000 ) ) ;
#14331 = CARTESIAN_POINT ( 'NONE',  ( 2.660918448318279950, 33.69768628210145067, -12.46528703574805697 ) ) ;
#14332 = CARTESIAN_POINT ( 'NONE',  ( -27.00000000000000355, 196.8500000000000227, 0.000000000000000000 ) ) ;
#14333 = CARTESIAN_POINT ( 'NONE',  ( 15.00000000000000000, 0.000000000000000000, -3.543749998770939769 ) ) ;
#14334 = CARTESIAN_POINT ( 'NONE',  ( -0.1745138560725182642, 10.41018628210144037, 9.500000000000005329 ) ) ;
#14335 = CARTESIAN_POINT ( 'NONE',  ( 15.24356964374999990, 248.0593750006145228, 0.000000000000000000 ) ) ;
#14336 = VERTEX_POINT ( 'NONE', #18455 ) ;
#14337 = CARTESIAN_POINT ( 'NONE',  ( 15.00000000000000000, 0.000000000000000000, -4.950000000000009948 ) ) ;
#14338 = DIRECTION ( 'NONE',  ( 1.000000000000000000, 0.000000000000000000, 0.000000000000000000 ) ) ;
#14339 = EDGE_CURVE ( 'NONE', #212, #32537, #15762, .T. ) ;
#14340 = CARTESIAN_POINT ( 'NONE',  ( 27.55375985076035761, -5.407089921784865361, 160.7282817348149706 ) ) ;
#14341 = CARTESIAN_POINT ( 'NONE',  ( 13.44051670066911797, -5.407089921784859143, -3.665624999385552751 ) ) ;
#14342 = CARTESIAN_POINT ( 'NONE',  ( 28.51246584124881167, 5.725134610794655465, 159.7765254813093350 ) ) ;
#14343 = CARTESIAN_POINT ( 'NONE',  ( 26.99999999999999645, 240.7374999999999829, 3.464101615137751278 ) ) ;
#14344 = CARTESIAN_POINT ( 'NONE',  ( 5.438367727407757144E-14, 198.5374999999999943, -27.00000000000000000 ) ) ;
#14345 = EDGE_CURVE ( 'NONE', #30675, #37490, #733, .T. ) ;
#14346 = CARTESIAN_POINT ( 'NONE',  ( -8.715434833791929847, 59.86018628210145209, -8.962234695871762469 ) ) ;
#14347 = ORIENTED_EDGE ( 'NONE', *, *, #35174, .T. ) ;
#14348 = VERTEX_POINT ( 'NONE', #24321 ) ;
#14349 = CARTESIAN_POINT ( 'NONE',  ( 20.99999999999999645, 185.0294372515228645, 5.999999999999999112 ) ) ;
#14350 = CARTESIAN_POINT ( 'NONE',  ( -27.00000000000000355, 196.0250000012290457, -15.58845726811989429 ) ) ;
#14351 = DIRECTION ( 'NONE',  ( 0.08715574274764675833, 0.000000000000000000, 0.9961946980917465444 ) ) ;
#14352 = CONICAL_SURFACE ( 'NONE', #36422, 5.999999999999998224, 0.2617993877991499074 ) ;
#14353 = CARTESIAN_POINT ( 'NONE',  ( -14.38691631536193860, 43.86481371789854933, -5.770363421894132649 ) ) ;
#14354 = DIRECTION ( 'NONE',  ( 0.9961946980917462113, 0.000000000000000000, -0.08715574274765118534 ) ) ;
#14355 = CARTESIAN_POINT ( 'NONE',  ( 15.24356964374999990, 243.5593750006145228, 0.000000000000000000 ) ) ;
#14356 = CARTESIAN_POINT ( 'NONE',  ( -45.45163769728823411, 213.9548777149308592, -2.149950860017830756 ) ) ;
#14357 = AXIS2_PLACEMENT_3D ( 'NONE', #3718, #4281, #35929 ) ;
#14358 = CYLINDRICAL_SURFACE ( 'NONE', #27645, 5.999999999999998224 ) ;
#14359 = CARTESIAN_POINT ( 'NONE',  ( 33.83240095338533848, 5.407089921784862696, 160.8565502063291603 ) ) ;
#14360 = CARTESIAN_POINT ( 'NONE',  ( 8.843639120294245259, 11.66481371789854293, 3.474262827703527901 ) ) ;
#14361 = CARTESIAN_POINT ( 'NONE',  ( -66.43080436395490551, 203.5000000000000000, -0.1155267958017335561 ) ) ;
#14362 = CARTESIAN_POINT ( 'NONE',  ( 16.25535974507127790, 195.0000000000000000, 21.84619082737673068 ) ) ;
#14363 = CARTESIAN_POINT ( 'NONE',  ( -13.62178482187500528, 195.2843750006145456, -23.59362340125807123 ) ) ;
#14364 = CARTESIAN_POINT ( 'NONE',  ( -14.25334919248795096, 134.7148137178985507, 6.092822981423662299 ) ) ;
#14365 = VERTEX_POINT ( 'NONE', #12373 ) ;
#14366 =( BOUNDED_CURVE ( )  B_SPLINE_CURVE ( 2, ( #15587, #35850, #33206, #21475, #33014, #4202, #15779, #24119, #23930 ),
 .UNSPECIFIED., .F., .F. ) 
 B_SPLINE_CURVE_WITH_KNOTS ( ( 3, 2, 2, 2, 3 ),
 ( 0.8152173913043478937, 0.8188405797101449002, 0.8260869565217391353, 0.8333333333333333703, 0.8369565217391303769 ),
 .UNSPECIFIED. ) 
 CURVE ( )  GEOMETRIC_REPRESENTATION_ITEM ( )  RATIONAL_B_SPLINE_CURVE ( ( 0.9330127018922192983, 0.9330127018922202975, 1.000000000000000000, 0.8660254037844387076, 1.000000000000000000, 0.8660254037844387076, 1.000000000000000000, 0.9330127018922202975, 0.9330127018922192983 ) ) 
 REPRESENTATION_ITEM ( '' )  );
#14367 = CARTESIAN_POINT ( 'NONE',  ( 2.311890736173175753, 37.72268628210144215, 12.53471296425194836 ) ) ;
#14368 = CARTESIAN_POINT ( 'NONE',  ( 13.56230152254411436, -5.196152422706632912, -8.362499998771033560 ) ) ;
#14369 = CARTESIAN_POINT ( 'NONE',  ( 3.306546357697853733E-15, 210.0000000000000284, 27.00000000000000000 ) ) ;
#14370 = CARTESIAN_POINT ( 'NONE',  ( 25.14327919817509027, 0.000000000000000000, 168.9948256618500864 ) ) ;
#14371 = CARTESIAN_POINT ( 'NONE',  ( 23.99999999999999645, 5.196152422706631135, -2.343749998770960907 ) ) ;
#14372 = CARTESIAN_POINT ( 'NONE',  ( 13.44051670066911264, -5.407089921784865361, -8.671874999385515537 ) ) ;
#14373 = CARTESIAN_POINT ( 'NONE',  ( 16.56230152254411792, 6.928203230275514990, -0.1125000000000229705 ) ) ;
#14374 = CARTESIAN_POINT ( 'NONE',  ( 8.710071997420127943, 73.08518628210143220, 3.796722387233375073 ) ) ;
#14375 = CARTESIAN_POINT ( 'NONE',  ( -4.622313124798576922, 97.23518628210145209, -11.61527771782819762 ) ) ;
#14376 = DIRECTION ( 'NONE',  ( 0.08715574274765150453, 0.000000000000000000, 0.9961946980917461003 ) ) ;
#14377 = CARTESIAN_POINT ( 'NONE',  ( 7.234628195640309123, 198.6299038117966802, -27.00000000000000711 ) ) ;
#14378 = ORIENTED_EDGE ( 'NONE', *, *, #12185, .F. ) ;
#14379 = CARTESIAN_POINT ( 'NONE',  ( 27.79398286670857132, -5.407089921784859143, 163.4740433714303265 ) ) ;
#14380 = CARTESIAN_POINT ( 'NONE',  ( 21.00000000000000000, 6.646953231504538984, -7.003124999385472726 ) ) ;
#14381 = CARTESIAN_POINT ( 'NONE',  ( -27.24356964375000345, 196.2218750006145456, -15.72908226750537786 ) ) ;
#14382 = CARTESIAN_POINT ( 'NONE',  ( 37.48485094012463748, 7.646167579472024665E-16, 166.7857807271014394 ) ) ;
#14383 = CARTESIAN_POINT ( 'NONE',  ( 37.14497502684837826, 3.464101615137759271, 165.6956295096424299 ) ) ;
#14384 = CARTESIAN_POINT ( 'NONE',  ( 22.56230152254411792, 7.347880794884125653E-16, -6.075000000000052580 ) ) ;
#14385 = CARTESIAN_POINT ( 'NONE',  ( 26.75643035624999655, 240.1468750006145285, 3.323476615752267715 ) ) ;
#14386 = CARTESIAN_POINT ( 'NONE',  ( -27.24356964375000345, 198.4156250006145399, -15.72908226750537786 ) ) ;
#14387 =( BOUNDED_CURVE ( )  B_SPLINE_CURVE ( 2, ( #32525, #7141, #6568, #15290, #15858, #21176, #26842, #9971, #32715 ),
 .UNSPECIFIED., .F., .F. ) 
 B_SPLINE_CURVE_WITH_KNOTS ( ( 3, 2, 2, 2, 3 ),
 ( 0.4239130434782608647, 0.4275362318840579823, 0.4347826086956521618, 0.4420289855072463969, 0.4456521739130434590 ),
 .UNSPECIFIED. ) 
 CURVE ( )  GEOMETRIC_REPRESENTATION_ITEM ( )  RATIONAL_B_SPLINE_CURVE ( ( 0.9330127018922194093, 0.9330127018922194093, 1.000000000000000000, 0.8660254037844387076, 1.000000000000000000, 0.8660254037844387076, 1.000000000000000000, 0.9330127018922198534, 0.9330127018922191873 ) ) 
 REPRESENTATION_ITEM ( '' )  );
#14388 = CARTESIAN_POINT ( 'NONE',  ( 7.228626920338837358, 113.7273137178985820, 10.49813415416005036 ) ) ;
#14389 = CARTESIAN_POINT ( 'NONE',  ( 10.69584247140445221, 126.8476862821014635, -6.932735513423970097 ) ) ;
#14391 = VERTEX_POINT ( 'NONE', #30188 ) ;
#14390 = EDGE_LOOP ( 'NONE', ( #32318, #14500, #12352, #29293 ) ) ;
#14392 = CARTESIAN_POINT ( 'NONE',  ( -13.62178482187498396, 198.9781250006145399, 23.59362340125808188 ) ) ;
#14393 = CARTESIAN_POINT ( 'NONE',  ( 26.75643035624999655, 243.1843750006144944, 3.323476615752267715 ) ) ;
#14394 = CARTESIAN_POINT ( 'NONE',  ( 26.99999999999976197, -3.464101615137889834, -2.512499999999992628 ) ) ;
#14395 = CARTESIAN_POINT ( 'NONE',  ( -11.08355503943118592, 99.63981371789857633, -10.83675517735179383 ) ) ;
#14396 = CARTESIAN_POINT ( 'NONE',  ( 23.87821517812500005, -4.985214923628404016, -2.353124999385475036 ) ) ;
#14397 = PRODUCT_DEFINITION_SHAPE ( 'NONE', 'NONE',  #18078 ) ;
#14398 = CARTESIAN_POINT ( 'NONE',  ( 13.49999999999999645, 197.2625000012290286, -23.38268590217984766 ) ) ;
#14399 = CARTESIAN_POINT ( 'NONE',  ( -2.064181346179062349, 82.10231371789853938, -9.465287035748106703 ) ) ;
#14400 = CARTESIAN_POINT ( 'NONE',  ( 10.31873187879410914, 0.000000000000000000, -3.740624999385516958 ) ) ;
#14401 = CARTESIAN_POINT ( 'NONE',  ( 20.99999999999999645, 241.7593750006145115, 6.646953231504538984 ) ) ;
#14402 = CARTESIAN_POINT ( 'NONE',  ( 8.715434833792128799, 74.33981371789855075, -8.962234695871567070 ) ) ;
#14403 = CIRCLE ( 'NONE', #32553, 2.649999999999992806 ) ;
#14404 = LINE ( 'NONE', #30531, #27287 ) ;
#14405 = CARTESIAN_POINT ( 'NONE',  ( 2.311890736173175753, 111.3226862821014720, 12.53471296425194836 ) ) ;
#14406 = CARTESIAN_POINT ( 'NONE',  ( 22.56230152254412147, -3.464101615137751278, -3.299999998771024678 ) ) ;
#14407 = CARTESIAN_POINT ( 'NONE',  ( -38.92038769728823411, 208.1428034533959703, 6.469044688360770401 ) ) ;
#14408 = CARTESIAN_POINT ( 'NONE',  ( 24.00000000000000000, 239.8562500012290286, 5.196152422706629359 ) ) ;
#14409 = DIRECTION ( 'NONE',  ( -1.000000000000000000, -4.130293990420971855E-17, 0.000000000000000000 ) ) ;
#14410 = AXIS2_PLACEMENT_3D ( 'NONE', #29801, #3835, #24130 ) ;
#14411 = CARTESIAN_POINT ( 'NONE',  ( -14.38691631536207183, 104.1351862821014720, 5.770363421893814682 ) ) ;
#14412 = CARTESIAN_POINT ( 'NONE',  ( -12.50000000000000355, 21.91018628210143859, -0.1745138560725492671 ) ) ;
#14413 = DIRECTION ( 'NONE',  ( 0.08715574274765150453, 0.000000000000000000, 0.9961946980917461003 ) ) ;
#14414 = FACE_OUTER_BOUND ( 'NONE', #34198, .T. ) ;
#14415 = CARTESIAN_POINT ( 'NONE',  ( 8.843639120294328748, 127.1351862821014720, -3.474262827703334722 ) ) ;
#14416 = CARTESIAN_POINT ( 'NONE',  ( 33.85570362020085611, 5.196152422706631135, 162.5202250306932399 ) ) ;
#14417 = VERTEX_POINT ( 'NONE', #35675 ) ;
#14418 = CARTESIAN_POINT ( 'NONE',  ( 37.57146195948011069, 3.604726614523238837, 167.7757492083300690 ) ) ;
#14419 = CARTESIAN_POINT ( 'NONE',  ( -3.474262827703337830, 69.63518628210144357, -8.843639120294326972 ) ) ;
#14420 =( BOUNDED_CURVE ( )  B_SPLINE_CURVE ( 2, ( #15080, #29665, #12610, #27383, #23993, #21156, #15460 ),
 .UNSPECIFIED., .F., .F. ) 
 B_SPLINE_CURVE_WITH_KNOTS ( ( 3, 2, 2, 3 ),
 ( 0.4130434782608697342, 0.4202898550724640248, 0.4275362318840583153, 0.4347826086956526059 ),
 .UNSPECIFIED. ) 
 CURVE ( )  GEOMETRIC_REPRESENTATION_ITEM ( )  RATIONAL_B_SPLINE_CURVE ( ( 0.9999999999999968914, 0.8660254037844418162, 1.000000000000000000, 0.8660254037844387076, 1.000000000000000000, 0.8660254037844304920, 1.000000000000008216 ) ) 
 REPRESENTATION_ITEM ( '' )  );
#14421 = CARTESIAN_POINT ( 'NONE',  ( 21.00000000000000355, 0.000000000000000000, 50.00000000000001421 ) ) ;
#14422 = CARTESIAN_POINT ( 'NONE',  ( 22.60769515458670753, 241.3174038105676686, -6.000000000000011546 ) ) ;
#14423 = CARTESIAN_POINT ( 'NONE',  ( 18.00000000000000355, 242.4812500012290570, 5.196152422706632912 ) ) ;
#14424 = CARTESIAN_POINT ( 'NONE',  ( 27.24356964375000700, 195.0968750006145456, 15.72908226750537075 ) ) ;
#14425 = CARTESIAN_POINT ( 'NONE',  ( -26.99999999999999645, 197.0000000012290116, 15.58845726811991561 ) ) ;
#14427 = CLOSED_SHELL ( 'NONE', ( #2736, #20332, #27945, #1359, #30209, #16354, #31709, #15672, #5903, #20150, #14665, #2887, #27519, #1763, #4292, #33464, #3539, #6864, #6608, #6935, #16660, #14464, #14927, #27932, #29080, #26315, #18772, #36037, #28781, #29607, #27662, #3415, #18545, #25118, #2519, #35997, #36575, #23162, #10614, #33764, #22857, #7558, #14184, #33048, #15222, #1718, #6153, #29167, #16117, #21757, #14509, #35067, #12384, #12287, #23127, #5981, #32600, #7066, #21420, #13174, #5488, #20307, #31352, #29870, #13075, #4542, #30497, #12272, #26735, #6172, #17476, #14730, #36725, #33751, #17858, #22061, #9835, #37139, #23624, #14447, #27559, #35329, #2474, #25240, #14689, #30892, #21074, #24201, #3519, #17262, #7878, #19922, #11936, #36997, #20346, #32790, #15404, #5625, #20608, #32521, #2404, #24785, #15966 ) ) ;
#14426 = CARTESIAN_POINT ( 'NONE',  ( -3.796722387233185003, 35.81481371789853796, -8.710071997420207879 ) ) ;
#14428 = CARTESIAN_POINT ( 'NONE',  ( -13.62178482187500528, 198.4343750006145228, -23.59362340125807123 ) ) ;
#14429 = CIRCLE ( 'NONE', #35606, 27.00000000000000355 ) ;
#14430 = VERTEX_POINT ( 'NONE', #3460 ) ;
#14431 = VERTEX_POINT ( 'NONE', #6500 ) ;
#14432 = CARTESIAN_POINT ( 'NONE',  ( 23.87821517812499650, 248.2468750006145228, -4.985214923628404904 ) ) ;
#14433 = CARTESIAN_POINT ( 'NONE',  ( 12.50000000000000355, 38.68981371789855217, -0.1745138560722771515 ) ) ;
#14434 = CARTESIAN_POINT ( 'NONE',  ( 22.80587116629411426, 3.604726614523243278, -7.584374999385505411 ) ) ;
#14435 = CARTESIAN_POINT ( 'NONE',  ( 26.75643035624999655, 7.049594010296217766E-16, -0.3656249993854721048 ) ) ;
#14436 = CARTESIAN_POINT ( 'NONE',  ( -5.770363421894122880, 142.7648137178985621, 14.38691631536194393 ) ) ;
#14437 = EDGE_LOOP ( 'NONE', ( #4581, #34907, #16592, #12146 ) ) ;
#14438 = CARTESIAN_POINT ( 'NONE',  ( 10.31873187879410381, 3.604726614523240613, -2.934374999385496618 ) ) ;
#14439 = CARTESIAN_POINT ( 'NONE',  ( 27.24356964375000345, 199.5781250006145342, -3.336375036156643733E-15 ) ) ;
#14440 = CARTESIAN_POINT ( 'NONE',  ( 34.28996860281051795, -5.407089921784861808, 166.0865723713108366 ) ) ;
#14441 = CARTESIAN_POINT ( 'NONE',  ( -45.44419563604516554, 203.5000000000000000, 0.1155267958017914542 ) ) ;
#14442 = CARTESIAN_POINT ( 'NONE',  ( 26.75643035624999655, 249.1093750006145058, -3.323476615752271268 ) ) ;
#14443 = FILL_AREA_STYLE_COLOUR ( '', #15373 ) ;
#14444 = CARTESIAN_POINT ( 'NONE',  ( -24.36897002145979485, 195.0000000000000284, 12.00491919322965195 ) ) ;
#14445 = CARTESIAN_POINT ( 'NONE',  ( -54.35044563604515844, 206.6211998817775566, -3.209657149897419348 ) ) ;
#14447 = ADVANCED_FACE ( 'NONE', ( #26770 ), #18074, .T. ) ;
#14446 = CARTESIAN_POINT ( 'NONE',  ( -38.72247103062156981, 206.6499508600178672, 5.571401726697986057 ) ) ;
#14448 = CARTESIAN_POINT ( 'NONE',  ( 31.41701779027052766, -7.209453229046475009, 169.0670581815966216 ) ) ;
#14449 = ORIENTED_EDGE ( 'NONE', *, *, #11549, .T. ) ;
#14450 = CARTESIAN_POINT ( 'NONE',  ( 15.00000000000000000, 3.464101615137752610, -0.4312499987709516591 ) ) ;
#14451 = CARTESIAN_POINT ( 'NONE',  ( 14.38691631536194393, 20.86481371789854578, 5.770363421894124656 ) ) ;
#14452 = CARTESIAN_POINT ( 'NONE',  ( -55.54538769728824832, 212.3930949314662371, -8.469044688360781947 ) ) ;
#14453 = CARTESIAN_POINT ( 'NONE',  ( 11.48171059495397728, 8.685186282101437172, 4.944772684328674117 ) ) ;
#14454 = CARTESIAN_POINT ( 'NONE',  ( 6.932735513423970097, 55.54768628210144499, 10.69584247140445044 ) ) ;
#14456 = EDGE_CURVE ( 'NONE', #7551, #22746, #4612, .T. ) ;
#14455 = CARTESIAN_POINT ( 'NONE',  ( 22.56230152254412857, -3.464101615137755275, -3.862500000000040679 ) ) ;
#14457 = EDGE_LOOP ( 'NONE', ( #23343, #34011, #17241, #29201, #7127, #23155 ) ) ;
#14458 = CARTESIAN_POINT ( 'NONE',  ( -46.04538769728823411, 211.8571965466040012, -6.469044688360769513 ) ) ;
#14459 = DIRECTION ( 'NONE',  ( 0.000000000000000000, -0.000000000000000000, -1.000000000000000000 ) ) ;
#14460 = CARTESIAN_POINT ( 'NONE',  ( -1.926257025242585782E-15, 196.1468750006145285, -31.45816453501075927 ) ) ;
#14461 = CARTESIAN_POINT ( 'NONE',  ( 37.26917196037089042, 7.347880794884117764E-16, 167.1152069556475510 ) ) ;
#14462 = DIRECTION ( 'NONE',  ( -1.000000000000000000, 0.000000000000000000, -0.000000000000000000 ) ) ;
#14463 = CARTESIAN_POINT ( 'NONE',  ( 15.02283181144952628, 7.347880794884122694E-16, 50.52293445648592751 ) ) ;
#14464 = ADVANCED_FACE ( 'NONE', ( #17881 ), #29616, .T. ) ;
#14465 = CARTESIAN_POINT ( 'NONE',  ( 20.99999999999997513, 246.3437500012290684, -5.999999999999999112 ) ) ;
#14466 = CARTESIAN_POINT ( 'NONE',  ( 18.12178482187500350, 245.8843750006145115, 4.985214923628407568 ) ) ;
#14467 = CARTESIAN_POINT ( 'NONE',  ( -1.715153634034442431, 96.47731371789852517, 9.534712964251900402 ) ) ;
#14468 = CARTESIAN_POINT ( 'NONE',  ( 18.12178482187499640, 242.1343750006145115, -4.985214923628404904 ) ) ;
#14469 = VERTEX_POINT ( 'NONE', #18260 ) ;
#14470 = CARTESIAN_POINT ( 'NONE',  ( -58.31622103062155560, 211.6261429550005744, 6.530955311639227823 ) ) ;
#14471 = CARTESIAN_POINT ( 'NONE',  ( 37.11229162342512211, 7.347880794884117764E-16, 165.3220564990824073 ) ) ;
#14472 = ADVANCED_FACE ( 'NONE', ( #6689 ), #9905, .F. ) ;
#14473 = CARTESIAN_POINT ( 'NONE',  ( 26.99999999999999645, 246.6812500012290457, -7.347880794884117764E-16 ) ) ;
#14474 = ORIENTED_EDGE ( 'NONE', *, *, #35373, .T. ) ;
#14475 = CARTESIAN_POINT ( 'NONE',  ( 8.962234695871567070, 104.2398137178985564, 8.715434833792127023 ) ) ;
#14476 = CARTESIAN_POINT ( 'NONE',  ( 10.31873187879410914, 0.000000000000000000, -2.446874999385534544 ) ) ;
#14477 = CARTESIAN_POINT ( 'NONE',  ( 27.54558899987776144, 5.407089921784856479, 160.6348884818688418 ) ) ;
#14478 = CARTESIAN_POINT ( 'NONE',  ( 15.24356964374999990, 0.000000000000000000, -1.153124999385496396 ) ) ;
#14479 = CARTESIAN_POINT ( 'NONE',  ( 4.622313124798831829, 64.56481371789855928, -11.61527771782809282 ) ) ;
#14480 = CARTESIAN_POINT ( 'NONE',  ( -20.68320088531713452, 194.9994763905949924, -17.35526436380663284 ) ) ;
#14481 = ORIENTED_EDGE ( 'NONE', *, *, #1630, .T. ) ;
#14482 = ORIENTED_EDGE ( 'NONE', *, *, #31242, .T. ) ;
#14483 = ORIENTED_EDGE ( 'NONE', *, *, #2176, .F. ) ;
#14484 = CARTESIAN_POINT ( 'NONE',  ( 15.00000000000000178, -3.464101615137757051, -7.106249998770957532 ) ) ;
#14485 = CARTESIAN_POINT ( 'NONE',  ( 26.75643035624999655, 7.049594010296217766E-16, -5.765624999385460470 ) ) ;
#14486 = CARTESIAN_POINT ( 'NONE',  ( 26.75643035624999655, 246.7843750006145171, 3.323476615752267715 ) ) ;
#14487 = CARTESIAN_POINT ( 'NONE',  ( -2.311890736173176641, 42.32268628210145067, -12.53471296425194836 ) ) ;
#14488 = CARTESIAN_POINT ( 'NONE',  ( -55.14211230271182984, 203.5309553116391896, 1.857196546604092724 ) ) ;
#14489 = CARTESIAN_POINT ( 'NONE',  ( 8.278277990405213060, 214.7706457535942661, -3.659938751172172822 ) ) ;
#14490 = CARTESIAN_POINT ( 'NONE',  ( -45.04836230271183695, 206.0451222850691977, -2.149950860017851184 ) ) ;
#14491 = CARTESIAN_POINT ( 'NONE',  ( 33.88185034302515675, -5.196152422706629359, 162.8190834401207496 ) ) ;
#14492 = CARTESIAN_POINT ( 'NONE',  ( -0.1745138560722763466, 109.9898137178985706, -12.50000000000000355 ) ) ;
#14493 = CARTESIAN_POINT ( 'NONE',  ( -54.35788769728822700, 214.4690446883608104, 1.321298161741840893 ) ) ;
#14494 = CARTESIAN_POINT ( 'NONE',  ( -40.30580436395490551, 218.5000000000000000, 0.1155267958017064944 ) ) ;
#14495 = CARTESIAN_POINT ( 'NONE',  ( 20.99999999999999645, -6.646953231504538984, -3.740624999385479654 ) ) ;
#14496 = LINE ( 'NONE', #23591, #8329 ) ;
#14497 = CARTESIAN_POINT ( 'NONE',  ( 8.927990412390371944, 76.92731371789854222, 13.04141134922778811 ) ) ;
#14498 = CARTESIAN_POINT ( 'NONE',  ( -55.73586230271182984, 205.8500491399821613, 7.418979330068642852 ) ) ;
#14499 = EDGE_CURVE ( 'NONE', #11470, #1148, #21109, .T. ) ;
#14500 = ORIENTED_EDGE ( 'NONE', *, *, #33533, .T. ) ;
#14501 = CARTESIAN_POINT ( 'NONE',  ( 26.99999999999999645, 248.9687500012290116, -3.464101615137755275 ) ) ;
#14502 = CARTESIAN_POINT ( 'NONE',  ( 4.622313124798573369, 111.0351862821014635, 11.61527771782819940 ) ) ;
#14503 = CARTESIAN_POINT ( 'NONE',  ( 15.50000000000000533, 54.11018628210144499, 0.1745138560725827404 ) ) ;
#14505 = EDGE_CURVE ( 'NONE', #15610, #22453, #3837, .T. ) ;
#14504 = CARTESIAN_POINT ( 'NONE',  ( 15.00000000000000000, 243.2125000000000057, -3.464101615137752610 ) ) ;
#14506 = CARTESIAN_POINT ( 'NONE',  ( 30.72576380560321851, 7.209453229046482114, 161.1659889823564811 ) ) ;
#14507 = CARTESIAN_POINT ( 'NONE',  ( 15.50000000000000533, 72.51018628210145778, 0.1745138560725827404 ) ) ;
#14508 = CARTESIAN_POINT ( 'NONE',  ( -26.99999999999999645, 194.7500000012290400, 15.58845726811991561 ) ) ;
#14509 = ADVANCED_FACE ( 'NONE', ( #35485 ), #15600, .T. ) ;
#14510 = CARTESIAN_POINT ( 'NONE',  ( 10.31873187879411091, -3.604726614523240613, -10.00312499938551802 ) ) ;
#14511 = CYLINDRICAL_SURFACE ( 'NONE', #12211, 5.999999999999999112 ) ;
#14512 = CARTESIAN_POINT ( 'NONE',  ( -44.46205436395488420, 214.6737587650352168, 4.842901733360204908 ) ) ;
#14513 = CARTESIAN_POINT ( 'NONE',  ( 15.00000000000000000, 249.0625000000000000, -3.464101615137752610 ) ) ;
#14514 = CARTESIAN_POINT ( 'NONE',  ( 12.46528703574805874, 45.19768628210143646, 2.660918448318279950 ) ) ;
#14515 = CARTESIAN_POINT ( 'NONE',  ( 5.727106289114498080E-15, 196.5125000000000171, 31.17691453623979214 ) ) ;
#14516 = CARTESIAN_POINT ( 'NONE',  ( 20.99999999999999645, 6.928203230275506996, -3.656249998770947585 ) ) ;
#14517 = CARTESIAN_POINT ( 'NONE',  ( -8.710071997420207879, 143.9148137178985678, 3.796722387233182339 ) ) ;
#14518 = CARTESIAN_POINT ( 'NONE',  ( 20.99999999999999645, 249.2968750006145342, -6.646953231504538984 ) ) ;
#14519 = EDGE_LOOP ( 'NONE', ( #13364, #3521, #23713, #29150 ) ) ;
#14520 = CARTESIAN_POINT ( 'NONE',  ( 18.00000000000000355, -5.196152422706632912, -5.324999999999996625 ) ) ;
#14521 = LINE ( 'NONE', #35156, #14257 ) ;
#14522 = CARTESIAN_POINT ( 'NONE',  ( 36.88023945835897166, 3.464101615138061696, 162.6696881154131802 ) ) ;
#14523 = CARTESIAN_POINT ( 'NONE',  ( 19.68408634441911076, 5.407089921784857367, -5.240624999385545379 ) ) ;
#14524 = CARTESIAN_POINT ( 'NONE',  ( 34.34716455898865206, 5.407089921784857367, 166.7403251419335390 ) ) ;
#14525 = CARTESIAN_POINT ( 'NONE',  ( 23.99999999999999645, 240.4000000000000057, -5.196152422706631135 ) ) ;
#14526 = CARTESIAN_POINT ( 'NONE',  ( 15.00000000000000000, 0.000000000000000000, -0.8437499987709595750 ) ) ;
#14527 = CARTESIAN_POINT ( 'NONE',  ( 11.48171059495397728, 73.08518628210144641, 4.944772684328674117 ) ) ;
#14528 = ORIENTED_EDGE ( 'NONE', *, *, #14038, .T. ) ;
#14529 = ORIENTED_EDGE ( 'NONE', *, *, #9234, .T. ) ;
#14530 = CARTESIAN_POINT ( 'NONE',  ( 36.59916218799779841, -3.464101615138058143, 159.4569602140672657 ) ) ;
#14531 = CARTESIAN_POINT ( 'NONE',  ( -26.99999999999998934, 195.2000000012290286, 15.58845726811991561 ) ) ;
#14532 = CARTESIAN_POINT ( 'NONE',  ( 36.74623750377856624, -3.464101615137356927, 161.1380387658726931 ) ) ;
#14533 = CARTESIAN_POINT ( 'NONE',  ( 15.24356964374999990, 3.323476615752268604, -6.928124999385478766 ) ) ;
#14534 = VECTOR ( 'NONE', #26960, 1000.000000000000000 ) ;
#14535 = PRODUCT_DEFINITION_CONTEXT ( 'detailed design', #14628, 'design' ) ;
#14536 = CARTESIAN_POINT ( 'NONE',  ( 8.927990412390371944, 40.12731371789853796, 13.04141134922778811 ) ) ;
#14537 = CARTESIAN_POINT ( 'NONE',  ( 26.99999999999999645, 7.347880794884117764E-16, -4.218749998770948473 ) ) ;
#14538 = CARTESIAN_POINT ( 'NONE',  ( 25.20371201115935733, 3.464101615137634038, 166.8909276273280398 ) ) ;
#14539 = CARTESIAN_POINT ( 'NONE',  ( -39.11830436395489841, 209.8844732041982297, 4.499999999999996447 ) ) ;
#14540 = DIRECTION ( 'NONE',  ( 0.08715574274765150453, 0.000000000000000000, 0.9961946980917461003 ) ) ;
#14541 = CARTESIAN_POINT ( 'NONE',  ( 25.44883753774445978, 3.464101615137752166, 169.6927252169354290 ) ) ;
#14542 = CARTESIAN_POINT ( 'NONE',  ( -2.064181346179062349, 26.90231371789854364, -9.465287035748106703 ) ) ;
#14543 = CARTESIAN_POINT ( 'NONE',  ( -57.72247103062156270, 206.6499508600178672, 5.571401726697986057 ) ) ;
#14544 = DIRECTION ( 'NONE',  ( 0.000000000000000000, 0.000000000000000000, 1.000000000000000000 ) ) ;
#14545 =( GEOMETRIC_REPRESENTATION_CONTEXT ( 3 ) GLOBAL_UNCERTAINTY_ASSIGNED_CONTEXT ( ( #16549 ) ) GLOBAL_UNIT_ASSIGNED_CONTEXT ( ( #24444, #24992, #36549 ) ) REPRESENTATION_CONTEXT ( 'NONE', 'WORKASPACE' ) );
#14546 = CARTESIAN_POINT ( 'NONE',  ( 15.80494806997313439, 195.0000000000000284, 22.17725129625731029 ) ) ;
#14547 = CARTESIAN_POINT ( 'NONE',  ( -27.24356964374999635, 194.9468750006145399, 15.72908226750539384 ) ) ;
#14548 = CARTESIAN_POINT ( 'NONE',  ( -6.092822981423666739, 127.8148137178985735, -14.25334919248795096 ) ) ;
#14549 = EDGE_CURVE ( 'NONE', #3075, #27300, #12943, .T. ) ;
#14550 = VERTEX_POINT ( 'NONE', #32266 ) ;
#14551 = CARTESIAN_POINT ( 'NONE',  ( 7.228626920339068285, 43.47268628210144925, -10.49813415415989581 ) ) ;
#14552 = CARTESIAN_POINT ( 'NONE',  ( 16.56230152254411081, 6.928203230275506996, -9.899999998771034981 ) ) ;
#14553 = CARTESIAN_POINT ( 'NONE',  ( 0.000000000000000000, 141.0000000000000000, 7.500000000000000000 ) ) ;
#14554 = CARTESIAN_POINT ( 'NONE',  ( 27.48022219281702405, -5.407089921784859143, 159.8877424583000391 ) ) ;
#14555 = CARTESIAN_POINT ( 'NONE',  ( 21.00000000000000000, 6.928203230275506996, -2.306249998770960374 ) ) ;
#14556 = CARTESIAN_POINT ( 'NONE',  ( 10.31873187879410736, 0.000000000000000000, -8.296874999385501326 ) ) ;
#14557 = CARTESIAN_POINT ( 'NONE',  ( 7.234628195640309123, 197.2799038117966859, -27.00000000000000711 ) ) ;
#14558 = CIRCLE ( 'NONE', #35735, 28.99999999999999645 ) ;
#14559 = CARTESIAN_POINT ( 'NONE',  ( -7.954856959092191815, 68.77268628210143220, -5.529263428287477744 ) ) ;
#14560 = CYLINDRICAL_SURFACE ( 'NONE', #12832, 6.000000000000001776 ) ;
#14561 = CARTESIAN_POINT ( 'NONE',  ( 27.47391033735120303, 4.898587196589416773E-16, 169.8919867420001992 ) ) ;
#14562 = CARTESIAN_POINT ( 'NONE',  ( 10.49813415415989581, 91.77268628210144641, 7.228626920339068285 ) ) ;
#14563 = CARTESIAN_POINT ( 'NONE',  ( 22.56230152254345711, 3.464101615138142520, -5.137500000000025935 ) ) ;
#14564 = CARTESIAN_POINT ( 'NONE',  ( 7.234628195640322446, 198.4450961906613600, 26.99999999999999645 ) ) ;
#14565 = EDGE_LOOP ( 'NONE', ( #6491, #19954, #16359, #19403 ) ) ;
#14566 = CARTESIAN_POINT ( 'NONE',  ( 33.83730346391489263, 5.407089921784857367, 160.9125861580968149 ) ) ;
#14567 = CARTESIAN_POINT ( 'NONE',  ( 21.00000000000000000, -6.646953231504538984, -7.228124999385454608 ) ) ;
#14568 = CARTESIAN_POINT ( 'NONE',  ( 5.778771075727756162E-15, 195.9218750006145342, 31.45816453501076637 ) ) ;
#14569 = CARTESIAN_POINT ( 'NONE',  ( 34.48606902399273366, -5.407089921784861808, 168.3280104420172449 ) ) ;
#14570 = CARTESIAN_POINT ( 'NONE',  ( 34.15965927292618431, 5.196152422706637353, 165.9944540390638679 ) ) ;
#14571 = CARTESIAN_POINT ( 'NONE',  ( -13.49999999999998401, 198.2750000000000057, 23.38268590217985476 ) ) ;
#14572 = CARTESIAN_POINT ( 'NONE',  ( 21.00000000000000000, 249.2125000000000057, 6.928203230275506996 ) ) ;
#14573 = CARTESIAN_POINT ( 'NONE',  ( 27.24356964375000345, 199.5781250006145342, -3.336375036156643733E-15 ) ) ;
#14574 = CARTESIAN_POINT ( 'NONE',  ( 8.715434833792128799, 129.5398137178985678, -8.962234695871567070 ) ) ;
#14575 = CARTESIAN_POINT ( 'NONE',  ( -6.932735513423968321, 124.5476862821014521, -10.69584247140445221 ) ) ;
#14576 = PRESENTATION_LAYER_ASSIGNMENT (  '', '', ( #33920 ) ) ;
#14578 = ORIENTED_EDGE ( 'NONE', *, *, #30423, .F. ) ;
#14577 = ORIENTED_EDGE ( 'NONE', *, *, #15680, .F. ) ;
#14579 = CARTESIAN_POINT ( 'NONE',  ( 27.24356964374999635, 199.1656250006145399, -15.72908226750539029 ) ) ;
#14580 = CARTESIAN_POINT ( 'NONE',  ( 15.24356964374999990, 241.6468750006145285, 0.000000000000000000 ) ) ;
#14581 = CARTESIAN_POINT ( 'NONE',  ( -15.50000000000000533, 89.28981371789856780, 0.1745138560722471477 ) ) ;
#14582 = CARTESIAN_POINT ( 'NONE',  ( 18.12178482187499640, 4.985214923628404904, -3.028124999385484184 ) ) ;
#14583 = CARTESIAN_POINT ( 'NONE',  ( 15.24356964374999990, 247.5718750006145399, -3.323476615752268604 ) ) ;
#14584 = CARTESIAN_POINT ( 'NONE',  ( 13.50000000000001421, 197.5625000012290400, 23.38268590217984055 ) ) ;
#14585 = CARTESIAN_POINT ( 'NONE',  ( 5.529263428287300108, 67.72731371789853938, 7.954856959092309943 ) ) ;
#14586 = CARTESIAN_POINT ( 'NONE',  ( 13.44051670066911441, 5.407089921784856479, -2.915624999385552307 ) ) ;
#14587 =( BOUNDED_CURVE ( )  B_SPLINE_CURVE ( 2, ( #6878, #30887, #21487, #33027, #33729, #9533, #16491, #28039, #2071, #6499, #29615, #15220, #26769, #23941, #5843, #31077, #5651, #25940, #28961, #16865, #14569, #31442, #31623, #17234, #14199, #33913, #17421, #22924, #22548, #37303, #8147, #25750, #2441, #14015, #31806, #28226, #8693, #28402, #2255, #31259, #2999, #20079, #20267, #19530, #5465, #5100, #34287, #37117, #28772, #36930, #7955, #34097, #17047, #34469, #14382, #8512, #16679, #11353, #28585, #5285, #2623, #2812, #23105, #37483, #8331, #13834, #11534, #22738, #10977, #34649, #19901, #26121, #11718, #153, #25381, #19719, #25565, #11165, #17793, #32370, #27068, #6220, #15320, #24041, #35393, #29712, #3937, #35587, #12473, #23292, #12281, #9632, #20455, #29336, #29142, #32186, #902, #31997, #18359, #20639, #21209, #522, #3374, #34837, #18172, #9442, #11905, #6026, #21020, #32748, #9256, #32556, #3566, #6597, #3746, #14943, #6785, #35025, #29908, #26679, #20829, #9069, #6409, #26303, #23855, #26490, #26872, #15512, #17612, #23472, #12089, #1092, #23663, #8877, #35207, #3183, #14759, #17983, #340, #29527, #15129, #710, #10563, #24229, #4313, #22140, #16265, #24598, #32935, #4873, #4502, #30099, #33686, #19310, #18746, #1658, #16452, #27996, #10378, #24961, #13232, #4131, #27628, #24781, #13413, #19116, #6989, #36148, #35964, #7173, #27815, #1277, #1469, #16079, #21953, #13043, #36332, #30288, #1843, #30848, #33499, #18557, #36519, #10002, #15703, #7544, #30666, #27254, #12848, #30482, #4684, #24416, #21583, #10191, #33130, #15892, #7727, #27437, #21767, #12661, #35773, #7357, #9817, #33317, #21394, #18929, #22877, #20218, #2028, #2212, #37442, #14155, #13794, #25524, #31216, #36890, #34244, #25341, #11123, #16640, #22700, #8649, #8103, #8286, #13974, #5058, #33874, #19859, #28543, #37077, #22322, #10936, #22510, #31581, #2767, #25709, #8465, #31764, #14340, #28729, #13605, #25894, #36710, #34057, #7916, #19677, #17189, #10749, #34606, #5245, #11491, #31402, #5421, #5604, #28181, #37262, #20035, #17002, #11309, #23060, #34428, #5795, #2585, #17375, #25155, #16822, #19490, #28364, #31036 ),
 .UNSPECIFIED., .F., .F. ) 
 B_SPLINE_CURVE_WITH_KNOTS ( ( 3, 2, 2, 2, 2, 2, 2, 2, 2, 2, 2, 2, 2, 2, 2, 2, 2, 2, 2, 2, 2, 2, 2, 2, 2, 2, 2, 2, 2, 2, 2, 2, 2, 2, 2, 2, 2, 2, 2, 2, 2, 2, 2, 2, 2, 2, 2, 2, 2, 2, 2, 2, 2, 2, 2, 2, 2, 2, 2, 2, 2, 2, 2, 2, 2, 2, 2, 2, 2, 2, 2, 2, 2, 2, 2, 2, 2, 2, 2, 2, 2, 2, 2, 2, 2, 2, 2, 2, 2, 2, 2, 2, 2, 2, 2, 2, 2, 2, 2, 2, 2, 2, 2, 2, 2, 2, 2, 2, 2, 2, 2, 2, 2, 2, 2, 2, 2, 2, 2, 2, 2, 2, 2, 2, 2, 2, 2, 2, 2, 2, 2, 2, 2, 2, 3 ),
 ( 0.000000000000000000, 0.007246376811594202987, 0.01449275362318840597, 0.02173913043478260809, 0.02898550724637681195, 0.03623188405797101580, 0.04347826086956521618, 0.05072463768115942351, 0.05797101449275362389, 0.06521739130434782428, 0.07246376811594203160, 0.07971014492753622505, 0.08695652173913043237, 0.09420289855072463969, 0.1014492753623188470, 0.1086956521739130405, 0.1159420289855072478, 0.1231884057971014551, 0.1304347826086956486, 0.1376811594202898559, 0.1449275362318840632, 0.1521739130434782705, 0.1594202898550724501, 0.1666666666666666574, 0.1739130434782608647, 0.1811594202898550721, 0.1884057971014492794, 0.1956521739130434867, 0.2028985507246376940, 0.2101449275362318736, 0.2173913043478260809, 0.2246376811594202882, 0.2318840579710144956, 0.2391304347826087029, 0.2463768115942029102, 0.2536231884057971175, 0.2608695652173912971, 0.2681159420289855322, 0.2753623188405797118, 0.2826086956521738913, 0.2898550724637681264, 0.2971014492753623060, 0.3043478260869565410, 0.3115942028985507206, 0.3188405797101449002, 0.3260869565217391353, 0.3333333333333333148, 0.3405797101449275499, 0.3478260869565217295, 0.3550724637681159646, 0.3623188405797101441, 0.3695652173913043237, 0.3768115942028985588, 0.3840579710144927383, 0.3913043478260869734, 0.3985507246376811530, 0.4057971014492753881, 0.4130434782608695676, 0.4202898550724637472, 0.4275362318840579823, 0.4347826086956521618, 0.4420289855072463969, 0.4492753623188405765, 0.4565217391304347561, 0.4637681159420289911, 0.4710144927536231707, 0.4782608695652174058, 0.4855072463768115854, 0.4927536231884058204, 0.5000000000000000000, 0.5072463768115942351, 0.5144927536231883591, 0.5217391304347825942, 0.5289855072463768293, 0.5362318840579710644, 0.5434782608695651884, 0.5507246376811594235, 0.5579710144927536586, 0.5652173913043477826, 0.5724637681159420177, 0.5797101449275362528, 0.5869565217391304879, 0.5942028985507246119, 0.6014492753623188470, 0.6086956521739130821, 0.6159420289855072062, 0.6231884057971014412, 0.6304347826086956763, 0.6376811594202898004, 0.6449275362318840354, 0.6521739130434782705, 0.6594202898550725056, 0.6666666666666666297, 0.6739130434782608647, 0.6811594202898550998, 0.6884057971014492239, 0.6956521739130434590, 0.7028985507246376940, 0.7101449275362319291, 0.7173913043478260532, 0.7246376811594202882, 0.7318840579710145233, 0.7391304347826086474, 0.7463768115942028825, 0.7536231884057971175, 0.7608695652173913526, 0.7681159420289854767, 0.7753623188405797118, 0.7826086956521739468, 0.7898550724637680709, 0.7971014492753623060, 0.8043478260869565410, 0.8115942028985507761, 0.8188405797101449002, 0.8260869565217391353, 0.8333333333333333703, 0.8405797101449274944, 0.8478260869565217295, 0.8550724637681159646, 0.8623188405797101996, 0.8695652173913043237, 0.8768115942028985588, 0.8840579710144927938, 0.8913043478260869179, 0.8985507246376811530, 0.9057971014492753881, 0.9130434782608695121, 0.9202898550724637472, 0.9275362318840579823, 0.9347826086956522174, 0.9420289855072463414, 0.9492753623188405765, 0.9565217391304348116, 0.9637681159420289356, 0.9662082893573751274 ),
 .UNSPECIFIED. ) 
 CURVE ( )  GEOMETRIC_REPRESENTATION_ITEM ( )  RATIONAL_B_SPLINE_CURVE ( ( 1.000000000000000000, 0.8660254037844387076, 1.000000000000000000, 0.8660254037844387076, 1.000000000000000000, 0.8660254037844387076, 1.000000000000000000, 0.8660254037844387076, 1.000000000000000000, 0.8660254037844387076, 1.000000000000000000, 0.8660254037844387076, 1.000000000000000000, 0.8660254037844387076, 1.000000000000000000, 0.8660254037844387076, 1.000000000000000000, 0.8660254037844387076, 1.000000000000000000, 0.8660254037844387076, 1.000000000000000000, 0.8660254037844387076, 1.000000000000000000, 0.8660254037844387076, 1.000000000000000000, 0.8660254037844387076, 1.000000000000000000, 0.8660254037844387076, 1.000000000000000000, 0.8660254037844387076, 1.000000000000000000, 0.8660254037844387076, 1.000000000000000000, 0.8660254037844387076, 1.000000000000000000, 0.8660254037844387076, 1.000000000000000000, 0.8660254037844387076, 1.000000000000000000, 0.8660254037844387076, 1.000000000000000000, 0.8660254037844387076, 1.000000000000000000, 0.8660254037844387076, 1.000000000000000000, 0.8660254037844387076, 1.000000000000000000, 0.8660254037844387076, 1.000000000000000000, 0.8660254037844387076, 1.000000000000000000, 0.8660254037844387076, 1.000000000000000000, 0.8660254037844387076, 1.000000000000000000, 0.8660254037844387076, 1.000000000000000000, 0.8660254037844387076, 1.000000000000000000, 0.8660254037844387076, 1.000000000000000000, 0.8660254037844387076, 1.000000000000000000, 0.8660254037844387076, 1.000000000000000000, 0.8660254037844387076, 1.000000000000000000, 0.8660254037844387076, 1.000000000000000000, 0.8660254037844387076, 1.000000000000000000, 0.8660254037844387076, 1.000000000000000000, 0.8660254037844387076, 1.000000000000000000, 0.8660254037844387076, 1.000000000000000000, 0.8660254037844387076, 1.000000000000000000, 0.8660254037844387076, 1.000000000000000000, 0.8660254037844387076, 1.000000000000000000, 0.8660254037844387076, 1.000000000000000000, 0.8660254037844387076, 1.000000000000000000, 0.8660254037844387076, 1.000000000000000000, 0.8660254037844387076, 1.000000000000000000, 0.8660254037844387076, 1.000000000000000000, 0.8660254037844387076, 1.000000000000000000, 0.8660254037844387076, 1.000000000000000000, 0.8660254037844387076, 1.000000000000000000, 0.8660254037844387076, 1.000000000000000000, 0.8660254037844387076, 1.000000000000000000, 0.8660254037844387076, 1.000000000000000000, 0.8660254037844387076, 1.000000000000000000, 0.8660254037844387076, 1.000000000000000000, 0.8660254037844387076, 1.000000000000000000, 0.8660254037844387076, 1.000000000000000000, 0.8660254037844387076, 1.000000000000000000, 0.8660254037844387076, 1.000000000000000000, 0.8660254037844387076, 1.000000000000000000, 0.8660254037844387076, 1.000000000000000000, 0.8660254037844387076, 1.000000000000000000, 0.8660254037844387076, 1.000000000000000000, 0.8660254037844387076, 1.000000000000000000, 0.8660254037844387076, 1.000000000000000000, 0.8660254037844387076, 1.000000000000000000, 0.8660254037844387076, 1.000000000000000000, 0.8660254037844387076, 1.000000000000000000, 0.8660254037844387076, 1.000000000000000000, 0.8660254037844387076, 1.000000000000000000, 0.8660254037844387076, 1.000000000000000000, 0.8660254037844387076, 1.000000000000000000, 0.8660254037844387076, 1.000000000000000000, 0.8660254037844387076, 1.000000000000000000, 0.8660254037844387076, 1.000000000000000000, 0.8660254037844387076, 1.000000000000000000, 0.8660254037844387076, 1.000000000000000000, 0.8660254037844387076, 1.000000000000000000, 0.8660254037844387076, 1.000000000000000000, 0.8660254037844387076, 1.000000000000000000, 0.8660254037844387076, 1.000000000000000000, 0.8660254037844387076, 1.000000000000000000, 0.8660254037844387076, 1.000000000000000000, 0.8660254037844387076, 1.000000000000000000, 0.8660254037844387076, 1.000000000000000000, 0.8660254037844387076, 1.000000000000000000, 0.8660254037844387076, 1.000000000000000000, 0.8660254037844387076, 1.000000000000000000, 0.8660254037844387076, 1.000000000000000000, 0.8660254037844387076, 1.000000000000000000, 0.8660254037844387076, 1.000000000000000000, 0.8660254037844387076, 1.000000000000000000, 0.8660254037844387076, 1.000000000000000000, 0.8660254037844387076, 1.000000000000000000, 0.8660254037844387076, 1.000000000000000000, 0.8660254037844387076, 1.000000000000000000, 0.8660254037844387076, 1.000000000000000000, 0.8660254037844387076, 1.000000000000000000, 0.8660254037844387076, 1.000000000000000000, 0.8660254037844387076, 1.000000000000000000, 0.8660254037844387076, 1.000000000000000000, 0.8660254037844387076, 1.000000000000000000, 0.8660254037844387076, 1.000000000000000000, 0.8660254037844387076, 1.000000000000000000, 0.8660254037844387076, 1.000000000000000000, 0.8660254037844387076, 1.000000000000000000, 0.8660254037844387076, 1.000000000000000000, 0.8660254037844387076, 1.000000000000000000, 0.8660254037844387076, 1.000000000000000000, 0.8660254037844387076, 1.000000000000000000, 0.8660254037844387076, 1.000000000000000000, 0.8660254037844387076, 1.000000000000000000, 0.8660254037844387076, 1.000000000000000000, 0.8660254037844387076, 1.000000000000000000, 0.8660254037844387076, 1.000000000000000000, 0.8660254037844387076, 1.000000000000000000, 0.8660254037844387076, 1.000000000000000000, 0.8660254037844387076, 1.000000000000000000, 0.8660254037844387076, 1.000000000000000000, 0.8660254037844387076, 1.000000000000000000, 0.8660254037844387076, 1.000000000000000000, 0.8660254037844387076, 1.000000000000000000, 0.8660254037844387076, 1.000000000000000000, 0.8660254037844387076, 1.000000000000000000, 0.8660254037844387076, 1.000000000000000000, 0.8660254037844387076, 1.000000000000000000, 0.8660254037844387076, 1.000000000000000000, 0.8660254037844387076, 1.000000000000000000, 0.8660254037844387076, 1.000000000000000000, 0.8660254037844387076, 1.000000000000000000, 0.8660254037844387076, 1.000000000000000000, 0.8660254037844387076, 1.000000000000000000, 0.8660254037844387076, 1.000000000000000000, 0.8660254037844387076, 1.000000000000000000, 0.9548848677736607726, 0.9401542295229587953 ) ) 
 REPRESENTATION_ITEM ( '' )  );
#14588 = EDGE_CURVE ( 'NONE', #17802, #4869, #3956, .T. ) ;
#14589 = CARTESIAN_POINT ( 'NONE',  ( 15.24356964374999990, 242.9968750006145228, 0.000000000000000000 ) ) ;
#14590 = CARTESIAN_POINT ( 'NONE',  ( -4.944772684328424539, 45.01481371789854791, -11.48171059495408031 ) ) ;
#14591 = CARTESIAN_POINT ( 'NONE',  ( 16.56230152254410726, 0.000000000000000000, -10.00000000000000000 ) ) ;
#14592 = CARTESIAN_POINT ( 'NONE',  ( 7.228626920339068285, 107.8726862821014549, -10.49813415415989581 ) ) ;
#14593 = CARTESIAN_POINT ( 'NONE',  ( 10.56230152254411259, -3.464101615137757051, -4.799999998770999809 ) ) ;
#14594 = EDGE_CURVE ( 'NONE', #21071, #34895, #25976, .T. ) ;
#14595 = CARTESIAN_POINT ( 'NONE',  ( -32.38913769728823411, 206.8500491399821044, -5.686928522499717253 ) ) ;
#14596 = DIRECTION ( 'NONE',  ( 1.000000000000000000, 0.000000000000000000, 0.000000000000000000 ) ) ;
#14597 = VECTOR ( 'NONE', #10150, 1000.000000000000000 ) ;
#14598 = CARTESIAN_POINT ( 'NONE',  ( 33.96355885174396860, 5.196152422706637353, 163.7530159683574311 ) ) ;
#14599 = CARTESIAN_POINT ( 'NONE',  ( 11.08355503943142750, 98.96018628210144641, -10.83675517735155225 ) ) ;
#14600 = CARTESIAN_POINT ( 'NONE',  ( -7.228626920339070061, 20.47268628210143859, 10.49813415415989404 ) ) ;
#14601 = CYLINDRICAL_SURFACE ( 'NONE', #35176, 6.000000000000001776 ) ;
#14602 = LINE ( 'NONE', #6055, #35690 ) ;
#14603 = CARTESIAN_POINT ( 'NONE',  ( 6.594114490232313663, 128.8601862821014663, 6.840914352312096547 ) ) ;
#14604 =( BOUNDED_CURVE ( )  B_SPLINE_CURVE ( 2, ( #24705, #36257, #21871, #34167, #25820, #22803, #37367, #5530, #28656 ),
 .UNSPECIFIED., .F., .F. ) 
 B_SPLINE_CURVE_WITH_KNOTS ( ( 3, 2, 2, 2, 3 ),
 ( 0.5625000000000000000, 0.5694444444444444198, 0.5833333333333333703, 0.5972222222222222099, 0.6041666666666667407 ),
 .UNSPECIFIED. ) 
 CURVE ( )  GEOMETRIC_REPRESENTATION_ITEM ( )  RATIONAL_B_SPLINE_CURVE ( ( 0.9330127018922194093, 0.9330127018922194093, 1.000000000000000000, 0.8660254037844387076, 1.000000000000000000, 0.8660254037844387076, 1.000000000000000000, 0.9330127018922187432, 0.9330127018922192983 ) ) 
 REPRESENTATION_ITEM ( '' )  );
#14605 = CARTESIAN_POINT ( 'NONE',  ( 21.00000000000000000, 242.4343750006145228, -6.646953231504538984 ) ) ;
#14606 = ORIENTED_EDGE ( 'NONE', *, *, #20289, .F. ) ;
#14607 = CARTESIAN_POINT ( 'NONE',  ( -29.00000000000002487, 210.0000000000000000, 0.000000000000000000 ) ) ;
#14608 = CARTESIAN_POINT ( 'NONE',  ( 7.954856959092191815, 64.17268628210143788, 5.529263428287477744 ) ) ;
#14609 = CARTESIAN_POINT ( 'NONE',  ( 23.87821517812500005, -4.985214923628404016, -1.340624999385475746 ) ) ;
#14610 = CARTESIAN_POINT ( 'NONE',  ( 10.56230152254378929, 3.464101615137573198, -7.687500000000015987 ) ) ;
#14611 = CARTESIAN_POINT ( 'NONE',  ( 13.62178482187499640, 196.1093750006145342, -23.59362340125807123 ) ) ;
#14612 = DIRECTION ( 'NONE',  ( -0.000000000000000000, 1.000000000000000000, -0.000000000000000000 ) ) ;
#14613 = CYLINDRICAL_SURFACE ( 'NONE', #35102, 5.999999999999999112 ) ;
#14614 = CARTESIAN_POINT ( 'NONE',  ( -9.534712964251895073, 43.57731371789854080, -1.715153634034446428 ) ) ;
#14615 = CARTESIAN_POINT ( 'NONE',  ( 0.000000000000000000, 0.000000000000000000, -7.500000000000000000 ) ) ;
#14616 = EDGE_LOOP ( 'NONE', ( #22188, #5446, #5222, #37210 ) ) ;
#14617 = ORIENTED_EDGE ( 'NONE', *, *, #15854, .T. ) ;
#14618 = CARTESIAN_POINT ( 'NONE',  ( 21.00000000000000000, 248.2843750006145171, -6.646953231504538984 ) ) ;
#14620 = VECTOR ( 'NONE', #18123, 1000.000000000000000 ) ;
#14619 = CARTESIAN_POINT ( 'NONE',  ( -11.61527771782809282, 53.06481371789854506, -4.622313124798832717 ) ) ;
#14621 = CARTESIAN_POINT ( 'NONE',  ( 13.44051670066910908, 5.407089921784862696, -8.821874999385526550 ) ) ;
#14622 = CARTESIAN_POINT ( 'NONE',  ( 23.87821517812499650, 4.985214923628404904, -8.503124999385491378 ) ) ;
#14623 = CARTESIAN_POINT ( 'NONE',  ( -7.228626920338836470, 17.12731371789854862, -10.49813415416005213 ) ) ;
#14624 = EDGE_LOOP ( 'NONE', ( #24486, #6390, #8293, #3897 ) ) ;
#14625 = CARTESIAN_POINT ( 'NONE',  ( 22.80587116629412137, 7.646167579472024665E-16, -3.571874999385521221 ) ) ;
#14626 = CARTESIAN_POINT ( 'NONE',  ( -27.24356964374999990, 198.8656250006145569, -15.72908226750537786 ) ) ;
#14627 = CARTESIAN_POINT ( 'NONE',  ( 34.34226204845910502, 5.407089921784862696, 166.6842891901658845 ) ) ;
#14628 = APPLICATION_CONTEXT ( 'automotive_design' ) ;
#14629 = CARTESIAN_POINT ( 'NONE',  ( -61.67336230271184405, 217.4189793300686233, 4.149950860017807663 ) ) ;
#14630 = CARTESIAN_POINT ( 'NONE',  ( 15.24356964374999990, 249.2968750006145058, 0.000000000000000000 ) ) ;
#14631 = CARTESIAN_POINT ( 'NONE',  ( -24.86337347398900022, 195.0000000000000853, -10.63620294009199441 ) ) ;
#14632 = CARTESIAN_POINT ( 'NONE',  ( -57.51711230271184405, 214.4690446883608104, -1.321298161741814914 ) ) ;
#14633 = CARTESIAN_POINT ( 'NONE',  ( -33.77455436395490551, 205.1570982666397356, 4.673758765035198159 ) ) ;
#14634 = EDGE_LOOP ( 'NONE', ( #28158, #32281, #13921, #23905 ) ) ;
#14635 = CYLINDRICAL_SURFACE ( 'NONE', #23393, 5.999999999999998224 ) ;
#14636 = CARTESIAN_POINT ( 'NONE',  ( 19.56230152254412147, 5.196152422706637353, -1.500000000000029088 ) ) ;
#14637 = CARTESIAN_POINT ( 'NONE',  ( 14.25334919248795451, 28.91481371789854649, -6.092822981423661410 ) ) ;
#14638 = CARTESIAN_POINT ( 'NONE',  ( -66.03497103062157692, 202.6965474657331185, -4.350049139982091084 ) ) ;
#14640 = AXIS2_PLACEMENT_3D ( 'NONE', #5278, #19340, #2062 ) ;
#14639 =( BOUNDED_CURVE ( )  B_SPLINE_CURVE ( 2, ( #17638, #19930, #14786, #29170, #28985, #6250, #8538, #17828, #31468 ),
 .UNSPECIFIED., .F., .F. ) 
 B_SPLINE_CURVE_WITH_KNOTS ( ( 3, 2, 2, 2, 3 ),
 ( 0.8152173913043478937, 0.8188405797101449002, 0.8260869565217391353, 0.8333333333333333703, 0.8369565217391303769 ),
 .UNSPECIFIED. ) 
 CURVE ( )  GEOMETRIC_REPRESENTATION_ITEM ( )  RATIONAL_B_SPLINE_CURVE ( ( 0.9330127018922192983, 0.9330127018922202975, 1.000000000000000000, 0.8660254037844387076, 1.000000000000000000, 0.8660254037844387076, 1.000000000000000000, 0.9330127018922202975, 0.9330127018922192983 ) ) 
 REPRESENTATION_ITEM ( '' )  );
#14641 = CARTESIAN_POINT ( 'NONE',  ( 8.715434833791931624, 9.260186282101429356, 8.962234695871760692 ) ) ;
#14642 = CARTESIAN_POINT ( 'NONE',  ( 12.50000000000000355, 44.91018628210144215, 0.1745138560725507937 ) ) ;
#14643 = CARTESIAN_POINT ( 'NONE',  ( 10.56230152254410903, 0.000000000000000000, -4.500000000000031974 ) ) ;
#14644 = VERTEX_POINT ( 'NONE', #7816 ) ;
#14645 = CARTESIAN_POINT ( 'NONE',  ( -48.42038769728822700, 208.1428034533959703, 6.469044688360771289 ) ) ;
#14646 = DIRECTION ( 'NONE',  ( 0.000000000000000000, -0.000000000000000000, -1.000000000000000000 ) ) ;
#14647 = CARTESIAN_POINT ( 'NONE',  ( -1.926257025242585782E-15, 195.2468750006145513, -31.45816453501075927 ) ) ;
#14648 = CARTESIAN_POINT ( 'NONE',  ( 19.56230152254411081, -5.196152422706629359, -6.487499998771045995 ) ) ;
#14649 = CARTESIAN_POINT ( 'NONE',  ( 1.069080835302379631E-14, 195.2750000012290457, 27.00000000000000000 ) ) ;
#14650 = FACE_OUTER_BOUND ( 'NONE', #17647, .T. ) ;
#14651 = CARTESIAN_POINT ( 'NONE',  ( 18.00000000000000355, 240.2312500012290570, 5.196152422706632912 ) ) ;
#14652 = CARTESIAN_POINT ( 'NONE',  ( 15.24356964374999990, 246.2593750006145399, 0.000000000000000000 ) ) ;
#14653 = CARTESIAN_POINT ( 'NONE',  ( -9.500000000000005329, 89.28981371789856780, 0.1745138560723101806 ) ) ;
#14654 = DIRECTION ( 'NONE',  ( 0.000000000000000000, 0.000000000000000000, -1.000000000000000000 ) ) ;
#14655 = EDGE_LOOP ( 'NONE', ( #21402, #20315, #28222, #24098, #23575 ) ) ;
#14656 = CARTESIAN_POINT ( 'NONE',  ( -59.50372103062156981, 216.5309553116391612, -1.626142955000564383 ) ) ;
#14657 = PLANE ( 'NONE',  #17212 ) ;
#14658 = CARTESIAN_POINT ( 'NONE',  ( 26.99999999999999645, 245.7437500012290457, 3.464101615137751278 ) ) ;
#14659 = CARTESIAN_POINT ( 'NONE',  ( 12.50000000000000355, 103.0898137178985650, -0.1745138560722771515 ) ) ;
#14660 = CARTESIAN_POINT ( 'NONE',  ( 22.80587116629411426, -3.604726614523238837, -1.809374999385491511 ) ) ;
#14661 = CARTESIAN_POINT ( 'NONE',  ( 27.00000000000001421, 198.0500000012290513, 15.58845726811988897 ) ) ;
#14662 = CARTESIAN_POINT ( 'NONE',  ( 18.12178482187500350, -4.985214923628407568, -1.978124999385488803 ) ) ;
#14663 = CARTESIAN_POINT ( 'NONE',  ( -0.1745138560722763466, 73.18981371789855928, -12.50000000000000355 ) ) ;
#14664 = CARTESIAN_POINT ( 'NONE',  ( 27.24356964374999635, 197.4218750006145342, -15.72908226750539029 ) ) ;
#14665 = ADVANCED_FACE ( 'NONE', ( #27715 ), #30936, .T. ) ;
#14666 = ORIENTED_EDGE ( 'NONE', *, *, #12852, .F. ) ;
#14667 = ORIENTED_EDGE ( 'NONE', *, *, #27143, .T. ) ;
#14668 = ORIENTED_EDGE ( 'NONE', *, *, #21240, .T. ) ;
#14669 = CARTESIAN_POINT ( 'NONE',  ( 26.75643035624999655, 3.323476615752271268, -4.378124999385460292 ) ) ;
#14670 = CARTESIAN_POINT ( 'NONE',  ( -7.234628195640302017, 195.5924038105676743, 27.00000000000000711 ) ) ;
#14671 = CARTESIAN_POINT ( 'NONE',  ( 21.00000000000000000, 247.1593750006145171, 6.646953231504538984 ) ) ;
#14672 = CARTESIAN_POINT ( 'NONE',  ( 12.46528703574805874, 35.99768628210144072, 2.660918448318279950 ) ) ;
#14673 = CARTESIAN_POINT ( 'NONE',  ( -55.34002896937850124, 204.4285982733020433, 3.350049139982171020 ) ) ;
#14674 = DIRECTION ( 'NONE',  ( 0.9961946980917462113, 0.000000000000000000, -0.08715574274765118534 ) ) ;
#14675 = CARTESIAN_POINT ( 'NONE',  ( -32.57961230271184405, 211.3212981617417938, 4.469044688360757966 ) ) ;
#14676 = CARTESIAN_POINT ( 'NONE',  ( 36.79853094953357129, 7.347880794884117764E-16, 161.7357555859521199 ) ) ;
#14677 = CARTESIAN_POINT ( 'NONE',  ( 8.715434833792128799, 111.1398137178985621, -8.962234695871567070 ) ) ;
#14678 = CARTESIAN_POINT ( 'NONE',  ( -60.49330436395489130, 210.1155267958017703, -4.499999999999996447 ) ) ;
#14679 = CARTESIAN_POINT ( 'NONE',  ( -38.72247103062156981, 205.6499508600178956, 7.303452534266880569 ) ) ;
#14680 = EDGE_CURVE ( 'NONE', #26075, #37491, #19393, .T. ) ;
#14681 = CARTESIAN_POINT ( 'NONE',  ( 26.75643035624999655, 3.323476615752271268, -4.940624999385510918 ) ) ;
#14682 = CARTESIAN_POINT ( 'NONE',  ( 2.999999999999997335, 244.5000000000000000, 0.000000000000000000 ) ) ;
#14683 = CARTESIAN_POINT ( 'NONE',  ( 10.83675517735179206, 83.53981371789856780, -11.08355503943118769 ) ) ;
#14684 = CARTESIAN_POINT ( 'NONE',  ( -57.51711230271184405, 218.4690446883607535, -2.393094931466363651 ) ) ;
#14685 = ORIENTED_EDGE ( 'NONE', *, *, #7983, .T. ) ;
#14686 = CARTESIAN_POINT ( 'NONE',  ( 22.60769515458672885, 240.6825961894323314, 5.999999999999997335 ) ) ;
#14687 = CARTESIAN_POINT ( 'NONE',  ( 12.53471296425194836, 109.0226862821014606, -2.311890736173178418 ) ) ;
#14688 = CARTESIAN_POINT ( 'NONE',  ( 14.38691631536207538, 53.53518628210145636, -5.770363421893813793 ) ) ;
#14689 = ADVANCED_FACE ( 'NONE', ( #4953, #1556 ), #33219, .F. ) ;
#14690 = CARTESIAN_POINT ( 'NONE',  ( 20.99999999999999645, 0.000000000000000000, -8.000000000000000000 ) ) ;
#14691 = CARTESIAN_POINT ( 'NONE',  ( 27.73678691053042300, 5.407089921784862696, 162.8202906008076241 ) ) ;
#14692 = CARTESIAN_POINT ( 'NONE',  ( -14.38691631536207183, 67.33518628210143220, 5.770363421893814682 ) ) ;
#14693 = CARTESIAN_POINT ( 'NONE',  ( -1.926257025242585782E-15, 198.7906250006145399, -31.45816453501076637 ) ) ;
#14694 = CARTESIAN_POINT ( 'NONE',  ( 13.44051670066911619, -5.407089921784859143, -9.065624999385569538 ) ) ;
#14695 = CARTESIAN_POINT ( 'NONE',  ( 10.56230152254410903, 7.347880794884117764E-16, -10.00000000000000000 ) ) ;
#14696 = CARTESIAN_POINT ( 'NONE',  ( -45.45163769728822700, 215.6869285224996986, -3.149950860017881382 ) ) ;
#14697 = AXIS2_PLACEMENT_3D ( 'NONE', #9992, #6775, #12653 ) ;
#14698 = CARTESIAN_POINT ( 'NONE',  ( 12.38894624757142360, 4.437320182635244414, -9.999999999999994671 ) ) ;
#14699 = CARTESIAN_POINT ( 'NONE',  ( 6.932735513423970097, 46.34768628210145636, 10.69584247140445044 ) ) ;
#14700 = CARTESIAN_POINT ( 'NONE',  ( -27.24356964374999990, 199.8218750006145399, -15.72908226750537786 ) ) ;
#14701 = CARTESIAN_POINT ( 'NONE',  ( 24.98146486726017912, 0.000000000000000000, 164.3506311484184437 ) ) ;
#14702 = CARTESIAN_POINT ( 'NONE',  ( -1.715153634034234598, 14.72268628210143859, -9.534712964251941258 ) ) ;
#14703 = CARTESIAN_POINT ( 'NONE',  ( 23.87821517812499650, 246.1093750006145342, -4.985214923628404904 ) ) ;
#14704 = ORIENTED_EDGE ( 'NONE', *, *, #15765, .F. ) ;
#14705 = CARTESIAN_POINT ( 'NONE',  ( 15.00000000000000000, 0.000000000000000000, -5.849999999999994316 ) ) ;
#14707 = CARTESIAN_POINT ( 'NONE',  ( 21.00000000000000355, 0.000000000000000000, 50.00000000000001421 ) ) ;
#14706 = PRODUCT_DEFINITION_SHAPE ( 'NONE', 'NONE',  #37505 ) ;
#14708 = CARTESIAN_POINT ( 'NONE',  ( 27.92429219659289785, 5.196152422706630247, 163.5661617036773237 ) ) ;
#14709 = CARTESIAN_POINT ( 'NONE',  ( 10.31873187879411091, -3.604726614523240613, -3.703124999385514649 ) ) ;
#14710 = CARTESIAN_POINT ( 'NONE',  ( 28.17311034766084887, 5.407089921784856479, 167.8074903081294167 ) ) ;
#14711 = CARTESIAN_POINT ( 'NONE',  ( 18.00000000000000000, 240.9250000000000114, -5.196152422706630247 ) ) ;
#14712 = CARTESIAN_POINT ( 'NONE',  ( -71.54107125509844423, 209.3291073423510795, 5.000000000000000000 ) ) ;
#14713 =( BOUNDED_CURVE ( )  B_SPLINE_CURVE ( 2, ( #26388, #11801, #19978, #31520, #6107, #3270, #5921 ),
 .UNSPECIFIED., .F., .F. ) 
 B_SPLINE_CURVE_WITH_KNOTS ( ( 3, 2, 2, 3 ),
 ( 0.3478260869565210078, 0.3550724637681153539, 0.3623188405797096445, 0.3695652173913039351 ),
 .UNSPECIFIED. ) 
 CURVE ( )  GEOMETRIC_REPRESENTATION_ITEM ( )  RATIONAL_B_SPLINE_CURVE ( ( 1.000000000000013323, 0.8660254037844252739, 1.000000000000000000, 0.8660254037844387076, 1.000000000000000000, 0.8660254037844459241, 0.9999999999999927836 ) ) 
 REPRESENTATION_ITEM ( '' )  );
#14714 = CARTESIAN_POINT ( 'NONE',  ( -4.944772684328673229, 75.38518628210144357, 11.48171059495397728 ) ) ;
#14715 = ORIENTED_EDGE ( 'NONE', *, *, #14047, .T. ) ;
#14716 = ORIENTED_EDGE ( 'NONE', *, *, #24095, .F. ) ;
#14717 = DIRECTION ( 'NONE',  ( 1.000000000000000000, 0.000000000000000000, -0.000000000000000000 ) ) ;
#14718 = FACE_OUTER_BOUND ( 'NONE', #21541, .T. ) ;
#14720 = CARTESIAN_POINT ( 'NONE',  ( 22.56230152254410370, 7.347880794884117764E-16, -4.612499998771030008 ) ) ;
#14719 = COLOUR_RGB ( '',0.8941176470588234615, 0.8941176470588234615, 0.8941176470588234615 ) ;
#14721 = CARTESIAN_POINT ( 'NONE',  ( 23.87821517812500005, -4.985214923628404016, -5.840624999385479299 ) ) ;
#14722 = CARTESIAN_POINT ( 'NONE',  ( -15.53471296425188442, 43.57731371789854080, -2.908627838312459080 ) ) ;
#14723 = AXIS2_PLACEMENT_3D ( 'NONE', #32354, #3919, #6203 ) ;
#14724 = CARTESIAN_POINT ( 'NONE',  ( 34.02892565880470954, -5.196152422706635576, 164.5001619919262055 ) ) ;
#14725 = CARTESIAN_POINT ( 'NONE',  ( 20.00041297495057080, 239.8598985277379256, -5.668978411116884608 ) ) ;
#14726 = CARTESIAN_POINT ( 'NONE',  ( -63.25669563604515844, 209.8844732041982297, -4.499999999999996447 ) ) ;
#14727 = LINE ( 'NONE', #26276, #8302 ) ;
#14728 = CARTESIAN_POINT ( 'NONE',  ( 34.36556471527461554, 5.196152422706631135, 168.3479640145299641 ) ) ;
#14729 = CARTESIAN_POINT ( 'NONE',  ( 8.152565276336593669, 21.15231371789855430, 5.233372021372610483 ) ) ;
#14730 = ADVANCED_FACE ( 'NONE', ( #7443 ), #7258, .T. ) ;
#14731 = CARTESIAN_POINT ( 'NONE',  ( -53.36830436395489841, 209.8844732041982581, 6.500000000000000888 ) ) ;
#14732 = CARTESIAN_POINT ( 'NONE',  ( -42.67336230271183695, 217.4189793300686233, 4.149950860017807663 ) ) ;
#14733 =( NAMED_UNIT ( * ) SI_UNIT ( $, .STERADIAN. ) SOLID_ANGLE_UNIT ( ) );
#14734 = DIRECTION ( 'NONE',  ( 0.000000000000000000, 0.000000000000000000, 1.000000000000000000 ) ) ;
#14735 = CARTESIAN_POINT ( 'NONE',  ( 27.24356964375000700, 196.8968750006145285, 15.72908226750537075 ) ) ;
#14736 = CARTESIAN_POINT ( 'NONE',  ( 15.46528703574811736, 130.4023137178985792, -3.257655550456947768 ) ) ;
#14737 = EDGE_CURVE ( 'NONE', #15380, #22146, #5162, .T. ) ;
#14738 = ORIENTED_EDGE ( 'NONE', *, *, #26044, .F. ) ;
#14739 = CARTESIAN_POINT ( 'NONE',  ( -7.228626920339069173, 48.07268628210143646, 10.49813415415989581 ) ) ;
#14740 = CARTESIAN_POINT ( 'NONE',  ( 15.00000000000000000, 244.6562500012290400, 0.000000000000000000 ) ) ;
#14741 = CARTESIAN_POINT ( 'NONE',  ( 21.64885123950055501, 5.731983593561799317, -8.000000000000000000 ) ) ;
#14742 = CARTESIAN_POINT ( 'NONE',  ( 31.35328515338631306, 7.209453229046482114, 168.3385908086170559 ) ) ;
#14743 = CARTESIAN_POINT ( 'NONE',  ( 21.00000000000000000, 6.928203230275506996, -1.856249998770964860 ) ) ;
#14744 = STYLED_ITEM ( 'NONE', ( #24481 ), #10611 ) ;
#14745 = CARTESIAN_POINT ( 'NONE',  ( 13.44051670066911264, -5.407089921784865361, -7.771874999385531169 ) ) ;
#14746 = CARTESIAN_POINT ( 'NONE',  ( 20.99999999999999645, 250.0000000000000000, 0.000000000000000000 ) ) ;
#14747 = CARTESIAN_POINT ( 'NONE',  ( -1.715153634034234598, 60.72268628210144925, -9.534712964251941258 ) ) ;
#14748 = CARTESIAN_POINT ( 'NONE',  ( 15.00000000000000000, 249.5499999999999829, 0.000000000000000000 ) ) ;
#14749 = CARTESIAN_POINT ( 'NONE',  ( 1.120210788295102201E-13, 196.7375000000000398, -27.00000000000000711 ) ) ;
#14750 = AXIS2_PLACEMENT_3D ( 'NONE', #13036, #12656, #27429 ) ;
#14751 = EDGE_CURVE ( 'NONE', #31857, #10703, #16808, .T. ) ;
#14752 = CARTESIAN_POINT ( 'NONE',  ( 6.932735513423970097, 101.5476862821014379, 10.69584247140445044 ) ) ;
#14753 = CARTESIAN_POINT ( 'NONE',  ( 25.02068495149662297, 0.000000000000000000, 164.7989187625597367 ) ) ;
#14754 = CARTESIAN_POINT ( 'NONE',  ( 9.184850993605147944E-16, 150.0000000000000000, -7.500000000000000000 ) ) ;
#14755 = ORIENTED_EDGE ( 'NONE', *, *, #25649, .F. ) ;
#14756 = CARTESIAN_POINT ( 'NONE',  ( 30.65222614765987785, 7.209453229046475009, 160.3254497058415495 ) ) ;
#14757 = CARTESIAN_POINT ( 'NONE',  ( 26.75643035624999655, 7.049594010296217766E-16, -7.115624999385477878 ) ) ;
#14758 = CARTESIAN_POINT ( 'NONE',  ( 27.00000000000000355, 196.1750000000000114, -3.306546357697854128E-15 ) ) ;
#14759 = CARTESIAN_POINT ( 'NONE',  ( 34.10694154304044901, 5.407089921784862696, 163.9945635053181547 ) ) ;
#14760 = CARTESIAN_POINT ( 'NONE',  ( 28.04522078954815356, -5.196152422706638241, 164.9483818460552413 ) ) ;
#14761 = CARTESIAN_POINT ( 'NONE',  ( 21.00000000000000000, 248.7624999999999886, 6.928203230275506996 ) ) ;
#14762 = CARTESIAN_POINT ( 'NONE',  ( -27.24356964375000345, 197.5156250006145342, -15.72908226750537786 ) ) ;
#14763 = CARTESIAN_POINT ( 'NONE',  ( 11.48171059495408208, 130.1148137178985564, -4.944772684328420986 ) ) ;
#14764 = AXIS2_PLACEMENT_3D ( 'NONE', #30786, #13731, #16389 ) ;
#14765 = CARTESIAN_POINT ( 'NONE',  ( -8.962234695871760692, 131.1601862821014777, 8.715434833791933400 ) ) ;
#14767 = ORIENTED_EDGE ( 'NONE', *, *, #31372, .F. ) ;
#14766 = ORIENTED_EDGE ( 'NONE', *, *, #14505, .F. ) ;
#14768 = CARTESIAN_POINT ( 'NONE',  ( -1.926257025242585782E-15, 198.7906250006145399, -31.45816453501075927 ) ) ;
#14769 = CARTESIAN_POINT ( 'NONE',  ( 15.24356964374999990, 242.5468750006145058, 0.000000000000000000 ) ) ;
#14770 = EDGE_CURVE ( 'NONE', #22884, #16873, #20605, .T. ) ;
#14771 = CARTESIAN_POINT ( 'NONE',  ( 15.53471296425188797, 94.17731371789857064, 2.908627838312457747 ) ) ;
#14772 = CARTESIAN_POINT ( 'NONE',  ( 26.75643035624999655, 3.323476615752271712, -5.390624999385475569 ) ) ;
#14773 = CARTESIAN_POINT ( 'NONE',  ( 26.75643035624999655, 248.2468750006145797, 3.323476615752267715 ) ) ;
#14774 = PRESENTATION_LAYER_ASSIGNMENT (  '', '', ( #35945 ) ) ;
#14775 = EDGE_CURVE ( 'NONE', #17027, #10943, #3074, .T. ) ;
#14776 = CARTESIAN_POINT ( 'NONE',  ( -1.909035429704832693E-15, 195.9500000012290002, -31.17691453623979214 ) ) ;
#14777 = CARTESIAN_POINT ( 'NONE',  ( 3.796722387233182339, 77.21481371789855075, 8.710071997420207879 ) ) ;
#14778 = CARTESIAN_POINT ( 'NONE',  ( 22.80587116629411071, -3.604726614523235284, -5.803124999385537386 ) ) ;
#14779 = AXIS2_PLACEMENT_3D ( 'NONE', #13732, #33816, #19613 ) ;
#14780 = CARTESIAN_POINT ( 'NONE',  ( 18.12178482187500350, 242.1718750006145058, 4.985214923628407568 ) ) ;
#14781 = CARTESIAN_POINT ( 'NONE',  ( -4.622313124798826500, 41.56481371789855217, 11.61527771782809637 ) ) ;
#14782 = CYLINDRICAL_SURFACE ( 'NONE', #15195, 2.649999999999991029 ) ;
#14783 = CARTESIAN_POINT ( 'NONE',  ( 8.715434833791931624, 92.06018628210145494, 8.962234695871760692 ) ) ;
#14784 = CARTESIAN_POINT ( 'NONE',  ( 22.56230152254410370, 3.464101615137755275, -3.674999998771026011 ) ) ;
#14785 = CARTESIAN_POINT ( 'NONE',  ( -69.99330436395489130, 210.1155267958017703, -4.499999999999996447 ) ) ;
#14786 = CARTESIAN_POINT ( 'NONE',  ( 18.00000000000000355, 241.1312500012290343, 5.196152422706632912 ) ) ;
#14787 = CARTESIAN_POINT ( 'NONE',  ( 8.927990412390657937, 107.8726862821014549, -13.04141134922759804 ) ) ;
#14788 = CARTESIAN_POINT ( 'NONE',  ( 22.56230152254410726, 7.347880794884117764E-16, -3.262499998771012599 ) ) ;
#14789 = CARTESIAN_POINT ( 'NONE',  ( 1.120210788295102201E-13, 196.8500000012290343, -27.00000000000000711 ) ) ;
#14790 = CARTESIAN_POINT ( 'NONE',  ( -2.064181346179269738, 111.8976862821014606, 9.465287035748067623 ) ) ;
#14791 = DIRECTION ( 'NONE',  ( 1.000000000000000000, 0.000000000000000000, 0.000000000000000000 ) ) ;
#14792 = CARTESIAN_POINT ( 'NONE',  ( -2.908627838312119351, 14.72268628210143859, -15.53471296425195369 ) ) ;
#14793 = DIRECTION ( 'NONE',  ( 1.000000000000000000, 0.000000000000000000, 0.000000000000000000 ) ) ;
#14794 = CARTESIAN_POINT ( 'NONE',  ( 21.00000000000000000, 241.5343750006145171, -6.646953231504538984 ) ) ;
#14795 = ORIENTED_EDGE ( 'NONE', *, *, #24850, .F. ) ;
#14796 = CARTESIAN_POINT ( 'NONE',  ( 0.000000000000000000, 200.0000000000000000, 0.000000000000000000 ) ) ;
#14797 = VECTOR ( 'NONE', #24720, 1000.000000000000114 ) ;
#14798 = CARTESIAN_POINT ( 'NONE',  ( -9.500000000000005329, 67.91018628210144925, -0.1745138560725176813 ) ) ;
#14799 = CARTESIAN_POINT ( 'NONE',  ( 21.00000000000000000, -6.646953231504538984, -0.9281249993854503444 ) ) ;
#14801 = EDGE_CURVE ( 'NONE', #8245, #36001, #33518, .T. ) ;
#14800 = CARTESIAN_POINT ( 'NONE',  ( 23.99999999999999645, 241.7500000000000000, -5.196152422706631135 ) ) ;
#14802 = CARTESIAN_POINT ( 'NONE',  ( 26.99999999999991118, -3.464101615137797463, -4.706249998770959841 ) ) ;
#14803 = CARTESIAN_POINT ( 'NONE',  ( 25.24620043574905282, 0.000000000000000000, 167.3765725426477502 ) ) ;
#14804 = ADVANCED_FACE ( 'NONE', ( #36235 ), #16166, .F. ) ;
#14805 = CARTESIAN_POINT ( 'NONE',  ( 4.178139385881633139, 195.0000000000000568, 26.92487590381980667 ) ) ;
#14806 = CARTESIAN_POINT ( 'NONE',  ( -8.710071997420207879, 42.71481371789855075, 3.796722387233182339 ) ) ;
#14807 = FACE_OUTER_BOUND ( 'NONE', #19683, .T. ) ;
#14808 = VERTEX_POINT ( 'NONE', #14061 ) ;
#14809 = CARTESIAN_POINT ( 'NONE',  ( 23.87821517812499650, 249.1468750006145285, -4.985214923628404904 ) ) ;
#14810 = CARTESIAN_POINT ( 'NONE',  ( -8.715434833792127023, 51.33981371789855785, 8.962234695871568846 ) ) ;
#14811 = CARTESIAN_POINT ( 'NONE',  ( 26.75643035624999655, 3.323476615752271712, -9.890624999385464022 ) ) ;
#14812 = CARTESIAN_POINT ( 'NONE',  ( -2.660918448318004614, 17.70231371789854435, -12.46528703574811558 ) ) ;
#14813 =( BOUNDED_SURFACE ( )  B_SPLINE_SURFACE ( 3, 2, ( 
 ( #11254, #13922, #34189, #13739, #8234, #21582, #19434, #16764, #25287, #31167, #34374, #13042, #31344, #36838, #22454, #5190, #10881, #24597, #5371, #16950, #28312, #28493, #2536, #8416, #2350, #30287, #35963, #14102, #16583, #8045, #25654, #19621, #19985, #31528, #5553, #36655, #17138, #10001, #10692, #14288, #7172, #18745, #4312, #22270, #15891, #33823, #27436, #5929, #6314, #29431, #11619, #26207, #34927, #14656, #31899, #20166, #23194, #32271, #430, #14470, #2898, #20543, #26024, #23378, #3276, #17886, #28863, #8972, #34742, #17508, #29043, #20357, #53, #8595, #3465, #11808, #8785, #32086, #6117, #9160, #26397, #34556, #3088, #244, #17696, #29236, #23006, #14849, #37388, #11996, #23567, #35112, #20727, #31714, #15036, #26584, #5741, #17321, #613, #25839, #11439, #31466, #30919, #14042, #22949, #11188, #22763, #31650, #22578, #2468, #34123, #36960, #11005, #5313, #36775, #20102, #33760, #22393, #16707, #5489, #16891, #8173, #25226, #14178, #19556, #28254, #19748, #5677, #28799, #5126, #28429, #25591, #31286, #37147, #28066, #2284, #8535, #14225, #33941, #7984, #34311, #31107, #8356, #17072, #17258, #10820, #19928, #13860, #25408, #28611, #2648, #25776, #16518, #2835, #37326, #11376, #34494, #14407, #25963, #22210, #4936, #7800, #19376, #2100, #13679, #20292, #11746, #34675, #9283, #365, #35233, #17635, #31833, #20480, #9095, #28983, #5866, #23687, #11559, #26900, #20857, #17444, #3401, #12307, #548, #12114, #21045, #6436, #32396, #14969, #14595, #29361, #180 ),
 ( #14785, #23133, #29739, #23315, #29553, #26517, #18009, #26705, #3772, #736, #26329, #15346, #32210, #6248, #6623, #11929, #3024, #32583, #26147, #6049, #23881, #34863, #23499, #8903, #15156, #8720, #3592, #35420, #32018, #29168, #9470, #3212, #35047, #18199, #20664, #17826, #15906, #22336, #33331, #24974, #1482, #24796, #7740, #30302, #10577, #4886, #16653, #36724, #13426, #36534, #13246, #22156, #21596, #7371, #16280, #36347, #30680, #33888, #13057, #19324, #10391, #21967, #4700, #33514, #24612, #33702, #16466, #27827, #30861, #28010, #10765, #1857, #7557, #2043, #7931, #27455, #19133, #13621, #25172, #19505, #31051, #5073, #36161, #28198, #10016, #10207, #30496, #2227, #13808, #35979, #21781, #33146, #18943, #4518, #7190, #18759, #4327, #16092, #27644, #1672, #22894, #2598, #31231, #19873, #11689, #17393, #37090, #25538, #25911, #11138, #17204, #8665, #34806, #13987, #2783, #31416, #28557, #25724, #14170, #22715, #19691, #23262, #5620, #5435, #14356, #37456, #26094, #31777, #8120, #37277, #34258, #17018, #8301, #34070, #11323, #10950, #23075, #34441, #11506, #8481, #5259, #20051, #31597, #16838, #28377, #34620, #25356, #3156, #20234, #2414, #28743, #124, #5812, #28934, #8851, #2969, #14539, #20424, #31969, #5999, #17579, #36902, #29112, #22524, #20989, #35362, #3534, #17762, #30062, #12060, #20796, #15099, #24195, #21363, #35177, #9413, #18141, #12250, #29495, #20610, #9223, #1056, #6754, #26460, #14911, #15288, #494, #6567, #35556, #35740, #3342, #29683, #32339 ),
 ( #32523, #6377, #3717, #26841, #15478, #21175, #34995, #26649, #23634, #17952, #680, #23441, #23820, #307, #12442, #871, #24012, #9601, #9038, #32714, #18328, #32150, #6190, #29873, #14726, #26274, #3906, #29303, #27033, #12630, #9786, #32902, #6955, #18523, #11873, #33466, #7140, #21916, #30253, #19456, #4650, #13567, #10345, #27963, #1434, #30634, #18714, #30448, #13378, #35928, #16231, #10529, #22289, #4838, #19082, #27783, #18896, #1809, #27219, #13010, #7508, #4467, #36297, #1994, #4280, #24932, #16046, #27594, #36485, #1624, #15856, #22105, #33654, #7693, #19274, #30815, #16416, #25121, #13195, #36677, #10715, #21549, #24748, #33843, #7881, #4097, #15668, #1244, #27402, #12814, #24383, #24565, #36118, #9970, #33284, #10158, #33097, #21733, #7322, #11639, #8435, #31186, #25679, #31549, #19644, #34576, #13759, #22475, #5573, #16604, #34210, #37230, #10901, #20186, #14309, #31004, #14490, #8805, #26047, #11278, #36857, #22847, #25305, #8254, #5209, #34023, #34396, #8067, #20004, #28512, #17158, #19828, #5024, #23214, #16786, #11460, #28700, #2737, #8617, #34763, #31736, #31366, #28147, #14123, #25861, #74, #5390, #28331, #2921, #2368, #25490, #5763, #13941, #16970, #37042, #17343, #2178, #37410, #23028, #11090, #22666, #28886, #2555, #20560, #35312, #32103, #11826, #15053, #12199, #35691, #23773, #35506, #31920, #29636, #6135, #3857, #29063, #17713, #20378, #14675, #5950, #32290, #17903, #26225, #3672, #262, #20746, #6332, #15242, #17529, #3107, #29448, #3483 ),
 ( #9367, #14866, #23585, #12013, #23397, #24148, #21128, #34945, #26982, #823, #8990, #29252, #20941, #3294, #26601, #632, #26412, #447, #32474, #35127, #6521, #9177, #18096, #26792, #1008, #12392, #23963, #9553, #32666, #6707, #18279, #29823, #15433, #12581, #32851, #12958, #15998, #27170, #36434, #30588, #9743, #30767, #25068, #4790, #4417, #15616, #27546, #4044, #24518, #9920, #12768, #1572, #1194, #24698, #7274, #36250, #36068, #21314, #27913, #35878, #27732, #13144, #10294, #24886, #1942, #10476, #10111, #13513, #30393, #21866, #16366, #21682, #24337, #19223, #21504, #4230, #22053, #33047, #33234, #7095, #13328, #6898, #4603, #33418, #18663, #18473, #7457, #27356, #30203, #19033, #15806, #1387, #16182, #1762, #30014, #33608, #7646, #18848, #8389, #10851, #20136, #7831, #22424, #36625, #30954, #22244, #11038, #34159, #4972, #19958, #16553, #36994, #22612, #31500, #14441, #10664, #8204, #19781, #33792, #25441, #28283, #19406, #28097, #36809, #25625, #31138, #2322, #13893, #2130, #2869, #37358, #13708, #5712, #17107, #25260, #33974, #2500, #8014, #31317, #5345, #5157, #19590, #16923, #16736, #22794, #28464, #14074, #37181, #11224, #5523, #34345, #28649, #2685, #14261, #25811, #11412, #22980, #34530, #8569, #31683, #17293, #28833, #20699, #26366, #32243, #23918, #5901, #400, #6283, #11966, #3247, #14821, #9134, #3059, #35460, #26, #26179, #20517, #35265, #17859, #23538, #29014, #3809, #23349, #32057, #35082, #9510, #32623, #8942, #29402, #3434, #15003, #26554 ),
 ( #6086, #29206, #17670, #23167, #29779, #26743, #17482, #6661, #6476, #34709, #216, #583, #20328, #12151, #23728, #9321, #8755, #20890, #31869, #32433, #18048, #29590, #3626, #34899, #15196, #777, #12344, #18235, #21085, #11781, #25997, #11591, #14629, #18991, #35651, #6851, #15954, #965, #18620, #21640, #32810, #4564, #36208, #15387, #36395, #30728, #10441, #10068, #21273, #33192, #9696, #30162, #15573, #18427, #7235, #29970, #30353, #12916, #4376, #4191, #26935, #33568, #4000, #33382, #18809, #27507, #30547, #7604, #16140, #15766, #19181, #36025, #1529, #22015, #27317, #27129, #24844, #1155, #9880, #27690, #12541, #13103, #1344, #24658, #21460, #12727, #24295, #24479, #35838, #33001, #10252, #24106, #21828, #1719, #7421, #7052, #13288, #20615, #312, #36952, #10624, #10998, #36584, #7977, #4930, #7791, #22571, #22203, #19741, #2277, #31279, #19550, #16325, #23447, #30911, #22756, #8167, #5308, #20430, #35000, #31974, #31099, #9043, #25402, #34117, #11879, #5120, #33752, #14732, #19369, #36770, #6004, #16512, #16699, #28059, #8856, #4752, #37140, #16885, #2094, #1904, #28421, #22385, #13670, #2462, #25220, #10814, #14035, #25585, #27873, #11183, #17585, #13474, #34812, #33935, #26280, #25026, #28248, #13854, #29117, #3161, #6572, #29688, #26466, #15483, #499, #32529, #18147, #27038, #9975, #32155, #3722, #15294, #6195, #20994, #23825, #14917, #17767, #32345, #21180, #26654, #35367, #9419, #29309, #35933, #32907, #12065, #1249, #12635, #3348, #6382, #35562, #23639 ),
 ( #18333, #26846, #876, #12448, #3540, #3911, #6759, #9606, #12819, #32720, #29878, #6961, #1062, #35182, #24017, #17957, #685, #29500, #9228, #15104, #20802, #24200, #35745, #9791, #12256, #21368, #18529, #30067, #4102, #15674, #27224, #24388, #24936, #30819, #30259, #13383, #22294, #10534, #22110, #31009, #16422, #19279, #36491, #24569, #1815, #10163, #36862, #33659, #5030, #27788, #7887, #18902, #7699, #36123, #10349, #4843, #15862, #27969, #2000, #2182, #33847, #13573, #25125, #36302, #36682, #7145, #30454, #10720, #21922, #16237, #19460, #21738, #16609, #33471, #7514, #28152, #19087, #33289, #13764, #25310, #21555, #33102, #18719, #4285, #27407, #30638, #1439, #13015, #7328, #4655, #4472, #16051, #27598, #1629, #13201, #24753, #8810, #22481, #11096, #5394, #20191, #31554, #37234, #13947, #26229, #8259, #16974, #11282, #20382, #17534, #31371, #5578, #14313, #8439, #25684, #16791, #28516, #34768, #2925, #22670, #34214, #11465, #19832, #2741, #31741, #31924, #37048, #25866, #2559, #14128, #22852, #34402, #20008, #5214, #5955, #28704, #17164, #19649, #37415, #34028, #8622, #23034, #34581, #5768, #31191, #17348, #28891, #28336, #8074, #10907, #14494, #26051, #78, #2373, #11643, #23219, #29069, #3113, #14679, #25496, #35511, #29641, #3298, #18100, #26417, #15621, #829, #9747, #6526, #24152, #35131, #26797, #14870, #26607, #9557, #32107, #12396, #6713, #18479, #1012, #15246, #23968, #15058, #21133, #23401, #9182, #3677, #636, #32479, #35695, #451, #32670, #12206 ),
 ( #18284, #29827, #3864, #12586, #15437, #23779, #26986, #21320, #17718, #35317, #32857, #9371, #20946, #6907, #30019, #12019, #4049, #11830, #23589, #32297, #267, #34949, #8995, #20751, #20565, #6336, #17908, #6141, #29258, #29452, #3487, #10298, #30592, #24703, #4422, #33052, #21687, #13518, #19228, #1391, #27361, #27736, #12965, #19041, #10481, #36629, #15812, #4607, #33239, #30399, #27551, #16004, #24523, #21508, #25075, #7461, #7278, #16187, #1767, #27917, #33612, #9926, #1578, #36072, #18852, #10116, #13150, #36255, #35883, #21870, #24342, #13333, #33423, #24891, #36441, #22060, #7651, #30772, #4794, #7837, #16372, #1947, #10669, #22248, #33799, #19409, #7099, #18667, #30959, #4977, #27175, #30208, #1199, #12772, #4235, #16558, #31, #31876, #11596, #11228, #22431, #22799, #10858, #19785, #16741, #19595, #34350, #33979, #31505, #14079, #5527, #31322, #28105, #34715, #5163, #34534, #19962, #17114, #31688, #8760, #5717, #5350, #20334, #37185, #8393, #23171, #16927, #8020, #26002, #31143, #11042, #17298, #28288, #28469, #2326, #20142, #2136, #11416, #28653, #13898, #13715, #2690, #34165, #25446, #14266, #36999, #22618, #25817, #37363, #25264, #22984, #28839, #36815, #8573, #8209, #2508, #25629, #2873, #14446, #221, #29018, #17863, #3439, #11785, #26750, #23353, #6287, #29408, #781, #21278, #5906, #15008, #26560, #17486, #32247, #35088, #26183, #3064, #6090, #32437, #404, #9138, #20703, #14633, #9701, #6665, #34905, #12546, #23923, #8949, #17674, #9325, #20522 ) ),
 .UNSPECIFIED., .T., .F., .F. ) 
 B_SPLINE_SURFACE_WITH_KNOTS ( ( 4, 3, 4 ),
 ( 3, 2, 2, 2, 2, 2, 2, 2, 2, 2, 2, 2, 2, 2, 2, 2, 2, 2, 2, 2, 2, 2, 2, 2, 2, 2, 2, 2, 2, 2, 2, 2, 2, 2, 2, 2, 2, 2, 2, 2, 2, 2, 2, 2, 2, 2, 2, 2, 2, 2, 2, 2, 2, 2, 2, 2, 2, 2, 2, 2, 2, 2, 2, 2, 2, 2, 2, 2, 2, 2, 2, 2, 2, 2, 2, 2, 2, 2, 2, 2, 2, 2, 2, 2, 2, 2, 2, 2, 2, 2, 2, 2, 2, 2, 2, 2, 3 ),
 ( 0.000000000000000000, 0.5000000000000000000, 1.000000000000000000 ),
 ( 0.000000000000000000, 0.01041666666666666609, 0.02083333333333333218, 0.03125000000000000000, 0.04166666666666666435, 0.05208333333333333565, 0.06250000000000000000, 0.07291666666666667129, 0.08333333333333332871, 0.09375000000000000000, 0.1041666666666666713, 0.1145833333333333287, 0.1250000000000000000, 0.1354166666666666574, 0.1458333333333333426, 0.1562500000000000000, 0.1666666666666666574, 0.1770833333333333426, 0.1875000000000000000, 0.1979166666666666574, 0.2083333333333333426, 0.2187500000000000000, 0.2291666666666666574, 0.2395833333333333426, 0.2500000000000000000, 0.2604166666666666852, 0.2708333333333333148, 0.2812500000000000000, 0.2916666666666666852, 0.3020833333333333148, 0.3125000000000000000, 0.3229166666666666852, 0.3333333333333333148, 0.3437500000000000000, 0.3541666666666666852, 0.3645833333333333148, 0.3750000000000000000, 0.3854166666666666852, 0.3958333333333333148, 0.4062500000000000000, 0.4166666666666666852, 0.4270833333333333148, 0.4375000000000000000, 0.4479166666666666852, 0.4583333333333333148, 0.4687500000000000000, 0.4791666666666666852, 0.4895833333333333148, 0.5000000000000000000, 0.5104166666666666297, 0.5208333333333333703, 0.5312500000000000000, 0.5416666666666666297, 0.5520833333333333703, 0.5625000000000000000, 0.5729166666666666297, 0.5833333333333333703, 0.5937500000000000000, 0.6041666666666666297, 0.6145833333333333703, 0.6250000000000000000, 0.6354166666666666297, 0.6458333333333333703, 0.6562500000000000000, 0.6666666666666666297, 0.6770833333333333703, 0.6875000000000000000, 0.6979166666666666297, 0.7083333333333333703, 0.7187500000000000000, 0.7291666666666666297, 0.7395833333333333703, 0.7500000000000000000, 0.7604166666666666297, 0.7708333333333333703, 0.7812500000000000000, 0.7916666666666666297, 0.8020833333333333703, 0.8125000000000000000, 0.8229166666666666297, 0.8333333333333333703, 0.8437500000000000000, 0.8541666666666666297, 0.8645833333333333703, 0.8750000000000000000, 0.8854166666666666297, 0.8958333333333333703, 0.9062500000000000000, 0.9166666666666666297, 0.9270833333333333703, 0.9375000000000000000, 0.9479166666666666297, 0.9583333333333333703, 0.9687500000000000000, 0.9791666666666666297, 0.9895833333333333703, 1.000000000000000000 ),
 .UNSPECIFIED. ) 
 GEOMETRIC_REPRESENTATION_ITEM ( )  RATIONAL_B_SPLINE_SURFACE ( (
 ( 1.000000000000000000, 0.9659258262890683122, 1.000000000000000000, 0.9659258262890683122, 1.000000000000000000, 0.9659258262890683122, 1.000000000000000000, 0.9659258262890683122, 1.000000000000000000, 0.9659258262890683122, 1.000000000000000000, 0.9659258262890683122, 1.000000000000000000, 0.9659258262890683122, 1.000000000000000000, 0.9659258262890683122, 1.000000000000000000, 0.9659258262890683122, 1.000000000000000000, 0.9659258262890683122, 1.000000000000000000, 0.9659258262890683122, 1.000000000000000000, 0.9659258262890683122, 1.000000000000000000, 0.9659258262890683122, 1.000000000000000000, 0.9659258262890683122, 1.000000000000000000, 0.9659258262890683122, 1.000000000000000000, 0.9659258262890683122, 1.000000000000000000, 0.9659258262890683122, 1.000000000000000000, 0.9659258262890683122, 1.000000000000000000, 0.9659258262890683122, 1.000000000000000000, 0.9659258262890683122, 1.000000000000000000, 0.9659258262890683122, 1.000000000000000000, 0.9659258262890683122, 1.000000000000000000, 0.9659258262890683122, 1.000000000000000000, 0.9659258262890683122, 1.000000000000000000, 0.9659258262890683122, 1.000000000000000000, 0.9659258262890683122, 1.000000000000000000, 0.9659258262890683122, 1.000000000000000000, 0.9659258262890683122, 1.000000000000000000, 0.9659258262890683122, 1.000000000000000000, 0.9659258262890683122, 1.000000000000000000, 0.9659258262890683122, 1.000000000000000000, 0.9659258262890683122, 1.000000000000000000, 0.9659258262890683122, 1.000000000000000000, 0.9659258262890683122, 1.000000000000000000, 0.9659258262890683122, 1.000000000000000000, 0.9659258262890683122, 1.000000000000000000, 0.9659258262890683122, 1.000000000000000000, 0.9659258262890683122, 1.000000000000000000, 0.9659258262890683122, 1.000000000000000000, 0.9659258262890683122, 1.000000000000000000, 0.9659258262890683122, 1.000000000000000000, 0.9659258262890683122, 1.000000000000000000, 0.9659258262890683122, 1.000000000000000000, 0.9659258262890683122, 1.000000000000000000, 0.9659258262890683122, 1.000000000000000000, 0.9659258262890683122, 1.000000000000000000, 0.9659258262890683122, 1.000000000000000000, 0.9659258262890683122, 1.000000000000000000, 0.9659258262890683122, 1.000000000000000000, 0.9659258262890683122, 1.000000000000000000, 0.9659258262890683122, 1.000000000000000000, 0.9659258262890683122, 1.000000000000000000, 0.9659258262890683122, 1.000000000000000000, 0.9659258262890683122, 1.000000000000000000, 0.9659258262890683122, 1.000000000000000000, 0.9659258262890683122, 1.000000000000000000, 0.9659258262890683122, 1.000000000000000000, 0.9659258262890683122, 1.000000000000000000, 0.9659258262890683122, 1.000000000000000000, 0.9659258262890683122, 1.000000000000000000, 0.9659258262890683122, 1.000000000000000000, 0.9659258262890683122, 1.000000000000000000, 0.9659258262890683122, 1.000000000000000000, 0.9659258262890683122, 1.000000000000000000, 0.9659258262890683122, 1.000000000000000000, 0.9659258262890683122, 1.000000000000000000, 0.9659258262890683122, 1.000000000000000000, 0.9659258262890683122, 1.000000000000000000, 0.9659258262890683122, 1.000000000000000000, 0.9659258262890683122, 1.000000000000000000, 0.9659258262890683122, 1.000000000000000000, 0.9659258262890683122, 1.000000000000000000, 0.9659258262890683122, 1.000000000000000000, 0.9659258262890683122, 1.000000000000000000, 0.9659258262890683122, 1.000000000000000000, 0.9659258262890683122, 1.000000000000000000, 0.9659258262890683122, 1.000000000000000000, 0.9659258262890683122, 1.000000000000000000, 0.9659258262890683122, 1.000000000000000000, 0.9659258262890683122, 1.000000000000000000, 0.9659258262890683122, 1.000000000000000000, 0.9659258262890683122, 1.000000000000000000, 0.9659258262890683122, 1.000000000000000000, 0.9659258262890683122, 1.000000000000000000, 0.9659258262890683122, 1.000000000000000000, 0.9659258262890683122, 1.000000000000000000, 0.9659258262890683122, 1.000000000000000000, 0.9659258262890683122, 1.000000000000000000, 0.9659258262890683122, 1.000000000000000000, 0.9659258262890683122, 1.000000000000000000, 0.9659258262890683122, 1.000000000000000000, 0.9659258262890683122, 1.000000000000000000, 0.9659258262890683122, 1.000000000000000000, 0.9659258262890683122, 1.000000000000000000, 0.9659258262890683122, 1.000000000000000000, 0.9659258262890683122, 1.000000000000000000),
 ( 0.3333333333333333703, 0.3219752754296894559, 0.3333333333333333703, 0.3219752754296894559, 0.3333333333333333703, 0.3219752754296894559, 0.3333333333333333703, 0.3219752754296894559, 0.3333333333333333703, 0.3219752754296894559, 0.3333333333333333703, 0.3219752754296894559, 0.3333333333333333703, 0.3219752754296894559, 0.3333333333333333703, 0.3219752754296894559, 0.3333333333333333703, 0.3219752754296894559, 0.3333333333333333703, 0.3219752754296894559, 0.3333333333333333703, 0.3219752754296894559, 0.3333333333333333703, 0.3219752754296894559, 0.3333333333333333703, 0.3219752754296894559, 0.3333333333333333703, 0.3219752754296894559, 0.3333333333333333703, 0.3219752754296894559, 0.3333333333333333703, 0.3219752754296894559, 0.3333333333333333703, 0.3219752754296894559, 0.3333333333333333703, 0.3219752754296894559, 0.3333333333333333703, 0.3219752754296894559, 0.3333333333333333703, 0.3219752754296894559, 0.3333333333333333703, 0.3219752754296894559, 0.3333333333333333703, 0.3219752754296894559, 0.3333333333333333703, 0.3219752754296894559, 0.3333333333333333703, 0.3219752754296894559, 0.3333333333333333703, 0.3219752754296894559, 0.3333333333333333703, 0.3219752754296894559, 0.3333333333333333703, 0.3219752754296894559, 0.3333333333333333703, 0.3219752754296894559, 0.3333333333333333703, 0.3219752754296894559, 0.3333333333333333703, 0.3219752754296894559, 0.3333333333333333703, 0.3219752754296894559, 0.3333333333333333703, 0.3219752754296894559, 0.3333333333333333703, 0.3219752754296894559, 0.3333333333333333703, 0.3219752754296894559, 0.3333333333333333703, 0.3219752754296894559, 0.3333333333333333703, 0.3219752754296894559, 0.3333333333333333703, 0.3219752754296894559, 0.3333333333333333703, 0.3219752754296894559, 0.3333333333333333703, 0.3219752754296894559, 0.3333333333333333703, 0.3219752754296894559, 0.3333333333333333703, 0.3219752754296894559, 0.3333333333333333703, 0.3219752754296894559, 0.3333333333333333703, 0.3219752754296894559, 0.3333333333333333703, 0.3219752754296894559, 0.3333333333333333703, 0.3219752754296894559, 0.3333333333333333703, 0.3219752754296894559, 0.3333333333333333703, 0.3219752754296894559, 0.3333333333333333703, 0.3219752754296894559, 0.3333333333333333703, 0.3219752754296894559, 0.3333333333333333703, 0.3219752754296894559, 0.3333333333333333703, 0.3219752754296894559, 0.3333333333333333703, 0.3219752754296894559, 0.3333333333333333703, 0.3219752754296894559, 0.3333333333333333703, 0.3219752754296894559, 0.3333333333333333703, 0.3219752754296894559, 0.3333333333333333703, 0.3219752754296894559, 0.3333333333333333703, 0.3219752754296894559, 0.3333333333333333703, 0.3219752754296894559, 0.3333333333333333703, 0.3219752754296894559, 0.3333333333333333703, 0.3219752754296894559, 0.3333333333333333703, 0.3219752754296894559, 0.3333333333333333703, 0.3219752754296894559, 0.3333333333333333703, 0.3219752754296894559, 0.3333333333333333703, 0.3219752754296894559, 0.3333333333333333703, 0.3219752754296894559, 0.3333333333333333703, 0.3219752754296894559, 0.3333333333333333703, 0.3219752754296894559, 0.3333333333333333703, 0.3219752754296894559, 0.3333333333333333703, 0.3219752754296894559, 0.3333333333333333703, 0.3219752754296894559, 0.3333333333333333703, 0.3219752754296894559, 0.3333333333333333703, 0.3219752754296894559, 0.3333333333333333703, 0.3219752754296894559, 0.3333333333333333703, 0.3219752754296894559, 0.3333333333333333703, 0.3219752754296894559, 0.3333333333333333703, 0.3219752754296894559, 0.3333333333333333703, 0.3219752754296894559, 0.3333333333333333703, 0.3219752754296894559, 0.3333333333333333703, 0.3219752754296894559, 0.3333333333333333703, 0.3219752754296894559, 0.3333333333333333703, 0.3219752754296894559, 0.3333333333333333703, 0.3219752754296894559, 0.3333333333333333703, 0.3219752754296894559, 0.3333333333333333703, 0.3219752754296894559, 0.3333333333333333703, 0.3219752754296894559, 0.3333333333333333703, 0.3219752754296894559, 0.3333333333333333703, 0.3219752754296894559, 0.3333333333333333703, 0.3219752754296894559, 0.3333333333333333703, 0.3219752754296894559, 0.3333333333333333703, 0.3219752754296894559, 0.3333333333333333703, 0.3219752754296894559, 0.3333333333333333703, 0.3219752754296894559, 0.3333333333333333703, 0.3219752754296894559, 0.3333333333333333703, 0.3219752754296894559, 0.3333333333333333703, 0.3219752754296894559, 0.3333333333333333703, 0.3219752754296894559, 0.3333333333333333703),
 ( 0.3333333333333333703, 0.3219752754296894559, 0.3333333333333333703, 0.3219752754296894559, 0.3333333333333333703, 0.3219752754296894559, 0.3333333333333333703, 0.3219752754296894559, 0.3333333333333333703, 0.3219752754296894559, 0.3333333333333333703, 0.3219752754296894559, 0.3333333333333333703, 0.3219752754296894559, 0.3333333333333333703, 0.3219752754296894559, 0.3333333333333333703, 0.3219752754296894559, 0.3333333333333333703, 0.3219752754296894559, 0.3333333333333333703, 0.3219752754296894559, 0.3333333333333333703, 0.3219752754296894559, 0.3333333333333333703, 0.3219752754296894559, 0.3333333333333333703, 0.3219752754296894559, 0.3333333333333333703, 0.3219752754296894559, 0.3333333333333333703, 0.3219752754296894559, 0.3333333333333333703, 0.3219752754296894559, 0.3333333333333333703, 0.3219752754296894559, 0.3333333333333333703, 0.3219752754296894559, 0.3333333333333333703, 0.3219752754296894559, 0.3333333333333333703, 0.3219752754296894559, 0.3333333333333333703, 0.3219752754296894559, 0.3333333333333333703, 0.3219752754296894559, 0.3333333333333333703, 0.3219752754296894559, 0.3333333333333333703, 0.3219752754296894559, 0.3333333333333333703, 0.3219752754296894559, 0.3333333333333333703, 0.3219752754296894559, 0.3333333333333333703, 0.3219752754296894559, 0.3333333333333333703, 0.3219752754296894559, 0.3333333333333333703, 0.3219752754296894559, 0.3333333333333333703, 0.3219752754296894559, 0.3333333333333333703, 0.3219752754296894559, 0.3333333333333333703, 0.3219752754296894559, 0.3333333333333333703, 0.3219752754296894559, 0.3333333333333333703, 0.3219752754296894559, 0.3333333333333333703, 0.3219752754296894559, 0.3333333333333333703, 0.3219752754296894559, 0.3333333333333333703, 0.3219752754296894559, 0.3333333333333333703, 0.3219752754296894559, 0.3333333333333333703, 0.3219752754296894559, 0.3333333333333333703, 0.3219752754296894559, 0.3333333333333333703, 0.3219752754296894559, 0.3333333333333333703, 0.3219752754296894559, 0.3333333333333333703, 0.3219752754296894559, 0.3333333333333333703, 0.3219752754296894559, 0.3333333333333333703, 0.3219752754296894559, 0.3333333333333333703, 0.3219752754296894559, 0.3333333333333333703, 0.3219752754296894559, 0.3333333333333333703, 0.3219752754296894559, 0.3333333333333333703, 0.3219752754296894559, 0.3333333333333333703, 0.3219752754296894559, 0.3333333333333333703, 0.3219752754296894559, 0.3333333333333333703, 0.3219752754296894559, 0.3333333333333333703, 0.3219752754296894559, 0.3333333333333333703, 0.3219752754296894559, 0.3333333333333333703, 0.3219752754296894559, 0.3333333333333333703, 0.3219752754296894559, 0.3333333333333333703, 0.3219752754296894559, 0.3333333333333333703, 0.3219752754296894559, 0.3333333333333333703, 0.3219752754296894559, 0.3333333333333333703, 0.3219752754296894559, 0.3333333333333333703, 0.3219752754296894559, 0.3333333333333333703, 0.3219752754296894559, 0.3333333333333333703, 0.3219752754296894559, 0.3333333333333333703, 0.3219752754296894559, 0.3333333333333333703, 0.3219752754296894559, 0.3333333333333333703, 0.3219752754296894559, 0.3333333333333333703, 0.3219752754296894559, 0.3333333333333333703, 0.3219752754296894559, 0.3333333333333333703, 0.3219752754296894559, 0.3333333333333333703, 0.3219752754296894559, 0.3333333333333333703, 0.3219752754296894559, 0.3333333333333333703, 0.3219752754296894559, 0.3333333333333333703, 0.3219752754296894559, 0.3333333333333333703, 0.3219752754296894559, 0.3333333333333333703, 0.3219752754296894559, 0.3333333333333333703, 0.3219752754296894559, 0.3333333333333333703, 0.3219752754296894559, 0.3333333333333333703, 0.3219752754296894559, 0.3333333333333333703, 0.3219752754296894559, 0.3333333333333333703, 0.3219752754296894559, 0.3333333333333333703, 0.3219752754296894559, 0.3333333333333333703, 0.3219752754296894559, 0.3333333333333333703, 0.3219752754296894559, 0.3333333333333333703, 0.3219752754296894559, 0.3333333333333333703, 0.3219752754296894559, 0.3333333333333333703, 0.3219752754296894559, 0.3333333333333333703, 0.3219752754296894559, 0.3333333333333333703, 0.3219752754296894559, 0.3333333333333333703, 0.3219752754296894559, 0.3333333333333333703, 0.3219752754296894559, 0.3333333333333333703, 0.3219752754296894559, 0.3333333333333333703, 0.3219752754296894559, 0.3333333333333333703, 0.3219752754296894559, 0.3333333333333333703, 0.3219752754296894559, 0.3333333333333333703, 0.3219752754296894559, 0.3333333333333333703),
 ( 1.000000000000000000, 0.9659258262890683122, 1.000000000000000000, 0.9659258262890683122, 1.000000000000000000, 0.9659258262890683122, 1.000000000000000000, 0.9659258262890683122, 1.000000000000000000, 0.9659258262890683122, 1.000000000000000000, 0.9659258262890683122, 1.000000000000000000, 0.9659258262890683122, 1.000000000000000000, 0.9659258262890683122, 1.000000000000000000, 0.9659258262890683122, 1.000000000000000000, 0.9659258262890683122, 1.000000000000000000, 0.9659258262890683122, 1.000000000000000000, 0.9659258262890683122, 1.000000000000000000, 0.9659258262890683122, 1.000000000000000000, 0.9659258262890683122, 1.000000000000000000, 0.9659258262890683122, 1.000000000000000000, 0.9659258262890683122, 1.000000000000000000, 0.9659258262890683122, 1.000000000000000000, 0.9659258262890683122, 1.000000000000000000, 0.9659258262890683122, 1.000000000000000000, 0.9659258262890683122, 1.000000000000000000, 0.9659258262890683122, 1.000000000000000000, 0.9659258262890683122, 1.000000000000000000, 0.9659258262890683122, 1.000000000000000000, 0.9659258262890683122, 1.000000000000000000, 0.9659258262890683122, 1.000000000000000000, 0.9659258262890683122, 1.000000000000000000, 0.9659258262890683122, 1.000000000000000000, 0.9659258262890683122, 1.000000000000000000, 0.9659258262890683122, 1.000000000000000000, 0.9659258262890683122, 1.000000000000000000, 0.9659258262890683122, 1.000000000000000000, 0.9659258262890683122, 1.000000000000000000, 0.9659258262890683122, 1.000000000000000000, 0.9659258262890683122, 1.000000000000000000, 0.9659258262890683122, 1.000000000000000000, 0.9659258262890683122, 1.000000000000000000, 0.9659258262890683122, 1.000000000000000000, 0.9659258262890683122, 1.000000000000000000, 0.9659258262890683122, 1.000000000000000000, 0.9659258262890683122, 1.000000000000000000, 0.9659258262890683122, 1.000000000000000000, 0.9659258262890683122, 1.000000000000000000, 0.9659258262890683122, 1.000000000000000000, 0.9659258262890683122, 1.000000000000000000, 0.9659258262890683122, 1.000000000000000000, 0.9659258262890683122, 1.000000000000000000, 0.9659258262890683122, 1.000000000000000000, 0.9659258262890683122, 1.000000000000000000, 0.9659258262890683122, 1.000000000000000000, 0.9659258262890683122, 1.000000000000000000, 0.9659258262890683122, 1.000000000000000000, 0.9659258262890683122, 1.000000000000000000, 0.9659258262890683122, 1.000000000000000000, 0.9659258262890683122, 1.000000000000000000, 0.9659258262890683122, 1.000000000000000000, 0.9659258262890683122, 1.000000000000000000, 0.9659258262890683122, 1.000000000000000000, 0.9659258262890683122, 1.000000000000000000, 0.9659258262890683122, 1.000000000000000000, 0.9659258262890683122, 1.000000000000000000, 0.9659258262890683122, 1.000000000000000000, 0.9659258262890683122, 1.000000000000000000, 0.9659258262890683122, 1.000000000000000000, 0.9659258262890683122, 1.000000000000000000, 0.9659258262890683122, 1.000000000000000000, 0.9659258262890683122, 1.000000000000000000, 0.9659258262890683122, 1.000000000000000000, 0.9659258262890683122, 1.000000000000000000, 0.9659258262890683122, 1.000000000000000000, 0.9659258262890683122, 1.000000000000000000, 0.9659258262890683122, 1.000000000000000000, 0.9659258262890683122, 1.000000000000000000, 0.9659258262890683122, 1.000000000000000000, 0.9659258262890683122, 1.000000000000000000, 0.9659258262890683122, 1.000000000000000000, 0.9659258262890683122, 1.000000000000000000, 0.9659258262890683122, 1.000000000000000000, 0.9659258262890683122, 1.000000000000000000, 0.9659258262890683122, 1.000000000000000000, 0.9659258262890683122, 1.000000000000000000, 0.9659258262890683122, 1.000000000000000000, 0.9659258262890683122, 1.000000000000000000, 0.9659258262890683122, 1.000000000000000000, 0.9659258262890683122, 1.000000000000000000, 0.9659258262890683122, 1.000000000000000000, 0.9659258262890683122, 1.000000000000000000, 0.9659258262890683122, 1.000000000000000000, 0.9659258262890683122, 1.000000000000000000, 0.9659258262890683122, 1.000000000000000000, 0.9659258262890683122, 1.000000000000000000, 0.9659258262890683122, 1.000000000000000000, 0.9659258262890683122, 1.000000000000000000, 0.9659258262890683122, 1.000000000000000000, 0.9659258262890683122, 1.000000000000000000, 0.9659258262890683122, 1.000000000000000000, 0.9659258262890683122, 1.000000000000000000),
 ( 0.3333333333333333703, 0.3219752754296894559, 0.3333333333333333703, 0.3219752754296894559, 0.3333333333333333703, 0.3219752754296894559, 0.3333333333333333703, 0.3219752754296894559, 0.3333333333333333703, 0.3219752754296894559, 0.3333333333333333703, 0.3219752754296894559, 0.3333333333333333703, 0.3219752754296894559, 0.3333333333333333703, 0.3219752754296894559, 0.3333333333333333703, 0.3219752754296894559, 0.3333333333333333703, 0.3219752754296894559, 0.3333333333333333703, 0.3219752754296894559, 0.3333333333333333703, 0.3219752754296894559, 0.3333333333333333703, 0.3219752754296894559, 0.3333333333333333703, 0.3219752754296894559, 0.3333333333333333703, 0.3219752754296894559, 0.3333333333333333703, 0.3219752754296894559, 0.3333333333333333703, 0.3219752754296894559, 0.3333333333333333703, 0.3219752754296894559, 0.3333333333333333703, 0.3219752754296894559, 0.3333333333333333703, 0.3219752754296894559, 0.3333333333333333703, 0.3219752754296894559, 0.3333333333333333703, 0.3219752754296894559, 0.3333333333333333703, 0.3219752754296894559, 0.3333333333333333703, 0.3219752754296894559, 0.3333333333333333703, 0.3219752754296894559, 0.3333333333333333703, 0.3219752754296894559, 0.3333333333333333703, 0.3219752754296894559, 0.3333333333333333703, 0.3219752754296894559, 0.3333333333333333703, 0.3219752754296894559, 0.3333333333333333703, 0.3219752754296894559, 0.3333333333333333703, 0.3219752754296894559, 0.3333333333333333703, 0.3219752754296894559, 0.3333333333333333703, 0.3219752754296894559, 0.3333333333333333703, 0.3219752754296894559, 0.3333333333333333703, 0.3219752754296894559, 0.3333333333333333703, 0.3219752754296894559, 0.3333333333333333703, 0.3219752754296894559, 0.3333333333333333703, 0.3219752754296894559, 0.3333333333333333703, 0.3219752754296894559, 0.3333333333333333703, 0.3219752754296894559, 0.3333333333333333703, 0.3219752754296894559, 0.3333333333333333703, 0.3219752754296894559, 0.3333333333333333703, 0.3219752754296894559, 0.3333333333333333703, 0.3219752754296894559, 0.3333333333333333703, 0.3219752754296894559, 0.3333333333333333703, 0.3219752754296894559, 0.3333333333333333703, 0.3219752754296894559, 0.3333333333333333703, 0.3219752754296894559, 0.3333333333333333703, 0.3219752754296894559, 0.3333333333333333703, 0.3219752754296894559, 0.3333333333333333703, 0.3219752754296894559, 0.3333333333333333703, 0.3219752754296894559, 0.3333333333333333703, 0.3219752754296894559, 0.3333333333333333703, 0.3219752754296894559, 0.3333333333333333703, 0.3219752754296894559, 0.3333333333333333703, 0.3219752754296894559, 0.3333333333333333703, 0.3219752754296894559, 0.3333333333333333703, 0.3219752754296894559, 0.3333333333333333703, 0.3219752754296894559, 0.3333333333333333703, 0.3219752754296894559, 0.3333333333333333703, 0.3219752754296894559, 0.3333333333333333703, 0.3219752754296894559, 0.3333333333333333703, 0.3219752754296894559, 0.3333333333333333703, 0.3219752754296894559, 0.3333333333333333703, 0.3219752754296894559, 0.3333333333333333703, 0.3219752754296894559, 0.3333333333333333703, 0.3219752754296894559, 0.3333333333333333703, 0.3219752754296894559, 0.3333333333333333703, 0.3219752754296894559, 0.3333333333333333703, 0.3219752754296894559, 0.3333333333333333703, 0.3219752754296894559, 0.3333333333333333703, 0.3219752754296894559, 0.3333333333333333703, 0.3219752754296894559, 0.3333333333333333703, 0.3219752754296894559, 0.3333333333333333703, 0.3219752754296894559, 0.3333333333333333703, 0.3219752754296894559, 0.3333333333333333703, 0.3219752754296894559, 0.3333333333333333703, 0.3219752754296894559, 0.3333333333333333703, 0.3219752754296894559, 0.3333333333333333703, 0.3219752754296894559, 0.3333333333333333703, 0.3219752754296894559, 0.3333333333333333703, 0.3219752754296894559, 0.3333333333333333703, 0.3219752754296894559, 0.3333333333333333703, 0.3219752754296894559, 0.3333333333333333703, 0.3219752754296894559, 0.3333333333333333703, 0.3219752754296894559, 0.3333333333333333703, 0.3219752754296894559, 0.3333333333333333703, 0.3219752754296894559, 0.3333333333333333703, 0.3219752754296894559, 0.3333333333333333703, 0.3219752754296894559, 0.3333333333333333703, 0.3219752754296894559, 0.3333333333333333703, 0.3219752754296894559, 0.3333333333333333703, 0.3219752754296894559, 0.3333333333333333703, 0.3219752754296894559, 0.3333333333333333703, 0.3219752754296894559, 0.3333333333333333703, 0.3219752754296894559, 0.3333333333333333703),
 ( 0.3333333333333333703, 0.3219752754296894559, 0.3333333333333333703, 0.3219752754296894559, 0.3333333333333333703, 0.3219752754296894559, 0.3333333333333333703, 0.3219752754296894559, 0.3333333333333333703, 0.3219752754296894559, 0.3333333333333333703, 0.3219752754296894559, 0.3333333333333333703, 0.3219752754296894559, 0.3333333333333333703, 0.3219752754296894559, 0.3333333333333333703, 0.3219752754296894559, 0.3333333333333333703, 0.3219752754296894559, 0.3333333333333333703, 0.3219752754296894559, 0.3333333333333333703, 0.3219752754296894559, 0.3333333333333333703, 0.3219752754296894559, 0.3333333333333333703, 0.3219752754296894559, 0.3333333333333333703, 0.3219752754296894559, 0.3333333333333333703, 0.3219752754296894559, 0.3333333333333333703, 0.3219752754296894559, 0.3333333333333333703, 0.3219752754296894559, 0.3333333333333333703, 0.3219752754296894559, 0.3333333333333333703, 0.3219752754296894559, 0.3333333333333333703, 0.3219752754296894559, 0.3333333333333333703, 0.3219752754296894559, 0.3333333333333333703, 0.3219752754296894559, 0.3333333333333333703, 0.3219752754296894559, 0.3333333333333333703, 0.3219752754296894559, 0.3333333333333333703, 0.3219752754296894559, 0.3333333333333333703, 0.3219752754296894559, 0.3333333333333333703, 0.3219752754296894559, 0.3333333333333333703, 0.3219752754296894559, 0.3333333333333333703, 0.3219752754296894559, 0.3333333333333333703, 0.3219752754296894559, 0.3333333333333333703, 0.3219752754296894559, 0.3333333333333333703, 0.3219752754296894559, 0.3333333333333333703, 0.3219752754296894559, 0.3333333333333333703, 0.3219752754296894559, 0.3333333333333333703, 0.3219752754296894559, 0.3333333333333333703, 0.3219752754296894559, 0.3333333333333333703, 0.3219752754296894559, 0.3333333333333333703, 0.3219752754296894559, 0.3333333333333333703, 0.3219752754296894559, 0.3333333333333333703, 0.3219752754296894559, 0.3333333333333333703, 0.3219752754296894559, 0.3333333333333333703, 0.3219752754296894559, 0.3333333333333333703, 0.3219752754296894559, 0.3333333333333333703, 0.3219752754296894559, 0.3333333333333333703, 0.3219752754296894559, 0.3333333333333333703, 0.3219752754296894559, 0.3333333333333333703, 0.3219752754296894559, 0.3333333333333333703, 0.3219752754296894559, 0.3333333333333333703, 0.3219752754296894559, 0.3333333333333333703, 0.3219752754296894559, 0.3333333333333333703, 0.3219752754296894559, 0.3333333333333333703, 0.3219752754296894559, 0.3333333333333333703, 0.3219752754296894559, 0.3333333333333333703, 0.3219752754296894559, 0.3333333333333333703, 0.3219752754296894559, 0.3333333333333333703, 0.3219752754296894559, 0.3333333333333333703, 0.3219752754296894559, 0.3333333333333333703, 0.3219752754296894559, 0.3333333333333333703, 0.3219752754296894559, 0.3333333333333333703, 0.3219752754296894559, 0.3333333333333333703, 0.3219752754296894559, 0.3333333333333333703, 0.3219752754296894559, 0.3333333333333333703, 0.3219752754296894559, 0.3333333333333333703, 0.3219752754296894559, 0.3333333333333333703, 0.3219752754296894559, 0.3333333333333333703, 0.3219752754296894559, 0.3333333333333333703, 0.3219752754296894559, 0.3333333333333333703, 0.3219752754296894559, 0.3333333333333333703, 0.3219752754296894559, 0.3333333333333333703, 0.3219752754296894559, 0.3333333333333333703, 0.3219752754296894559, 0.3333333333333333703, 0.3219752754296894559, 0.3333333333333333703, 0.3219752754296894559, 0.3333333333333333703, 0.3219752754296894559, 0.3333333333333333703, 0.3219752754296894559, 0.3333333333333333703, 0.3219752754296894559, 0.3333333333333333703, 0.3219752754296894559, 0.3333333333333333703, 0.3219752754296894559, 0.3333333333333333703, 0.3219752754296894559, 0.3333333333333333703, 0.3219752754296894559, 0.3333333333333333703, 0.3219752754296894559, 0.3333333333333333703, 0.3219752754296894559, 0.3333333333333333703, 0.3219752754296894559, 0.3333333333333333703, 0.3219752754296894559, 0.3333333333333333703, 0.3219752754296894559, 0.3333333333333333703, 0.3219752754296894559, 0.3333333333333333703, 0.3219752754296894559, 0.3333333333333333703, 0.3219752754296894559, 0.3333333333333333703, 0.3219752754296894559, 0.3333333333333333703, 0.3219752754296894559, 0.3333333333333333703, 0.3219752754296894559, 0.3333333333333333703, 0.3219752754296894559, 0.3333333333333333703, 0.3219752754296894559, 0.3333333333333333703, 0.3219752754296894559, 0.3333333333333333703, 0.3219752754296894559, 0.3333333333333333703),
 ( 1.000000000000000000, 0.9659258262890683122, 1.000000000000000000, 0.9659258262890683122, 1.000000000000000000, 0.9659258262890683122, 1.000000000000000000, 0.9659258262890683122, 1.000000000000000000, 0.9659258262890683122, 1.000000000000000000, 0.9659258262890683122, 1.000000000000000000, 0.9659258262890683122, 1.000000000000000000, 0.9659258262890683122, 1.000000000000000000, 0.9659258262890683122, 1.000000000000000000, 0.9659258262890683122, 1.000000000000000000, 0.9659258262890683122, 1.000000000000000000, 0.9659258262890683122, 1.000000000000000000, 0.9659258262890683122, 1.000000000000000000, 0.9659258262890683122, 1.000000000000000000, 0.9659258262890683122, 1.000000000000000000, 0.9659258262890683122, 1.000000000000000000, 0.9659258262890683122, 1.000000000000000000, 0.9659258262890683122, 1.000000000000000000, 0.9659258262890683122, 1.000000000000000000, 0.9659258262890683122, 1.000000000000000000, 0.9659258262890683122, 1.000000000000000000, 0.9659258262890683122, 1.000000000000000000, 0.9659258262890683122, 1.000000000000000000, 0.9659258262890683122, 1.000000000000000000, 0.9659258262890683122, 1.000000000000000000, 0.9659258262890683122, 1.000000000000000000, 0.9659258262890683122, 1.000000000000000000, 0.9659258262890683122, 1.000000000000000000, 0.9659258262890683122, 1.000000000000000000, 0.9659258262890683122, 1.000000000000000000, 0.9659258262890683122, 1.000000000000000000, 0.9659258262890683122, 1.000000000000000000, 0.9659258262890683122, 1.000000000000000000, 0.9659258262890683122, 1.000000000000000000, 0.9659258262890683122, 1.000000000000000000, 0.9659258262890683122, 1.000000000000000000, 0.9659258262890683122, 1.000000000000000000, 0.9659258262890683122, 1.000000000000000000, 0.9659258262890683122, 1.000000000000000000, 0.9659258262890683122, 1.000000000000000000, 0.9659258262890683122, 1.000000000000000000, 0.9659258262890683122, 1.000000000000000000, 0.9659258262890683122, 1.000000000000000000, 0.9659258262890683122, 1.000000000000000000, 0.9659258262890683122, 1.000000000000000000, 0.9659258262890683122, 1.000000000000000000, 0.9659258262890683122, 1.000000000000000000, 0.9659258262890683122, 1.000000000000000000, 0.9659258262890683122, 1.000000000000000000, 0.9659258262890683122, 1.000000000000000000, 0.9659258262890683122, 1.000000000000000000, 0.9659258262890683122, 1.000000000000000000, 0.9659258262890683122, 1.000000000000000000, 0.9659258262890683122, 1.000000000000000000, 0.9659258262890683122, 1.000000000000000000, 0.9659258262890683122, 1.000000000000000000, 0.9659258262890683122, 1.000000000000000000, 0.9659258262890683122, 1.000000000000000000, 0.9659258262890683122, 1.000000000000000000, 0.9659258262890683122, 1.000000000000000000, 0.9659258262890683122, 1.000000000000000000, 0.9659258262890683122, 1.000000000000000000, 0.9659258262890683122, 1.000000000000000000, 0.9659258262890683122, 1.000000000000000000, 0.9659258262890683122, 1.000000000000000000, 0.9659258262890683122, 1.000000000000000000, 0.9659258262890683122, 1.000000000000000000, 0.9659258262890683122, 1.000000000000000000, 0.9659258262890683122, 1.000000000000000000, 0.9659258262890683122, 1.000000000000000000, 0.9659258262890683122, 1.000000000000000000, 0.9659258262890683122, 1.000000000000000000, 0.9659258262890683122, 1.000000000000000000, 0.9659258262890683122, 1.000000000000000000, 0.9659258262890683122, 1.000000000000000000, 0.9659258262890683122, 1.000000000000000000, 0.9659258262890683122, 1.000000000000000000, 0.9659258262890683122, 1.000000000000000000, 0.9659258262890683122, 1.000000000000000000, 0.9659258262890683122, 1.000000000000000000, 0.9659258262890683122, 1.000000000000000000, 0.9659258262890683122, 1.000000000000000000, 0.9659258262890683122, 1.000000000000000000, 0.9659258262890683122, 1.000000000000000000, 0.9659258262890683122, 1.000000000000000000, 0.9659258262890683122, 1.000000000000000000, 0.9659258262890683122, 1.000000000000000000, 0.9659258262890683122, 1.000000000000000000, 0.9659258262890683122, 1.000000000000000000, 0.9659258262890683122, 1.000000000000000000, 0.9659258262890683122, 1.000000000000000000, 0.9659258262890683122, 1.000000000000000000, 0.9659258262890683122, 1.000000000000000000, 0.9659258262890683122, 1.000000000000000000, 0.9659258262890683122, 1.000000000000000000, 0.9659258262890683122, 1.000000000000000000) ) ) 
 REPRESENTATION_ITEM ( '' )  SURFACE ( )  );
#14814 = EDGE_CURVE ( 'NONE', #5242, #21580, #35700, .T. ) ;
#14815 = CYLINDRICAL_SURFACE ( 'NONE', #24990, 7.500000000000000000 ) ;
#14816 = EDGE_LOOP ( 'NONE', ( #33736, #29283, #28409 ) ) ;
#14817 = CARTESIAN_POINT ( 'NONE',  ( 16.56230152254411081, 7.209453229046482114, -3.909374999385482496 ) ) ;
#14818 = PRODUCT_RELATED_PRODUCT_CATEGORY ( 'part', '', ( #3198 ) ) ;
#14819 = CARTESIAN_POINT ( 'NONE',  ( -13.62178482187500528, 198.8281250006145342, -23.59362340125807123 ) ) ;
#14820 = CARTESIAN_POINT ( 'NONE',  ( 34.30304196422265761, 5.407089921784862696, 166.2360015760246199 ) ) ;
#14821 = CARTESIAN_POINT ( 'NONE',  ( -34.16294563604515133, 214.6737587650350747, -4.842901733360249317 ) ) ;
#14822 = CARTESIAN_POINT ( 'NONE',  ( 19.39230484541326049, 245.4638461906613998, -5.999999999999997335 ) ) ;
#14823 = FILL_AREA_STYLE_COLOUR ( '', #5056 ) ;
#14824 = DIRECTION ( 'NONE',  ( -1.000000000000000000, 0.000000000000000000, -0.000000000000000000 ) ) ;
#14825 = CARTESIAN_POINT ( 'NONE',  ( -57.71502896937850835, 213.8393509191290889, -2.350049139982142155 ) ) ;
#14826 = CARTESIAN_POINT ( 'NONE',  ( 34.03873067997093216, -5.196152422706629359, 164.6122338966858933 ) ) ;
#14827 = CARTESIAN_POINT ( 'NONE',  ( 25.19067013329413385, -3.604726614523240613, 169.5365065289374797 ) ) ;
#14828 = ORIENTED_EDGE ( 'NONE', *, *, #16506, .F. ) ;
#14829 =( BOUNDED_CURVE ( )  B_SPLINE_CURVE ( 2, ( #32764, #12490, #10208, #12865, #9648, #35410, #9832, #32951, #7004 ),
 .UNSPECIFIED., .F., .F. ) 
 B_SPLINE_CURVE_WITH_KNOTS ( ( 3, 2, 2, 2, 3 ),
 ( 0.6195652173913043237, 0.6231884057971014412, 0.6304347826086956763, 0.6376811594202898004, 0.6413043478260869179 ),
 .UNSPECIFIED. ) 
 CURVE ( )  GEOMETRIC_REPRESENTATION_ITEM ( )  RATIONAL_B_SPLINE_CURVE ( ( 0.9330127018922194093, 0.9330127018922194093, 1.000000000000000000, 0.8660254037844387076, 1.000000000000000000, 0.8660254037844387076, 1.000000000000000000, 0.9330127018922194093, 0.9330127018922194093 ) ) 
 REPRESENTATION_ITEM ( '' )  );
#14830 = CARTESIAN_POINT ( 'NONE',  ( -28.47956685997937498, 204.1588929126527603, 5.472637659619466355 ) ) ;
#14831 = CARTESIAN_POINT ( 'NONE',  ( -13.04141134922778456, 14.82731371789855324, 8.927990412390377273 ) ) ;
#14832 = CARTESIAN_POINT ( 'NONE',  ( -58.31622103062156981, 212.1620413398628671, 8.530955311639223382 ) ) ;
#14833 = CARTESIAN_POINT ( 'NONE',  ( 1.715153634034233487, 129.7226862821014208, 9.534712964251941258 ) ) ;
#14834 = CARTESIAN_POINT ( 'NONE',  ( -12.46528703574805697, 40.59768628210144215, -2.660918448318280838 ) ) ;
#14835 = CARTESIAN_POINT ( 'NONE',  ( 16.56230152254411436, 6.928203230275514990, -5.062500000000007994 ) ) ;
#14836 = ORIENTED_EDGE ( 'NONE', *, *, #670, .T. ) ;
#14837 = CARTESIAN_POINT ( 'NONE',  ( -43.67038769728823411, 208.1428034533959703, 6.469044688360771289 ) ) ;
#14838 = CARTESIAN_POINT ( 'NONE',  ( 7.234628195640269155, 195.1825961894323598, 27.00000000000003197 ) ) ;
#14839 = CARTESIAN_POINT ( 'NONE',  ( -9.465287035748065847, 22.19768628210144001, -2.064181346179273735 ) ) ;
#14840 = CARTESIAN_POINT ( 'NONE',  ( -1.926257025242585782E-15, 196.5968750006145456, -31.45816453501075927 ) ) ;
#14841 = DIRECTION ( 'NONE',  ( -0.000000000000000000, -1.000000000000000000, -0.000000000000000000 ) ) ;
#14842 = CARTESIAN_POINT ( 'NONE',  ( -6.000000000000000888, -20.00000000000000000, 20.00000000000000711 ) ) ;
#14843 = DIRECTION ( 'NONE',  ( 1.000000000000000000, 0.000000000000000000, 0.000000000000000000 ) ) ;
#14844 = CARTESIAN_POINT ( 'NONE',  ( 25.45210587809749825, 0.000000000000000000, 169.7300825181138748 ) ) ;
#14845 = CARTESIAN_POINT ( 'NONE',  ( 23.87821517812499650, 244.7593750006145399, -4.985214923628404904 ) ) ;
#14846 = CARTESIAN_POINT ( 'NONE',  ( -3.474262827703527901, 87.56481371789857349, 8.843639120294245259 ) ) ;
#14847 = CARTESIAN_POINT ( 'NONE',  ( 26.75643035624999655, 240.2218750006145456, -3.323476615752271268 ) ) ;
#14848 = EDGE_LOOP ( 'NONE', ( #21456, #35254, #8981, #28311 ) ) ;
#14849 = CARTESIAN_POINT ( 'NONE',  ( -52.77455436395490551, 205.1570982666397356, 4.673758765035198159 ) ) ;
#14850 = CARTESIAN_POINT ( 'NONE',  ( 15.00000000000000000, 247.3187500012290343, -3.464101615137752166 ) ) ;
#14851 = CARTESIAN_POINT ( 'NONE',  ( 10.49813415416005213, 93.02731371789856496, -7.228626920338837358 ) ) ;
#14852 = CARTESIAN_POINT ( 'NONE',  ( 10.31873187879410381, 3.604726614523240613, -1.134374999385481697 ) ) ;
#14853 = CARTESIAN_POINT ( 'NONE',  ( 30.65222614765988141, 7.209453229046475009, 160.3254497058415495 ) ) ;
#14854 = CARTESIAN_POINT ( 'NONE',  ( 26.75643035624999655, 3.323476615752271712, -1.790624999385476812 ) ) ;
#14855 = CARTESIAN_POINT ( 'NONE',  ( 12.46528703574811558, 66.00231371789855928, -2.660918448318005503 ) ) ;
#14856 = CARTESIAN_POINT ( 'NONE',  ( 27.24356964374999635, 197.8718750006145513, -15.72908226750539029 ) ) ;
#14857 = VECTOR ( 'NONE', #5799, 1000.000000000000000 ) ;
#14858 = ORIENTED_EDGE ( 'NONE', *, *, #20929, .F. ) ;
#14859 = ORIENTED_EDGE ( 'NONE', *, *, #36496, .F. ) ;
#14860 = CARTESIAN_POINT ( 'NONE',  ( 26.75643035624999655, 3.323476615752271268, -3.928124999385464999 ) ) ;
#14861 = CARTESIAN_POINT ( 'NONE',  ( 2.999999999999997335, 244.5000000000000000, 5.000000000000000000 ) ) ;
#14862 = CARTESIAN_POINT ( 'NONE',  ( 26.75643035624999655, 245.5093750006145115, -3.323476615752271712 ) ) ;
#14863 = CARTESIAN_POINT ( 'NONE',  ( -8.962234695871760692, 48.36018628210145209, 8.715434833791933400 ) ) ;
#14864 = CARTESIAN_POINT ( 'NONE',  ( -56.52752896937850124, 213.3500491399821613, 5.571401726697954970 ) ) ;
#14865 = CARTESIAN_POINT ( 'NONE',  ( -71.54107125509844423, 209.3291073423510795, -5.000000000000000000 ) ) ;
#14866 = CARTESIAN_POINT ( 'NONE',  ( -67.80877896937850835, 211.6261429550004607, -6.530955311639245586 ) ) ;
#14867 = CARTESIAN_POINT ( 'NONE',  ( 30.85077782416043135, -6.928203230275506996, 162.5949057530440029 ) ) ;
#14868 = CARTESIAN_POINT ( 'NONE',  ( 6.932735513424201024, 101.6523137178985650, -10.69584247140429412 ) ) ;
#14869 = CARTESIAN_POINT ( 'NONE',  ( -62.86830436395490551, 209.8844732041982297, 4.499999999999996447 ) ) ;
#14870 = CARTESIAN_POINT ( 'NONE',  ( -35.95163769728824121, 217.4189793300686233, -4.149950860017907139 ) ) ;
#14871 = CARTESIAN_POINT ( 'NONE',  ( 20.99999999999999645, 6.646953231504538984, -5.765624999385476457 ) ) ;
#14872 = CARTESIAN_POINT ( 'NONE',  ( -8.927990412390371944, 72.32731371789854791, -13.04141134922778988 ) ) ;
#14873 = CARTESIAN_POINT ( 'NONE',  ( -55.93377896937850124, 207.8379586601372750, 8.530955311639258909 ) ) ;
#14874 = CIRCLE ( 'NONE', #29396, 2.649999999999992806 ) ;
#14875 = ORIENTED_EDGE ( 'NONE', *, *, #1533, .F. ) ;
#14876 = CARTESIAN_POINT ( 'NONE',  ( 26.99999999999999645, 240.8125000000000000, -3.464101615137755275 ) ) ;
#14877 = CARTESIAN_POINT ( 'NONE',  ( -4.622313124798576922, 97.23518628210145209, -11.61527771782819762 ) ) ;
#14878 = CARTESIAN_POINT ( 'NONE',  ( -10.83675517735155047, 41.46018628210145351, -11.08355503943142750 ) ) ;
#14879 = CIRCLE ( 'NONE', #34843, 2.649999999999999467 ) ;
#14880 = DIRECTION ( 'NONE',  ( 0.000000000000000000, 0.9932091452657081376, 0.1163425707149433885 ) ) ;
#14881 = CARTESIAN_POINT ( 'NONE',  ( 27.54068648934820729, 5.407089921784862696, 160.5788525301012157 ) ) ;
#14882 = CARTESIAN_POINT ( 'NONE',  ( 13.04141134922759804, 64.17268628210143788, 8.927990412390657937 ) ) ;
#14883 = CARTESIAN_POINT ( 'NONE',  ( -13.62178482187500528, 199.7281250006145399, -23.59362340125807123 ) ) ;
#14884 = CARTESIAN_POINT ( 'NONE',  ( 22.80587116629410360, 3.604726614523238837, -8.428124999385516958 ) ) ;
#14885 = CARTESIAN_POINT ( 'NONE',  ( 26.99999999999999645, 7.347880794884117764E-16, -1.968749998770946696 ) ) ;
#14886 = CARTESIAN_POINT ( 'NONE',  ( -56.33705436395489841, 205.3262412349647263, -4.842901733360204020 ) ) ;
#14887 = DIRECTION ( 'NONE',  ( 0.000000000000000000, 0.000000000000000000, -1.000000000000000000 ) ) ;
#14888 = CARTESIAN_POINT ( 'NONE',  ( -10.49813415415989581, 41.17268628210144499, -7.228626920339068285 ) ) ;
#14889 = CARTESIAN_POINT ( 'NONE',  ( -13.62178482187500528, 199.3343750006145569, -23.59362340125807123 ) ) ;
#14890 = DIRECTION ( 'NONE',  ( 0.000000000000000000, 0.000000000000000000, -1.000000000000000000 ) ) ;
#14891 = CARTESIAN_POINT ( 'NONE',  ( 5.529263428287477744, 6.672686282101436106, -7.954856959092191815 ) ) ;
#14892 = CARTESIAN_POINT ( 'NONE',  ( 15.24356964374999990, 247.1218750006145228, -3.323476615752268604 ) ) ;
#14893 = ORIENTED_EDGE ( 'NONE', *, *, #10865, .T. ) ;
#14894 = CARTESIAN_POINT ( 'NONE',  ( 18.00000000000000000, 5.196152422706630247, -6.824999999999997513 ) ) ;
#14895 = DIRECTION ( 'NONE',  ( 1.000000000000000000, 0.000000000000000000, 0.000000000000000000 ) ) ;
#14896 = CARTESIAN_POINT ( 'NONE',  ( 27.00000000000001421, 197.4875000000000114, 15.58845726811988897 ) ) ;
#14897 = CARTESIAN_POINT ( 'NONE',  ( 22.80587116629411071, -3.604726614523235284, -4.903124999385513938 ) ) ;
#14898 = CARTESIAN_POINT ( 'NONE',  ( 37.33287311370841621, 7.646167579472015790E-16, 165.0486662223039218 ) ) ;
#14899 = CARTESIAN_POINT ( 'NONE',  ( 26.99999999999999645, 242.1624999999999659, -3.464101615137755275 ) ) ;
#14900 = CARTESIAN_POINT ( 'NONE',  ( 26.99999999999999645, 198.9124999999999943, -15.58845726811990495 ) ) ;
#14901 = CARTESIAN_POINT ( 'NONE',  ( 11.61527771782819940, 44.33518628210145351, -4.622313124798573369 ) ) ;
#14902 = ORIENTED_EDGE ( 'NONE', *, *, #34903, .F. ) ;
#14903 = ORIENTED_EDGE ( 'NONE', *, *, #12409, .F. ) ;
#14904 = CYLINDRICAL_SURFACE ( 'NONE', #16706, 6.000000000000001776 ) ;
#14905 = CARTESIAN_POINT ( 'NONE',  ( 18.12178482187500350, -4.985214923628407568, -5.915624999385471483 ) ) ;
#14906 = CARTESIAN_POINT ( 'NONE',  ( 6.932735513423970097, 92.34768628210144925, 10.69584247140445044 ) ) ;
#14907 = CARTESIAN_POINT ( 'NONE',  ( -8.632099005475794229, 23.45231371789854435, 13.23911966647199812 ) ) ;
#14908 = FACE_OUTER_BOUND ( 'NONE', #5978, .T. ) ;
#14909 = COLOUR_RGB ( '',0.8941176470588234615, 0.8941176470588234615, 0.8941176470588234615 ) ;
#14910 = CARTESIAN_POINT ( 'NONE',  ( 26.75643035624999655, 241.0468750006145058, 3.323476615752267715 ) ) ;
#14911 = CARTESIAN_POINT ( 'NONE',  ( -33.57663769728823411, 206.0451222850691408, 2.149950860017832532 ) ) ;
#14912 = CARTESIAN_POINT ( 'NONE',  ( 20.99999999999999645, 185.0294372515228645, 5.999999999999999112 ) ) ;
#14913 = CARTESIAN_POINT ( 'NONE',  ( 34.40478479951106294, 5.196152422706631135, 168.7962516286712571 ) ) ;
#14914 = CARTESIAN_POINT ( 'NONE',  ( -8.843639120294245259, 16.26481371789853370, -3.474262827703533230 ) ) ;
#14915 = CARTESIAN_POINT ( 'NONE',  ( -64.05580436395490551, 216.5000000000000000, 0.1155267958017343610 ) ) ;
#14916 =( BOUNDED_CURVE ( )  B_SPLINE_CURVE ( 2, ( #12083, #29520, #34830, #35387, #32741, #14563, #18165 ),
 .UNSPECIFIED., .F., .F. ) 
 B_SPLINE_CURVE_WITH_KNOTS ( ( 3, 2, 2, 3 ),
 ( 0.4782608695652158515, 0.4855072463768100866, 0.4927536231884043771, 0.4999999999999986122 ),
 .UNSPECIFIED. ) 
 CURVE ( )  GEOMETRIC_REPRESENTATION_ITEM ( )  RATIONAL_B_SPLINE_CURVE ( ( 1.000000000000028644, 0.8660254037844099528, 1.000000000000000000, 0.8660254037844387076, 1.000000000000000000, 0.8660254037844643538, 0.9999999999999743538 ) ) 
 REPRESENTATION_ITEM ( '' )  );
#14917 = CARTESIAN_POINT ( 'NONE',  ( -33.17336230271183695, 217.4189793300686233, 4.149950860017807663 ) ) ;
#14918 = PRODUCT_CONTEXT ( 'NONE', #8119, 'mechanical' ) ;
#14919 = CARTESIAN_POINT ( 'NONE',  ( 16.56230152254411081, 6.928203230275506996, -4.499999998770991105 ) ) ;
#14920 = CARTESIAN_POINT ( 'NONE',  ( -1.926257025242585782E-15, 196.5968750006145456, -31.45816453501075927 ) ) ;
#14921 = CARTESIAN_POINT ( 'NONE',  ( -0.1745138560722442889, 137.5898137178985792, -15.50000000000000533 ) ) ;
#14922 = CARTESIAN_POINT ( 'NONE',  ( -64.24627896937849414, 203.4690446883607535, -1.626142955000504209 ) ) ;
#14923 = CIRCLE ( 'NONE', #16738, 5.999999999999998224 ) ;
#14924 = ORIENTED_EDGE ( 'NONE', *, *, #4375, .F. ) ;
#14925 = CARTESIAN_POINT ( 'NONE',  ( 4.622313124798573369, 46.63518628210145067, 11.61527771782819940 ) ) ;
#14926 = CARTESIAN_POINT ( 'NONE',  ( 0.000000000000000000, -20.00000000000000000, 0.000000000000000000 ) ) ;
#14927 = ADVANCED_FACE ( 'NONE', ( #16908 ), #5886, .T. ) ;
#14928 = CARTESIAN_POINT ( 'NONE',  ( 25.00000000000004263, 0.000000000000000000, 49.82535622836640954 ) ) ;
#14929 = CARTESIAN_POINT ( 'NONE',  ( 31.17679477432231394, -7.209453229046482114, 166.3212965449812657 ) ) ;
#14930 = CARTESIAN_POINT ( 'NONE',  ( 23.99999999999999645, 5.196152422706631135, -3.243749998770945275 ) ) ;
#14931 = CARTESIAN_POINT ( 'NONE',  ( -64.64955436395490551, 214.8429017333601792, -4.673758765035197271 ) ) ;
#14932 = CARTESIAN_POINT ( 'NONE',  ( 13.44051670066911619, -5.407089921784859143, -0.9656249993855170466 ) ) ;
#14933 = CARTESIAN_POINT ( 'NONE',  ( -8.843639120294326972, 58.13518628210145067, 3.474262827703335166 ) ) ;
#14934 = CARTESIAN_POINT ( 'NONE',  ( 10.56230152254227228, -3.464101615136696122, -1.199999998771057008 ) ) ;
#14935 = PLANE ( 'NONE',  #14179 ) ;
#14936 =( BOUNDED_CURVE ( )  B_SPLINE_CURVE ( 2, ( #17795, #9071, #29338, #23474, #12091, #14945, #3376, #35209, #24727 ),
 .UNSPECIFIED., .F., .F. ) 
 B_SPLINE_CURVE_WITH_KNOTS ( ( 3, 2, 2, 2, 3 ),
 ( 0.6041666666666667407, 0.6111111111111111605, 0.6250000000000000000, 0.6388888888888888395, 0.6458333333333333703 ),
 .UNSPECIFIED. ) 
 CURVE ( )  GEOMETRIC_REPRESENTATION_ITEM ( )  RATIONAL_B_SPLINE_CURVE ( ( 0.9330127018922192983, 0.9330127018922198534, 1.000000000000000000, 0.8660254037844387076, 1.000000000000000000, 0.8660254037844387076, 1.000000000000000000, 0.9330127018922187432, 0.9330127018922192983 ) ) 
 REPRESENTATION_ITEM ( '' )  );
#14937 = CARTESIAN_POINT ( 'NONE',  ( -11.61527771782819940, 94.93518628210145494, 4.622313124798574258 ) ) ;
#14938 = DIRECTION ( 'NONE',  ( 0.000000000000000000, 0.000000000000000000, 1.000000000000000000 ) ) ;
#14939 = ORIENTED_EDGE ( 'NONE', *, *, #17291, .T. ) ;
#14940 = CARTESIAN_POINT ( 'NONE',  ( 36.86223210287109708, 7.646167579472015790E-16, 159.6692148526084907 ) ) ;
#14941 = CARTESIAN_POINT ( 'NONE',  ( 15.00000000000000178, -3.464101615137757051, -0.4124999999999987566 ) ) ;
#14942 = LINE ( 'NONE', #709, #24810 ) ;
#14943 = CARTESIAN_POINT ( 'NONE',  ( 37.28548217858939040, -3.604726614523238837, 164.5069853552165284 ) ) ;
#14944 = CARTESIAN_POINT ( 'NONE',  ( 33.91126540609537443, -5.196152422706635576, 163.1552991495023548 ) ) ;
#14945 = CARTESIAN_POINT ( 'NONE',  ( 27.00000000000001421, 196.5875000000000341, 15.58845726811988897 ) ) ;
#14946 = CARTESIAN_POINT ( 'NONE',  ( 15.00000000000000000, 248.2000000000000171, 0.000000000000000000 ) ) ;
#14947 = CARTESIAN_POINT ( 'NONE',  ( 13.62178482187501416, 196.3531250006145115, 23.59362340125806767 ) ) ;
#14948 = CARTESIAN_POINT ( 'NONE',  ( 11.61527771782809637, 103.6648137178985678, 4.622313124798827388 ) ) ;
#14949 = CARTESIAN_POINT ( 'NONE',  ( -11.48171059495397373, 114.4851862821014521, -4.944772684328680334 ) ) ;
#14951 = ORIENTED_EDGE ( 'NONE', *, *, #19014, .F. ) ;
#14950 = VERTEX_POINT ( 'NONE', #25794 ) ;
#14952 = B_SPLINE_CURVE_WITH_KNOTS ( 'NONE', 1,
 ( #32132, #6171 ),
 .UNSPECIFIED., .F., .F.,
 ( 2, 2 ),
 ( 0.000000000000000000, 1.000000000000000000 ),
 .UNSPECIFIED. ) ;
#14953 = CARTESIAN_POINT ( 'NONE',  ( -27.24356964375000345, 196.6531250006145513, 0.000000000000000000 ) ) ;
#14954 = CARTESIAN_POINT ( 'NONE',  ( 33.93414378867374381, 5.196152422706631135, 163.4168002589758260 ) ) ;
#14955 = VECTOR ( 'NONE', #3157, 1000.000000000000000 ) ;
#14956 = EDGE_CURVE ( 'NONE', #30367, #13498, #37343, .T. ) ;
#14957 = CARTESIAN_POINT ( 'NONE',  ( -5.770363421894122880, 78.36481371789855643, 14.38691631536194393 ) ) ;
#14958 = CARTESIAN_POINT ( 'NONE',  ( 23.87821517812500005, -4.985214923628404016, -4.603124999385476812 ) ) ;
#14959 = CARTESIAN_POINT ( 'NONE',  ( 23.87821517812499650, 247.4593750006145285, -4.985214923628404904 ) ) ;
#14960 = CARTESIAN_POINT ( 'NONE',  ( 8.710071997420127943, 100.6851862821014834, 3.796722387233375073 ) ) ;
#14961 = CARTESIAN_POINT ( 'NONE',  ( 27.00000000000000355, 195.3875000012290286, -3.306546357697854128E-15 ) ) ;
#14962 = CARTESIAN_POINT ( 'NONE',  ( -9.534712964251895073, 80.37731371789853085, -1.715153634034446428 ) ) ;
#14963 = CARTESIAN_POINT ( 'NONE',  ( 10.31873187879411269, 3.604726614523236616, -4.678124999385532945 ) ) ;
#14964 = CARTESIAN_POINT ( 'NONE',  ( 18.12178482187500350, 241.2718750006145001, 4.985214923628407568 ) ) ;
#14965 = CARTESIAN_POINT ( 'NONE',  ( 11.61527771782809637, 48.46481371789855785, 4.622313124798827388 ) ) ;
#14966 = CARTESIAN_POINT ( 'NONE',  ( 20.99999999999999645, -6.928203230275506996, -3.037500000000010747 ) ) ;
#14967 = CARTESIAN_POINT ( 'NONE',  ( 12.50000000000000355, 100.1101862821014521, 0.1745138560725507937 ) ) ;
#14968 = CARTESIAN_POINT ( 'NONE',  ( 22.56230152254410370, 3.464101615137755275, -5.024999998771013665 ) ) ;
#14969 = CARTESIAN_POINT ( 'NONE',  ( -32.58705436395489841, 205.3262412349647263, -4.842901733360204020 ) ) ;
#14970 = CARTESIAN_POINT ( 'NONE',  ( 0.000000000000000000, 210.0000000000000284, 0.000000000000000000 ) ) ;
#14971 = DIRECTION ( 'NONE',  ( 0.000000000000000000, -1.000000000000000000, 0.000000000000000000 ) ) ;
#14972 = CARTESIAN_POINT ( 'NONE',  ( -14.25334919248782306, 77.68518628210145494, -6.092822981423979378 ) ) ;
#14973 = AXIS2_PLACEMENT_3D ( 'NONE', #7839, #25266, #4609 ) ;
#14974 = CARTESIAN_POINT ( 'NONE',  ( -4.622313124798576922, 5.235186282101428112, -11.61527771782819762 ) ) ;
#14975 = CARTESIAN_POINT ( 'NONE',  ( -26.99999999999999645, 199.1375000000000171, 15.58845726811991561 ) ) ;
#14976 = CARTESIAN_POINT ( 'NONE',  ( 3.474262827703335166, 111.0351862821014635, 8.843639120294326972 ) ) ;
#14977 = FACE_OUTER_BOUND ( 'NONE', #28481, .T. ) ;
#14978 = CARTESIAN_POINT ( 'NONE',  ( -15.46528703574804986, 12.99768628210143362, -3.257655550457287497 ) ) ;
#14979 = CARTESIAN_POINT ( 'NONE',  ( -27.24356964374999990, 195.3218750006145399, -15.72908226750537786 ) ) ;
#14980 = CARTESIAN_POINT ( 'NONE',  ( 18.12178482187500350, 241.2718750006145001, 4.985214923628407568 ) ) ;
#14981 = ORIENTED_EDGE ( 'NONE', *, *, #20298, .T. ) ;
#14982 = CARTESIAN_POINT ( 'NONE',  ( 31.12286715849720764, 7.209453229046475009, 165.7049010755369807 ) ) ;
#14983 = DIRECTION ( 'NONE',  ( 1.000000000000000000, 0.000000000000000000, 0.000000000000000000 ) ) ;
#14984 = CARTESIAN_POINT ( 'NONE',  ( 19.56230152254411081, -5.196152422706629359, -5.137499998771027698 ) ) ;
#14985 = CYLINDRICAL_SURFACE ( 'NONE', #21550, 2.649999999999991029 ) ;
#14986 = PLANE ( 'NONE',  #2153 ) ;
#14987 = CARTESIAN_POINT ( 'NONE',  ( 14.99999999999999822, 204.0000000000000284, 3.514718625761426019 ) ) ;
#14988 = CARTESIAN_POINT ( 'NONE',  ( 16.56230152254411081, 7.209453229046475009, -0.7031249993855005487 ) ) ;
#14989 = CARTESIAN_POINT ( 'NONE',  ( 8.152565276336593669, 11.95231371789853902, 5.233372021372610483 ) ) ;
#14990 = CARTESIAN_POINT ( 'NONE',  ( 28.99999999999999645, 210.0000000000000284, 0.000000000000000000 ) ) ;
#14991 = ORIENTED_EDGE ( 'NONE', *, *, #11549, .F. ) ;
#14992 = CARTESIAN_POINT ( 'NONE',  ( 21.00000000000000000, 239.8187500012290343, 6.928203230275506996 ) ) ;
#14993 = CARTESIAN_POINT ( 'NONE',  ( 8.962234695871567070, 49.03981371789854649, 8.715434833792127023 ) ) ;
#14994 = CARTESIAN_POINT ( 'NONE',  ( 23.87821517812499650, 4.985214923628404904, -1.190624999385464511 ) ) ;
#14995 = CARTESIAN_POINT ( 'NONE',  ( -7.228626920338836470, 7.927313717898537782, -10.49813415416005213 ) ) ;
#14996 = DIRECTION ( 'NONE',  ( 4.130293990420971855E-17, -1.000000000000000000, 0.000000000000000000 ) ) ;
#14997 = ORIENTED_EDGE ( 'NONE', *, *, #16436, .F. ) ;
#14998 = CARTESIAN_POINT ( 'NONE',  ( 16.56230152254411436, 7.209453229046482114, -2.559374999385494842 ) ) ;
#14999 = ORIENTED_EDGE ( 'NONE', *, *, #22340, .T. ) ;
#15000 = CARTESIAN_POINT ( 'NONE',  ( -27.24356964374999990, 197.9656250006145228, -15.72908226750537786 ) ) ;
#15001 = CARTESIAN_POINT ( 'NONE',  ( 33.98928129033111389, 5.407089921784862696, 162.6497006628943041 ) ) ;
#15002 = EDGE_CURVE ( 'NONE', #2711, #32139, #31485, .T. ) ;
#15003 = CARTESIAN_POINT ( 'NONE',  ( -30.20461230271182274, 208.1428034533959135, -6.469044688360754414 ) ) ;
#15004 = VECTOR ( 'NONE', #36234, 1000.000000000000000 ) ;
#15005 = CARTESIAN_POINT ( 'NONE',  ( 15.24356964375000167, 248.8843750006145399, 3.323476615752272600 ) ) ;
#15006 = CARTESIAN_POINT ( 'NONE',  ( -27.08961370327137175, 194.9999999999998863, -0.9223232689292477637 ) ) ;
#15007 = CARTESIAN_POINT ( 'NONE',  ( -58.50669563604516554, 209.8844732041982297, -4.499999999999996447 ) ) ;
#15008 = CARTESIAN_POINT ( 'NONE',  ( -36.14955436395490551, 214.8429017333601792, -4.673758765035196383 ) ) ;
#15009 = CARTESIAN_POINT ( 'NONE',  ( 37.40804494182826545, -3.604726614523235284, 165.9078841494080336 ) ) ;
#15010 = EDGE_LOOP ( 'NONE', ( #36665, #103, #7453, #27382, #26530, #9981, #19537, #1412, #7684, #15844, #34846, #36276, #29753, #7312, #31878, #25900, #41, #4592, #31725, #32352, #3727, #348, #27010, #8520, #15191, #6060, #17511, #36617, #37083, #20214, #25245, #22986, #10839, #16828, #11405, #3475, #34657, #19796, #28783 ) ) ;
#15011 = CARTESIAN_POINT ( 'NONE',  ( 24.00000000000000000, 241.6562500012290400, 5.196152422706629359 ) ) ;
#15012 = CARTESIAN_POINT ( 'NONE',  ( 13.23911966647199812, 11.95231371789853902, 8.632099005475788900 ) ) ;
#15013 = CARTESIAN_POINT ( 'NONE',  ( -62.07663769728824121, 202.5810206699313767, 4.149950860017909804 ) ) ;
#15014 = PRODUCT_DEFINITION_SHAPE ( 'NONE', 'NONE',  #6956 ) ;
#15015 = CARTESIAN_POINT ( 'NONE',  ( -5.233372021372430183, 133.7476862821013981, -8.152565276336710909 ) ) ;
#15016 = EDGE_CURVE ( 'NONE', #590, #33506, #19476, .T. ) ;
#15017 = CARTESIAN_POINT ( 'NONE',  ( -4.622313124798576922, 32.83518628210143930, -11.61527771782819762 ) ) ;
#15018 = EDGE_CURVE ( 'NONE', #15581, #28127, #37362, .T. ) ;
#15019 = CARTESIAN_POINT ( 'NONE',  ( 13.56230152254410548, 5.196152422706636465, -7.725000000000036948 ) ) ;
#15020 = EDGE_LOOP ( 'NONE', ( #33041, #612, #26784, #7733, #30242 ) ) ;
#15021 = PRESENTATION_STYLE_ASSIGNMENT (( #15591 ) ) ;
#15022 = CARTESIAN_POINT ( 'NONE',  ( -15.53471296425195369, 122.8226862821014294, 2.908627838312118019 ) ) ;
#15023 = CARTESIAN_POINT ( 'NONE',  ( -49.64999999999999858, 244.5000000000000000, -0.4999999999999973910 ) ) ;
#15024 = CARTESIAN_POINT ( 'NONE',  ( -8.710071997420127943, 4.085186282101443744, -3.796722387233380402 ) ) ;
#15025 = CARTESIAN_POINT ( 'NONE',  ( -13.62178482187498396, 194.9843750006145626, 23.59362340125808188 ) ) ;
#15026 = CARTESIAN_POINT ( 'NONE',  ( -1.045839947578415010E-13, 195.7250000012290343, 27.00000000000000355 ) ) ;
#15027 = CARTESIAN_POINT ( 'NONE',  ( 20.99999999999999645, 185.0294372515228645, -5.999999999999999112 ) ) ;
#15028 = CARTESIAN_POINT ( 'NONE',  ( 20.99999999999999289, 243.1937500012290343, -5.999999999999997335 ) ) ;
#15029 = DIRECTION ( 'NONE',  ( 1.000000000000000000, 0.000000000000000000, 0.000000000000000000 ) ) ;
#15030 = EDGE_CURVE ( 'NONE', #35488, #3383, #14143, .T. ) ;
#15031 = CARTESIAN_POINT ( 'NONE',  ( 21.00000000000000000, 243.2218750006145456, 6.646953231504538984 ) ) ;
#15032 = CARTESIAN_POINT ( 'NONE',  ( 9.500000000000005329, 84.68981371789855928, -0.1745138560723090149 ) ) ;
#15033 = CARTESIAN_POINT ( 'NONE',  ( -95.81998461310567450, 11.77610610744882358, -3.000000000000000000 ) ) ;
#15034 = VECTOR ( 'NONE', #35027, 1000.000000000000000 ) ;
#15035 = ORIENTED_EDGE ( 'NONE', *, *, #32395, .F. ) ;
#15036 = CARTESIAN_POINT ( 'NONE',  ( -51.38913769728823411, 206.8500491399821044, -5.686928522499717253 ) ) ;
#15037 = CARTESIAN_POINT ( 'NONE',  ( 21.00000000000000000, 246.3437500012290684, -6.928203230275506996 ) ) ;
#15038 = CARTESIAN_POINT ( 'NONE',  ( 2.311890736173452421, 91.87731371789855928, -12.53471296425189152 ) ) ;
#15039 = CARTESIAN_POINT ( 'NONE',  ( 13.44051670066911086, 5.407089921784862696, -1.621874999385541916 ) ) ;
#15040 = CARTESIAN_POINT ( 'NONE',  ( 24.44548853280170775, -3.604726614523240613, 161.0190418602530258 ) ) ;
#15041 = CARTESIAN_POINT ( 'NONE',  ( 23.87821517812499650, 4.985214923628404904, -1.753124999385485827 ) ) ;
#15042 = CARTESIAN_POINT ( 'NONE',  ( 11.48171059495408208, 74.91481371789855359, -4.944772684328420986 ) ) ;
#15043 = CARTESIAN_POINT ( 'NONE',  ( -1.926257025242585782E-15, 198.8468750006145740, -31.45816453501075927 ) ) ;
#15044 = ORIENTED_EDGE ( 'NONE', *, *, #2979, .F. ) ;
#15045 = ORIENTED_EDGE ( 'NONE', *, *, #13178, .F. ) ;
#15046 = CARTESIAN_POINT ( 'NONE',  ( 26.75643035624999655, -3.323476615752267271, -4.453124999385455141 ) ) ;
#15047 = CARTESIAN_POINT ( 'NONE',  ( 16.56230152254410726, 0.000000000000000000, -10.00000000000000000 ) ) ;
#15048 = CARTESIAN_POINT ( 'NONE',  ( 15.24356964375000167, 245.7343750006145058, 3.323476615752272600 ) ) ;
#15049 = CARTESIAN_POINT ( 'NONE',  ( 7.228626920339068285, 34.27268628210144641, -10.49813415415989581 ) ) ;
#15050 = CARTESIAN_POINT ( 'NONE',  ( -45.04836230271183695, 204.3130714775002446, -3.149950860017828091 ) ) ;
#15051 = CARTESIAN_POINT ( 'NONE',  ( 16.22935424640156654, 222.7217220095854202, -3.659938751165931148 ) ) ;
#15052 = AXIS2_PLACEMENT_3D ( 'NONE', #27609, #1641, #24762 ) ;
#15053 = CARTESIAN_POINT ( 'NONE',  ( -34.95461230271183695, 208.6787018382582346, -4.469044688360757966 ) ) ;
#15054 = CARTESIAN_POINT ( 'NONE',  ( 36.68413903717728175, 3.464101615137755275, 160.4282500447066866 ) ) ;
#15055 = CARTESIAN_POINT ( 'NONE',  ( -11.61527771782809282, 80.66481371789856780, -4.622313124798832717 ) ) ;
#15056 = CARTESIAN_POINT ( 'NONE',  ( -61.08705436395490551, 206.7903428501026042, -3.378800118222489157 ) ) ;
#15057 = EDGE_CURVE ( 'NONE', #15757, #8199, #3043, .T. ) ;
#15058 = CARTESIAN_POINT ( 'NONE',  ( -33.97247103062156270, 205.6499508600178956, 7.303452534266880569 ) ) ;
#15059 = CARTESIAN_POINT ( 'NONE',  ( 20.99999999999999645, 6.646953231504538984, -7.565624999385492266 ) ) ;
#15060 = CARTESIAN_POINT ( 'NONE',  ( 24.98477879236699195, 0.000000000000000000, 49.65137702900941008 ) ) ;
#15061 = CARTESIAN_POINT ( 'NONE',  ( -8.927990412390371944, 81.52731371789856496, -13.04141134922778988 ) ) ;
#15062 = CARTESIAN_POINT ( 'NONE',  ( -55.53794563604517975, 203.8621396198271043, 6.307003348498029460 ) ) ;
#15063 = CARTESIAN_POINT ( 'NONE',  ( 14.99999999999972466, -3.464101615137598067, -0.8062499987709568217 ) ) ;
#15064 = CARTESIAN_POINT ( 'NONE',  ( 8.715434833791931624, 92.06018628210145494, 8.962234695871760692 ) ) ;
#15065 = ADVANCED_FACE ( 'NONE', ( #17093 ), #14613, .F. ) ;
#15066 = CARTESIAN_POINT ( 'NONE',  ( 3.257655550457285720, 42.89768628210143220, -15.46528703574804986 ) ) ;
#15067 = CARTESIAN_POINT ( 'NONE',  ( 24.39809759768267128, 0.000000000000000000, 160.4773609931656608 ) ) ;
#15068 = CARTESIAN_POINT ( 'NONE',  ( 11.08355503943142750, 52.96018628210144641, -10.83675517735155225 ) ) ;
#15069 = CARTESIAN_POINT ( 'NONE',  ( -1.926257025242585782E-15, 199.2406250006145285, -31.45816453501076637 ) ) ;
#15070 = CARTESIAN_POINT ( 'NONE',  ( 22.80587116629410716, 3.604726614523238837, -7.978124999385491023 ) ) ;
#15071 = DIRECTION ( 'NONE',  ( -0.000000000000000000, 1.000000000000000000, -0.000000000000000000 ) ) ;
#15072 = CARTESIAN_POINT ( 'NONE',  ( -48.22247103062156270, 206.6499508600178672, 5.571401726697986057 ) ) ;
#15073 = CARTESIAN_POINT ( 'NONE',  ( 26.99999999999999645, 241.2437500012290457, 3.464101615137751278 ) ) ;
#15074 = CARTESIAN_POINT ( 'NONE',  ( -12.46528703574805697, 31.39768628210144641, -2.660918448318280838 ) ) ;
#15075 = CARTESIAN_POINT ( 'NONE',  ( 15.00000000000000000, 240.0999999999999943, 0.000000000000000000 ) ) ;
#15076 = CARTESIAN_POINT ( 'NONE',  ( -3.474262827703527901, 142.7648137178985621, 8.843639120294245259 ) ) ;
#15077 = CARTESIAN_POINT ( 'NONE',  ( 26.75643035624999655, 246.5218750006145285, -3.323476615752271268 ) ) ;
#15078 = VERTEX_POINT ( 'NONE', #26350 ) ;
#15079 = CARTESIAN_POINT ( 'NONE',  ( 15.00000000000000000, 3.464101615137752166, -8.137499999999985079 ) ) ;
#15080 = CARTESIAN_POINT ( 'NONE',  ( 26.99999999999999645, 7.347880794884117764E-16, -4.275000000000001243 ) ) ;
#15081 = CARTESIAN_POINT ( 'NONE',  ( 19.56230152254411792, -5.196152422706629359, -3.337499998771031873 ) ) ;
#15082 = CARTESIAN_POINT ( 'NONE',  ( 16.56230152254411081, -7.209453229046475009, -5.428124999385503635 ) ) ;
#15083 = CARTESIAN_POINT ( 'NONE',  ( 37.48648511030114605, -3.604726614523235284, 166.8044593776906197 ) ) ;
#15084 = CARTESIAN_POINT ( 'NONE',  ( 23.99999999999999645, 240.8500000000000227, -5.196152422706631135 ) ) ;
#15085 = CARTESIAN_POINT ( 'NONE',  ( 30.63506736085999904, 6.928203230275506996, 160.1293238752668913 ) ) ;
#15086 = CARTESIAN_POINT ( 'NONE',  ( 10.49813415415989581, 54.97268628210144925, 7.228626920339069173 ) ) ;
#15087 = ORIENTED_EDGE ( 'NONE', *, *, #22356, .F. ) ;
#15088 = EDGE_LOOP ( 'NONE', ( #21443, #20726, #24143 ) ) ;
#15089 = CARTESIAN_POINT ( 'NONE',  ( 36.94560626531313829, 7.347880794884125653E-16, 163.4168341377576041 ) ) ;
#15090 = CARTESIAN_POINT ( 'NONE',  ( 18.00000000000000000, 243.6250000000000000, -5.196152422706630247 ) ) ;
#15091 = CARTESIAN_POINT ( 'NONE',  ( 24.59253236524820352, -3.464101615137419543, 159.9051123081840444 ) ) ;
#15092 =( BOUNDED_CURVE ( )  B_SPLINE_CURVE ( 2, ( #13209, #10171, #10358, #4479, #1638, #19288, #30827 ),
 .UNSPECIFIED., .F., .F. ) 
 B_SPLINE_CURVE_WITH_KNOTS ( ( 3, 2, 2, 3 ),
 ( 0.1956521739130429038, 0.2028985507246371944, 0.2101449275362314850, 0.2173913043478257756 ),
 .UNSPECIFIED. ) 
 CURVE ( )  GEOMETRIC_REPRESENTATION_ITEM ( )  RATIONAL_B_SPLINE_CURVE ( ( 1.000000000000010658, 0.8660254037844279384, 1.000000000000000000, 0.8660254037844387076, 1.000000000000000000, 0.8660254037844443697, 0.9999999999999943379 ) ) 
 REPRESENTATION_ITEM ( '' )  );
#15093 = CARTESIAN_POINT ( 'NONE',  ( 30.76253263452132813, -6.928203230275514990, 161.5862586200017574 ) ) ;
#15094 = CARTESIAN_POINT ( 'NONE',  ( 15.24356964375000167, -3.323476615752272600, -7.303124999385448568 ) ) ;
#15095 = CARTESIAN_POINT ( 'NONE',  ( -2.660918448318275509, 102.6976862821014720, 12.46528703574805874 ) ) ;
#15096 = CARTESIAN_POINT ( 'NONE',  ( -8.927990412390371944, 26.32731371789854791, -13.04141134922778988 ) ) ;
#15097 = CARTESIAN_POINT ( 'NONE',  ( 26.99999999999962341, -3.464101615137965773, -5.156249998770960019 ) ) ;
#15098 = CARTESIAN_POINT ( 'NONE',  ( 18.12178482187499640, 239.8843750006145115, -4.985214923628404904 ) ) ;
#15099 = CARTESIAN_POINT ( 'NONE',  ( -36.14955436395489841, 213.3788001182225003, -3.209657149897400252 ) ) ;
#15100 = CARTESIAN_POINT ( 'NONE',  ( -5.043980924894071016, 224.5060857195767596, 2.499999999999999112 ) ) ;
#15101 = CARTESIAN_POINT ( 'NONE',  ( 36.86059793269458140, 3.604726614523243278, 159.6505362020193104 ) ) ;
#15102 = CARTESIAN_POINT ( 'NONE',  ( 10.49813415416005213, 139.0273137178985507, -7.228626920338837358 ) ) ;
#15103 = CARTESIAN_POINT ( 'NONE',  ( -56.13913769728823411, 206.8500491399821044, -5.686928522499717253 ) ) ;
#15104 = CARTESIAN_POINT ( 'NONE',  ( -66.23288769728823411, 201.5309553116392181, -2.393094931466246855 ) ) ;
#15105 = DIRECTION ( 'NONE',  ( 0.000000000000000000, 0.000000000000000000, 1.000000000000000000 ) ) ;
#15106 = CARTESIAN_POINT ( 'NONE',  ( 15.00000000000000000, 240.9625000000000057, -3.464101615137752610 ) ) ;
#15107 = CARTESIAN_POINT ( 'NONE',  ( -27.24356964374999635, 198.9406250006145171, 15.72908226750539384 ) ) ;
#15108 = CARTESIAN_POINT ( 'NONE',  ( -15.46528703574811736, 135.0023137178985166, 3.257655550456946436 ) ) ;
#15109 = CARTESIAN_POINT ( 'NONE',  ( -62.26711230271183695, 216.4690446883607535, -1.857196546604089393 ) ) ;
#15110 = ORIENTED_EDGE ( 'NONE', *, *, #9600, .F. ) ;
#15111 = CARTESIAN_POINT ( 'NONE',  ( -10.69584247140444866, 48.64768628210144641, 6.932735513423972762 ) ) ;
#15112 = CARTESIAN_POINT ( 'NONE',  ( -5.732297079746171420, 222.9518338469886203, -2.500000000000000000 ) ) ;
#15113 = CARTESIAN_POINT ( 'NONE',  ( 22.56230152254411792, 7.347880794884125653E-16, -9.675000000000045119 ) ) ;
#15114 = CARTESIAN_POINT ( 'NONE',  ( 31.27484498491342180, 7.209453229046482114, 167.4420155803344699 ) ) ;
#15115 = CARTESIAN_POINT ( 'NONE',  ( -6.092822981423970496, 102.9851862821014805, 14.25334919248782661 ) ) ;
#15116 = CARTESIAN_POINT ( 'NONE',  ( -66.82663769728823411, 204.3130714775002730, 3.149950860017883603 ) ) ;
#15117 = CARTESIAN_POINT ( 'NONE',  ( 13.44051670066911619, -5.407089921784859143, -1.415624999385550753 ) ) ;
#15118 = CARTESIAN_POINT ( 'NONE',  ( 8.152565276336714462, 62.44768628210144357, -5.233372021372432847 ) ) ;
#15119 = DIRECTION ( 'NONE',  ( 1.659705900203722642E-32, -2.710505431213758127E-16, -1.000000000000000000 ) ) ;
#15120 = CARTESIAN_POINT ( 'NONE',  ( 22.60769515458671108, 244.7325961894323143, 6.000000000000010658 ) ) ;
#15121 = CARTESIAN_POINT ( 'NONE',  ( -8.962234695871760692, 94.36018628210145209, 8.715434833791933400 ) ) ;
#15122 = FACE_OUTER_BOUND ( 'NONE', #34200, .T. ) ;
#15123 = CARTESIAN_POINT ( 'NONE',  ( 26.99999999999999645, 198.5750000012290570, -15.58845726811990495 ) ) ;
#15124 = CARTESIAN_POINT ( 'NONE',  ( -79.65000000000001990, 210.0000000000000000, -3.000000000000000000 ) ) ;
#15125 = CARTESIAN_POINT ( 'NONE',  ( 30.67183618977810156, -7.209453229046475009, 160.5495935129122245 ) ) ;
#15126 = CARTESIAN_POINT ( 'NONE',  ( 26.99999999999999645, 7.347880794884117764E-16, -0.2250000000000029754 ) ) ;
#15127 = VECTOR ( 'NONE', #36050, 1000.000000000000000 ) ;
#15128 = CARTESIAN_POINT ( 'NONE',  ( -29.50000000000000711, 237.0000000000000000, -2.499999999999994671 ) ) ;
#15129 = CARTESIAN_POINT ( 'NONE',  ( 34.09386818162830224, -5.407089921784861808, 163.8451343006043999 ) ) ;
#15130 = CARTESIAN_POINT ( 'NONE',  ( 33.87204532185894124, -5.196152422706635576, 162.7070115353610618 ) ) ;
#15131 = CARTESIAN_POINT ( 'NONE',  ( 26.99999999999999645, 248.3875000000000171, 3.464101615137751278 ) ) ;
#15132 = CARTESIAN_POINT ( 'NONE',  ( 13.62178482187499640, 196.9531250006145342, -23.59362340125807123 ) ) ;
#15133 = CARTESIAN_POINT ( 'NONE',  ( -10.69584247140429412, 108.5523137178985564, -6.932735513424201024 ) ) ;
#15134 = CARTESIAN_POINT ( 'NONE',  ( 2.311890736173175753, 111.3226862821014578, 12.53471296425194659 ) ) ;
#15135 = EDGE_LOOP ( 'NONE', ( #2067, #9504, #28736, #24048 ) ) ;
#15136 = CARTESIAN_POINT ( 'NONE',  ( -1.926257025242585782E-15, 195.1906250006145456, -31.45816453501075927 ) ) ;
#15137 = CARTESIAN_POINT ( 'NONE',  ( 15.24356964374999990, 240.2968750006145342, 0.000000000000000000 ) ) ;
#15138 = CARTESIAN_POINT ( 'NONE',  ( -11.08355503943118592, 72.03981371789855359, -10.83675517735179383 ) ) ;
#15139 =( BOUNDED_CURVE ( )  B_SPLINE_CURVE ( 2, ( #22042, #27899, #1929, #18033, #11769, #37345, #2855 ),
 .UNSPECIFIED., .F., .F. ) 
 B_SPLINE_CURVE_WITH_KNOTS ( ( 3, 2, 2, 3 ),
 ( 0.3260869565217382471, 0.3333333333333325932, 0.3405797101449269948, 0.3478260869565213409 ),
 .UNSPECIFIED. ) 
 CURVE ( )  GEOMETRIC_REPRESENTATION_ITEM ( )  RATIONAL_B_SPLINE_CURVE ( ( 1.000000000000016431, 0.8660254037844222763, 1.000000000000000000, 0.8660254037844387076, 1.000000000000000000, 0.8660254037844459241, 0.9999999999999927836 ) ) 
 REPRESENTATION_ITEM ( '' )  );
#15140 = ADVANCED_FACE ( 'NONE', ( #25610 ), #34328, .T. ) ;
#15141 = CARTESIAN_POINT ( 'NONE',  ( 15.24356964374999990, 3.323476615752268604, -4.790624999385491023 ) ) ;
#15142 = CARTESIAN_POINT ( 'NONE',  ( 18.12178482187500350, 247.2343750006145342, 4.985214923628407568 ) ) ;
#15143 = AXIS2_PLACEMENT_3D ( 'NONE', #3690, #464, #12032 ) ;
#15144 = CARTESIAN_POINT ( 'NONE',  ( -6.840914352312096547, 103.5601862821014407, 6.594114490232313663 ) ) ;
#15145 = CARTESIAN_POINT ( 'NONE',  ( 26.99999999999999645, 7.347880794884117764E-16, -6.468749998770951137 ) ) ;
#15146 = CARTESIAN_POINT ( 'NONE',  ( -8.152565276336593669, 71.75231371789854506, -5.233372021372610483 ) ) ;
#15147 = CARTESIAN_POINT ( 'NONE',  ( 19.68408634441910721, -5.407089921784855591, -4.490624999385572913 ) ) ;
#15148 = CARTESIAN_POINT ( 'NONE',  ( -5.233372021372612259, 115.4523137178985479, 8.152565276336593669 ) ) ;
#15149 = CARTESIAN_POINT ( 'NONE',  ( 26.75643035624999655, 241.4218750006145058, -7.049594010296217766E-16 ) ) ;
#15150 = CARTESIAN_POINT ( 'NONE',  ( -12.46528703574811558, 52.20231371789855501, 2.660918448318003726 ) ) ;
#15151 = FACE_OUTER_BOUND ( 'NONE', #579, .T. ) ;
#15152 = CARTESIAN_POINT ( 'NONE',  ( 12.53471296425194836, 99.82268628210144357, -2.311890736173178418 ) ) ;
#15153 = CARTESIAN_POINT ( 'NONE',  ( 13.56230152254410548, 5.196152422706630247, -6.262499998771015264 ) ) ;
#15154 = EDGE_CURVE ( 'NONE', #18985, #3075, #13943, .T. ) ;
#15155 =( BOUNDED_CURVE ( )  B_SPLINE_CURVE ( 2, ( #1287, #30109, #35974, #10011, #15523, #12671, #35218 ),
 .UNSPECIFIED., .F., .F. ) 
 B_SPLINE_CURVE_WITH_KNOTS ( ( 3, 2, 2, 3 ),
 ( 0.8478260869565249491, 0.8550724637681192952, 0.8623188405797136413, 0.8695652173913078764 ),
 .UNSPECIFIED. ) 
 CURVE ( )  GEOMETRIC_REPRESENTATION_ITEM ( )  RATIONAL_B_SPLINE_CURVE ( ( 0.9999999999999404920, 0.8660254037844982156, 1.000000000000000000, 0.8660254037844387076, 1.000000000000000000, 0.8660254037843729824, 1.000000000000065725 ) ) 
 REPRESENTATION_ITEM ( '' )  );
#15156 = CARTESIAN_POINT ( 'NONE',  ( -65.24330436395489130, 210.1155267958017703, -4.499999999999996447 ) ) ;
#15157 = CARTESIAN_POINT ( 'NONE',  ( 12.53471296425194836, 136.6226862821014834, -2.311890736173178418 ) ) ;
#15158 = CARTESIAN_POINT ( 'NONE',  ( 34.19028422204287665, 5.407089921784857367, 164.9471746853683669 ) ) ;
#15159 = CARTESIAN_POINT ( 'NONE',  ( 14.38691631536207538, 90.33518628210144641, -5.770363421893813793 ) ) ;
#15160 = CARTESIAN_POINT ( 'NONE',  ( 22.80587116629411781, 7.646167579472024665E-16, -4.921874999385511984 ) ) ;
#15161 = CARTESIAN_POINT ( 'NONE',  ( 22.60769515458672885, 248.5174038105676004, -6.000000000000000000 ) ) ;
#15162 = DIRECTION ( 'NONE',  ( 1.000000000000000000, 0.000000000000000000, -0.000000000000000000 ) ) ;
#15163 = CARTESIAN_POINT ( 'NONE',  ( 26.99999999999999645, 198.4625000000000057, -15.58845726811990495 ) ) ;
#15164 = CARTESIAN_POINT ( 'NONE',  ( -8.152565276336710909, 122.2476862821014691, 5.233372021372435512 ) ) ;
#15165 = CARTESIAN_POINT ( 'NONE',  ( 21.00000000000000000, 249.4375000000000568, -5.999999999999998224 ) ) ;
#15166 = EDGE_CURVE ( 'NONE', #24000, #27477, #29855, .T. ) ;
#15167 = CARTESIAN_POINT ( 'NONE',  ( 3.257655550457285720, 6.097686282101443922, -15.46528703574804986 ) ) ;
#15168 = CARTESIAN_POINT ( 'NONE',  ( 27.24356964374999635, 196.0718750006145683, -15.72908226750539029 ) ) ;
#15169 = CARTESIAN_POINT ( 'NONE',  ( 23.87821517812499650, 241.0468750006145058, -4.985214923628404904 ) ) ;
#15171 = ORIENTED_EDGE ( 'NONE', *, *, #30732, .T. ) ;
#15170 = VECTOR ( 'NONE', #6253, 1000.000000000000000 ) ;
#15172 = CARTESIAN_POINT ( 'NONE',  ( 28.05545009495152087, 5.407089921784856479, 166.4626274657055660 ) ) ;
#15173 = CARTESIAN_POINT ( 'NONE',  ( 26.75643035624999655, 3.323476615752271712, -3.478124999385468819 ) ) ;
#15174 = CARTESIAN_POINT ( 'NONE',  ( 10.56230152254485155, -3.464101615138189594, -4.912500000000042277 ) ) ;
#15175 = PLANE ( 'NONE',  #16701 ) ;
#15176 = CARTESIAN_POINT ( 'NONE',  ( 13.56230152254410548, 5.196152422706630247, -5.812499998771008869 ) ) ;
#15177 = CARTESIAN_POINT ( 'NONE',  ( 37.06326651802246630, 7.347880794884125653E-16, 164.7616969801814548 ) ) ;
#15178 = CARTESIAN_POINT ( 'NONE',  ( 7.234628195640309123, 198.9674038105676743, -27.00000000000000711 ) ) ;
#15179 = CARTESIAN_POINT ( 'NONE',  ( -2.064181346179062349, 26.90231371789854364, -9.465287035748106703 ) ) ;
#15180 = CARTESIAN_POINT ( 'NONE',  ( -1.926257025242585782E-15, 197.0468750006145342, -31.45816453501076637 ) ) ;
#15182 = VERTEX_POINT ( 'NONE', #30145 ) ;
#15181 = VERTEX_POINT ( 'NONE', #6830 ) ;
#15183 = CARTESIAN_POINT ( 'NONE',  ( 15.24356964375000167, 247.5343750006144887, 3.323476615752272600 ) ) ;
#15184 = CARTESIAN_POINT ( 'NONE',  ( 12.46528703574811558, 20.00231371789855217, -2.660918448318005947 ) ) ;
#15185 = CARTESIAN_POINT ( 'NONE',  ( 18.12178482187499640, 4.985214923628404904, -1.565624999385478722 ) ) ;
#15186 = CARTESIAN_POINT ( 'NONE',  ( 14.38691631536194393, 131.2648137178985621, 5.770363421894124656 ) ) ;
#15187 = CARTESIAN_POINT ( 'NONE',  ( 26.99999999999999645, 3.464101615137755275, -7.781249998770935150 ) ) ;
#15188 = DIRECTION ( 'NONE',  ( 0.000000000000000000, 0.000000000000000000, -1.000000000000000000 ) ) ;
#15189 = VERTEX_POINT ( 'NONE', #15368 ) ;
#15190 = CARTESIAN_POINT ( 'NONE',  ( 10.31873187879411091, -3.604726614523244610, -3.759374999385526994 ) ) ;
#15191 = ORIENTED_EDGE ( 'NONE', *, *, #2236, .T. ) ;
#15192 = CARTESIAN_POINT ( 'NONE',  ( 13.62178482187501416, 197.7031250006145342, 23.59362340125806767 ) ) ;
#15193 = EDGE_CURVE ( 'NONE', #10170, #15189, #33394, .T. ) ;
#15194 = CARTESIAN_POINT ( 'NONE',  ( 34.17230835010118994, -5.407089921784861808, 164.7417095288869859 ) ) ;
#15195 = AXIS2_PLACEMENT_3D ( 'NONE', #22758, #3397, #37322 ) ;
#15196 = CARTESIAN_POINT ( 'NONE',  ( -63.25669563604515844, 209.8844732041981729, -8.500000000000003553 ) ) ;
#15197 = CARTESIAN_POINT ( 'NONE',  ( 26.75643035624999655, 249.4843750006145058, 3.323476615752267271 ) ) ;
#15198 = CARTESIAN_POINT ( 'NONE',  ( 10.56230152254410903, 0.000000000000000000, -9.787499998771043153 ) ) ;
#15199 = EDGE_CURVE ( 'NONE', #1318, #22836, #36165, .T. ) ;
#15200 = CARTESIAN_POINT ( 'NONE',  ( -40.69419563604516554, 205.4999999999999716, 0.1155267958017633378 ) ) ;
#15201 = CARTESIAN_POINT ( 'NONE',  ( 7.234628195640322446, 196.9825961894323427, 26.99999999999999645 ) ) ;
#15202 = CARTESIAN_POINT ( 'NONE',  ( 37.49302179100721588, 3.604726614523238837, 166.8791739800475113 ) ) ;
#15203 = ORIENTED_EDGE ( 'NONE', *, *, #20272, .F. ) ;
#15204 = CARTESIAN_POINT ( 'NONE',  ( 19.39230484541326049, 248.5575961894323314, -5.999999999999994671 ) ) ;
#15205 = CARTESIAN_POINT ( 'NONE',  ( 8.927990412390657937, 135.4726862821014777, -13.04141134922759804 ) ) ;
#15206 = CARTESIAN_POINT ( 'NONE',  ( -66.43080436395490551, 201.5000000000000000, -0.1155267958017054536 ) ) ;
#15207 = ADVANCED_FACE ( 'NONE', ( #35820 ), #3612, .T. ) ;
#15208 = CARTESIAN_POINT ( 'NONE',  ( 6.840914352312096547, 126.5601862821014834, -6.594114490232313663 ) ) ;
#15209 = PLANE ( 'NONE',  #12707 ) ;
#15210 = CARTESIAN_POINT ( 'NONE',  ( 11.61527771782819940, 25.93518628210143717, -4.622313124798573369 ) ) ;
#15211 = CARTESIAN_POINT ( 'NONE',  ( 16.56230152254411081, 6.928203230275514990, -6.412500000000027178 ) ) ;
#15212 = ORIENTED_EDGE ( 'NONE', *, *, #9163, .T. ) ;
#15213 = CARTESIAN_POINT ( 'NONE',  ( -33.57663769728823411, 204.3130714775002730, 3.149950860017883603 ) ) ;
#15214 = CARTESIAN_POINT ( 'NONE',  ( 5.770363421893814682, 120.2351862821014521, 14.38691631536207183 ) ) ;
#15215 = FILL_AREA_STYLE ('',( #27525 ) ) ;
#15216 = CARTESIAN_POINT ( 'NONE',  ( 5.233372021372432847, 9.547686282101452093, 8.152565276336710909 ) ) ;
#15217 = CARTESIAN_POINT ( 'NONE',  ( -13.62178482187500528, 198.3781250006145171, -23.59362340125807123 ) ) ;
#15218 = DIRECTION ( 'NONE',  ( -0.000000000000000000, 1.000000000000000000, -0.000000000000000000 ) ) ;
#15219 = CARTESIAN_POINT ( 'NONE',  ( 22.56230152254410370, 7.347880794884117764E-16, -1.462499998771016330 ) ) ;
#15220 = CARTESIAN_POINT ( 'NONE',  ( 25.18576762276457259, -3.604726614523244610, 169.4804705771697968 ) ) ;
#15221 = CARTESIAN_POINT ( 'NONE',  ( 24.85073125303116726, 3.464101615137512358, 162.8563391000565161 ) ) ;
#15222 = ADVANCED_FACE ( 'NONE', ( #7035 ), #21067, .T. ) ;
#15223 = CARTESIAN_POINT ( 'NONE',  ( -1.715153634034442431, 78.07731371789854791, 9.534712964251900402 ) ) ;
#15224 = CARTESIAN_POINT ( 'NONE',  ( -4.500000000000000888, 210.0000000000000284, -2.500000000000000000 ) ) ;
#15225 = EDGE_LOOP ( 'NONE', ( #23468, #3355 ) ) ;
#15226 = CARTESIAN_POINT ( 'NONE',  ( 26.99999999999999645, 243.5687500012290343, -3.464101615137755275 ) ) ;
#15227 = CARTESIAN_POINT ( 'NONE',  ( 6.932735513424201024, 101.6523137178985650, -10.69584247140429412 ) ) ;
#15228 = CARTESIAN_POINT ( 'NONE',  ( 10.31873187879410558, 0.000000000000000000, -4.246874999385502392 ) ) ;
#15229 = CARTESIAN_POINT ( 'NONE',  ( 33.79808337967844523, 5.407089921784857367, 160.4642985439555218 ) ) ;
#15230 = CARTESIAN_POINT ( 'NONE',  ( 15.24356964374999990, 0.000000000000000000, -5.653124999385472194 ) ) ;
#15231 = CARTESIAN_POINT ( 'NONE',  ( 10.49813415416005213, 56.22731371789854649, -7.228626920338837358 ) ) ;
#15232 = CARTESIAN_POINT ( 'NONE',  ( 27.24356964375000700, 198.6968750006145115, 15.72908226750537075 ) ) ;
#15233 = ORIENTED_EDGE ( 'NONE', *, *, #25845, .F. ) ;
#15234 = ORIENTED_EDGE ( 'NONE', *, *, #10189, .F. ) ;
#15235 = CARTESIAN_POINT ( 'NONE',  ( 20.99999999999999645, 6.646953231504538984, -5.653124999385485516 ) ) ;
#15236 = CARTESIAN_POINT ( 'NONE',  ( -81.00000000000002842, 214.0000000000000000, 2.500000000000000000 ) ) ;
#15237 = CARTESIAN_POINT ( 'NONE',  ( 23.87821517812500005, 245.3968750006145285, 4.985214923628404016 ) ) ;
#15238 = CARTESIAN_POINT ( 'NONE',  ( 6.932735513423970097, 46.34768628210145636, 10.69584247140445044 ) ) ;
#15239 = EDGE_CURVE ( 'NONE', #22746, #9403, #29760, .T. ) ;
#15240 = CARTESIAN_POINT ( 'NONE',  ( -40.10044563604516554, 205.1570982666397072, -4.673758765035155527 ) ) ;
#15241 = CARTESIAN_POINT ( 'NONE',  ( 16.56230152254411436, 7.209453229046475009, -1.153124999385528371 ) ) ;
#15242 = CARTESIAN_POINT ( 'NONE',  ( -30.79836230271183339, 206.0451222850691977, -2.149950860017851184 ) ) ;
#15243 = FACE_OUTER_BOUND ( 'NONE', #1374, .T. ) ;
#15244 = CARTESIAN_POINT ( 'NONE',  ( 8.962234695871567070, 76.63981371789856212, 8.715434833792127023 ) ) ;
#15245 = CARTESIAN_POINT ( 'NONE',  ( -60.29538769728823411, 211.3212981617418222, -4.469044688360751749 ) ) ;
#15246 = CARTESIAN_POINT ( 'NONE',  ( -34.36830436395490551, 209.8844732041983150, 8.500000000000003553 ) ) ;
#15247 = CARTESIAN_POINT ( 'NONE',  ( 18.12178482187499640, 4.985214923628404904, -7.978124999385494576 ) ) ;
#15248 = CARTESIAN_POINT ( 'NONE',  ( 22.56230152254411792, 7.347880794884125653E-16, -0.6750000000000366818 ) ) ;
#15249 = CARTESIAN_POINT ( 'NONE',  ( 15.50000000000000533, 66.28981371789855359, -0.1745138560722452326 ) ) ;
#15250 = CARTESIAN_POINT ( 'NONE',  ( -57.71502896937850835, 217.3034525342667962, -4.350049139982195001 ) ) ;
#15251 = CIRCLE ( 'NONE', #21917, 24.80000000000000426 ) ;
#15252 = CARTESIAN_POINT ( 'NONE',  ( 2.660918448318279950, 88.89768628210146062, -12.46528703574805697 ) ) ;
#15253 = CARTESIAN_POINT ( 'NONE',  ( 15.53471296425195369, 26.22268628210144925, -2.908627838312120684 ) ) ;
#15254 = CARTESIAN_POINT ( 'NONE',  ( -69.00000000000002842, 210.0000000000000000, 0.000000000000000000 ) ) ;
#15255 = CARTESIAN_POINT ( 'NONE',  ( 27.59297993499679791, -5.407089921784865361, 161.1765693489562352 ) ) ;
#15256 = CARTESIAN_POINT ( 'NONE',  ( 15.53471296425195369, 44.62268628210144783, -2.908627838312120684 ) ) ;
#15257 = CARTESIAN_POINT ( 'NONE',  ( 22.60769515458672885, 247.2236538117966802, -6.000000000000000000 ) ) ;
#15258 = CARTESIAN_POINT ( 'NONE',  ( -27.24356964374999990, 199.8218750006145399, -15.72908226750537786 ) ) ;
#15259 = CARTESIAN_POINT ( 'NONE',  ( 26.99999999999999645, 7.347880794884117764E-16, -1.068749998770962550 ) ) ;
#15260 = CARTESIAN_POINT ( 'NONE',  ( -35.15997103062156270, 215.5714017266979852, 3.350049139982118618 ) ) ;
#15261 = CARTESIAN_POINT ( 'NONE',  ( 13.50000000000001421, 195.6500000000000057, 23.38268590217984055 ) ) ;
#15262 = CARTESIAN_POINT ( 'NONE',  ( -2.311890736173176641, 14.72268628210143859, -12.53471296425194836 ) ) ;
#15263 = CARTESIAN_POINT ( 'NONE',  ( 20.99999999999998579, 247.2437500012290457, -5.999999999999997335 ) ) ;
#15264 = CARTESIAN_POINT ( 'NONE',  ( 6.840914352311949109, 122.6398137178985479, 6.594114490232462877 ) ) ;
#15265 = CARTESIAN_POINT ( 'NONE',  ( 26.75643035624999655, 247.4218750006145626, -3.323476615752271268 ) ) ;
#15266 = ORIENTED_EDGE ( 'NONE', *, *, #36966, .F. ) ;
#15267 = CARTESIAN_POINT ( 'NONE',  ( 21.00000000000000000, 6.928203230275506996, -7.312499999999986677 ) ) ;
#15268 = AXIS2_PLACEMENT_3D ( 'NONE', #20446, #31988, #29134 ) ;
#15269 = CARTESIAN_POINT ( 'NONE',  ( 52.59268362704444399, 124.7349959275252615, -2.500000000000000000 ) ) ;
#15270 = CARTESIAN_POINT ( 'NONE',  ( -4.694659320240884604E-14, 197.4124999999999943, 27.00000000000000000 ) ) ;
#15271 = CARTESIAN_POINT ( 'NONE',  ( 22.80587116629411071, -3.604726614523235284, -7.603124999385552307 ) ) ;
#15272 = CARTESIAN_POINT ( 'NONE',  ( 28.06852345636367119, -5.407089921784859143, 166.6120566704193493 ) ) ;
#15273 = CARTESIAN_POINT ( 'NONE',  ( 19.56230152254411792, -5.196152422706629359, -2.437499998771047949 ) ) ;
#15274 = CARTESIAN_POINT ( 'NONE',  ( -13.50000000000000533, 199.4750000000000227, -23.38268590217984411 ) ) ;
#15275 = CARTESIAN_POINT ( 'NONE',  ( 12.53471296425194659, 53.82268628210145067, -2.311890736173178418 ) ) ;
#15276 = EDGE_LOOP ( 'NONE', ( #32703, #28233, #13322, #36265 ) ) ;
#15277 = ORIENTED_EDGE ( 'NONE', *, *, #34020, .T. ) ;
#15278 = CARTESIAN_POINT ( 'NONE',  ( -6.000000000000000888, -30.00000000000000000, 20.00000000000000711 ) ) ;
#15279 = CARTESIAN_POINT ( 'NONE',  ( 19.56230152254411792, -5.196152422706629359, -1.987499998771014020 ) ) ;
#15280 = LINE ( 'NONE', #35549, #7022 ) ;
#15281 = CARTESIAN_POINT ( 'NONE',  ( 25.22662187717753568, 0.000000000000000000, 169.9474368419002985 ) ) ;
#15282 = CARTESIAN_POINT ( 'NONE',  ( 21.00000000000000000, 6.646953231504538984, -5.653124999385485516 ) ) ;
#15283 = CARTESIAN_POINT ( 'NONE',  ( 12.50000000000000355, 100.1101862821014521, 0.1745138560725507937 ) ) ;
#15284 = CARTESIAN_POINT ( 'NONE',  ( 10.83675517735179206, 19.13981371789855146, -11.08355503943118769 ) ) ;
#15285 = EDGE_CURVE ( 'NONE', #11580, #20044, #32605, .T. ) ;
#15286 = CARTESIAN_POINT ( 'NONE',  ( 0.000000000000000000, 148.0000000000000000, 7.500000000000000000 ) ) ;
#15287 = CARTESIAN_POINT ( 'NONE',  ( 19.39230484541326760, 243.8486538117966802, 5.999999999999999112 ) ) ;
#15288 = CARTESIAN_POINT ( 'NONE',  ( -33.37872103062156981, 205.4690446883607535, 1.090244570138264368 ) ) ;
#15289 = PRODUCT_DEFINITION ( 'UNKNOWN', '', #22658, #34990 ) ;
#15290 = CARTESIAN_POINT ( 'NONE',  ( 15.00000000000000178, 245.5375000000000227, 3.464101615137757051 ) ) ;
#15291 = CARTESIAN_POINT ( 'NONE',  ( 37.34434378849074676, -3.464101615137751278, 167.9744248827517197 ) ) ;
#15292 = CARTESIAN_POINT ( 'NONE',  ( 8.962234695871567070, 131.8398137178985792, 8.715434833792127023 ) ) ;
#15293 = CARTESIAN_POINT ( 'NONE',  ( -58.90997103062156270, 215.5714017266979852, 3.350049139982118618 ) ) ;
#15294 = CARTESIAN_POINT ( 'NONE',  ( -33.96502896937850124, 217.3034525342667962, -4.350049139982195001 ) ) ;
#15295 = PRODUCT_CONTEXT ( 'NONE', #1065, 'mechanical' ) ;
#15296 = CARTESIAN_POINT ( 'NONE',  ( 23.87821517812500005, -4.985214923628404016, -0.5531249993854792102 ) ) ;
#15297 = CARTESIAN_POINT ( 'NONE',  ( 13.62178482187501416, 199.5031250006145456, 23.59362340125806767 ) ) ;
#15298 = CARTESIAN_POINT ( 'NONE',  ( -2.908627838312453306, 114.8773137178985735, 15.53471296425188797 ) ) ;
#15299 = CARTESIAN_POINT ( 'NONE',  ( -57.12127896937847993, 216.5309553116391612, 1.626142955000506873 ) ) ;
#15300 = ORIENTED_EDGE ( 'NONE', *, *, #7804, .F. ) ;
#15301 = CARTESIAN_POINT ( 'NONE',  ( -11.48171059495397373, 31.68518628210144428, -4.944772684328680334 ) ) ;
#15302 = CARTESIAN_POINT ( 'NONE',  ( 20.99999999999997868, 244.7687500012290513, 5.999999999999999112 ) ) ;
#15303 = AXIS2_PLACEMENT_3D ( 'NONE', #7164, #15503, #4120 ) ;
#15304 = CARTESIAN_POINT ( 'NONE',  ( -27.00000000000000355, 197.7125000000000057, -15.58845726811989429 ) ) ;
#15305 = CARTESIAN_POINT ( 'NONE',  ( 31.31406506914986920, 7.209453229046482114, 167.8903031944757629 ) ) ;
#15306 = CARTESIAN_POINT ( 'NONE',  ( -10.83675517735155047, 96.66018628210144925, -11.08355503943142750 ) ) ;
#15307 = CARTESIAN_POINT ( 'NONE',  ( -68.60788769728824832, 216.4690446883607535, 1.857196546604031662 ) ) ;
#15308 = CARTESIAN_POINT ( 'NONE',  ( 13.44051670066911441, 5.407089921784856479, -0.6656249993855500868 ) ) ;
#15309 = CARTESIAN_POINT ( 'NONE',  ( -9.465287035748065847, 49.79768628210144499, -2.064181346179273735 ) ) ;
#15310 = DIRECTION ( 'NONE',  ( -1.000000000000000000, 0.000000000000000000, 0.000000000000000000 ) ) ;
#15311 = PLANE ( 'NONE',  #19040 ) ;
#15312 = CARTESIAN_POINT ( 'NONE',  ( -10.69584247140444866, 85.44768628210144357, 6.932735513423972762 ) ) ;
#15313 = CARTESIAN_POINT ( 'NONE',  ( 0.000000000000000000, 210.0000000000000284, 0.000000000000000000 ) ) ;
#15314 = CARTESIAN_POINT ( 'NONE',  ( 10.49999999999999645, 244.5000000000000000, 2.500000000000000000 ) ) ;
#15315 = ORIENTED_EDGE ( 'NONE', *, *, #34344, .F. ) ;
#15316 = CARTESIAN_POINT ( 'NONE',  ( 26.99999999999999645, 244.8437500012290400, 3.464101615137751278 ) ) ;
#15317 = CARTESIAN_POINT ( 'NONE',  ( 15.00000000000000000, 0.000000000000000000, -0.4500000000000059508 ) ) ;
#15318 = AXIS2_PLACEMENT_3D ( 'NONE', #11319, #8115, #17387 ) ;
#15319 = CARTESIAN_POINT ( 'NONE',  ( -13.50000000000000533, 198.2375000012290229, -23.38268590217984411 ) ) ;
#15320 = CARTESIAN_POINT ( 'NONE',  ( 28.06362094583411704, -5.407089921784865361, 166.5560207186516664 ) ) ;
#15321 = UNCERTAINTY_MEASURE_WITH_UNIT (LENGTH_MEASURE( 1.000000000000000082E-05 ), #32625, 'distance_accuracy_value', 'NONE');
#15322 = CARTESIAN_POINT ( 'NONE',  ( 36.98809468990261706, 3.464101615137759271, 163.9024790530773146 ) ) ;
#15323 = DIRECTION ( 'NONE',  ( 0.000000000000000000, -0.000000000000000000, 1.000000000000000000 ) ) ;
#15324 = CARTESIAN_POINT ( 'NONE',  ( 21.00000000000000000, 248.9874999999999829, -6.928203230275506996 ) ) ;
#15325 = CARTESIAN_POINT ( 'NONE',  ( 27.24356964375000700, 197.2906250006145399, 15.72908226750537075 ) ) ;
#15326 = CARTESIAN_POINT ( 'NONE',  ( 2.311890736173452865, 101.0773137178985621, -12.53471296425189152 ) ) ;
#15327 = CARTESIAN_POINT ( 'NONE',  ( -11.48171059495397373, 96.08518628210146062, -4.944772684328680334 ) ) ;
#15328 = VERTEX_POINT ( 'NONE', #35068 ) ;
#15329 = VERTEX_POINT ( 'NONE', #26918 ) ;
#15330 = CARTESIAN_POINT ( 'NONE',  ( -1.909035429704832693E-15, 199.5500000012290513, -31.17691453623979214 ) ) ;
#15331 = CARTESIAN_POINT ( 'NONE',  ( 15.24356964375000167, 239.8843750006145399, 3.323476615752272600 ) ) ;
#15332 = CARTESIAN_POINT ( 'NONE',  ( -13.04141134922778456, 70.02731371789855075, 8.927990412390377273 ) ) ;
#15333 = CARTESIAN_POINT ( 'NONE',  ( 26.75643035624999655, 7.049594010296217766E-16, -4.078124999385480010 ) ) ;
#15334 = CARTESIAN_POINT ( 'NONE',  ( 18.12178482187499640, 248.4343750006145228, -4.985214923628404904 ) ) ;
#15335 = CARTESIAN_POINT ( 'NONE',  ( -7.954856959092191815, 96.37268628210144072, -5.529263428287477744 ) ) ;
#15336 = AXIS2_PLACEMENT_3D ( 'NONE', #36261, #36446, #4241 ) ;
#15337 = DIRECTION ( 'NONE',  ( 0.000000000000000000, 1.000000000000000000, 0.000000000000000000 ) ) ;
#15338 = CARTESIAN_POINT ( 'NONE',  ( 3.474262827703532341, 55.36481371789856354, -8.843639120294245259 ) ) ;
#15339 = CARTESIAN_POINT ( 'NONE',  ( 22.80587116629410716, 7.646167579472015790E-16, -4.415624999385525662 ) ) ;
#15340 = ADVANCED_FACE ( 'NONE', ( #18031 ), #33743, .T. ) ;
#15341 = CARTESIAN_POINT ( 'NONE',  ( 7.954856959092311719, 111.4273137178985422, -5.529263428287300108 ) ) ;
#15342 = CARTESIAN_POINT ( 'NONE',  ( 6.932735513424201024, 28.05231371789855643, -10.69584247140429412 ) ) ;
#15343 = CARTESIAN_POINT ( 'NONE',  ( 28.21190614766015159, -5.196152422706632912, 166.8536042073800729 ) ) ;
#15344 = CARTESIAN_POINT ( 'NONE',  ( -8.715434833791929847, 96.66018628210146346, -8.962234695871762469 ) ) ;
#15345 = CARTESIAN_POINT ( 'NONE',  ( 22.56230152254411081, -3.464101615137751278, -5.999999998770999099 ) ) ;
#15346 = CARTESIAN_POINT ( 'NONE',  ( -67.81622103062157692, 211.0902445701382533, 4.530955311639240257 ) ) ;
#15347 = CARTESIAN_POINT ( 'NONE',  ( 18.00000000000000000, 5.196152422706630247, -7.218749998770951137 ) ) ;
#15348 = CARTESIAN_POINT ( 'NONE',  ( 24.79520095057666396, 0.000000000000000000, 165.0162730863461604 ) ) ;
#15349 = CARTESIAN_POINT ( 'NONE',  ( 5.770363421893814682, 83.43518628210145494, 14.38691631536207183 ) ) ;
#15350 = CARTESIAN_POINT ( 'NONE',  ( 13.44051670066911441, -5.407089921784865361, -4.171874999385538629 ) ) ;
#15351 = CARTESIAN_POINT ( 'NONE',  ( 10.56230152254411081, 0.000000000000000000, -3.037499998771009402 ) ) ;
#15352 = CARTESIAN_POINT ( 'NONE',  ( 13.56230152254410370, 5.196152422706630247, -7.162499998770998744 ) ) ;
#15353 = CARTESIAN_POINT ( 'NONE',  ( 6.840914352312096547, 108.1601862821014635, -6.594114490232313663 ) ) ;
#15354 = EDGE_CURVE ( 'NONE', #35216, #1170, #20679, .T. ) ;
#15355 = CARTESIAN_POINT ( 'NONE',  ( 0.1745138560725515708, 134.6101862821014663, -12.50000000000000355 ) ) ;
#15356 = AXIS2_PLACEMENT_3D ( 'NONE', #11059, #34547, #16942 ) ;
#15357 = CARTESIAN_POINT ( 'NONE',  ( -27.24356964374999635, 196.2968750006145342, 15.72908226750539384 ) ) ;
#15358 = CARTESIAN_POINT ( 'NONE',  ( 15.24356964374999990, 243.4093750006145171, -3.323476615752268604 ) ) ;
#15359 = ORIENTED_EDGE ( 'NONE', *, *, #26547, .F. ) ;
#15360 = EDGE_CURVE ( 'NONE', #31488, #30489, #12747, .T. ) ;
#15361 = CARTESIAN_POINT ( 'NONE',  ( 34.38638464322509947, 5.407089921784857367, 167.1886127560748321 ) ) ;
#15362 = CARTESIAN_POINT ( 'NONE',  ( 15.24356964375000167, -3.323476615752272600, -1.903124999385467753 ) ) ;
#15363 = CARTESIAN_POINT ( 'NONE',  ( 19.56230152254412147, -5.196152422706635576, -4.800000000000082423 ) ) ;
#15365 = CARTESIAN_POINT ( 'NONE',  ( 5.999999999999999112, -30.00000000000000000, -19.99999999999999289 ) ) ;
#15364 =( BOUNDED_CURVE ( )  B_SPLINE_CURVE ( 2, ( #32626, #18238, #15577, #1347, #36027, #15769, #9323, #4379, #24660 ),
 .UNSPECIFIED., .F., .F. ) 
 B_SPLINE_CURVE_WITH_KNOTS ( ( 3, 2, 2, 2, 3 ),
 ( 0.06250000000000000000, 0.06944444444444444753, 0.08333333333333332871, 0.09722222222222222376, 0.1041666666666666713 ),
 .UNSPECIFIED. ) 
 CURVE ( )  GEOMETRIC_REPRESENTATION_ITEM ( )  RATIONAL_B_SPLINE_CURVE ( ( 0.9330127018922194093, 0.9330127018922194093, 1.000000000000000000, 0.8660254037844387076, 1.000000000000000000, 0.8660254037844387076, 1.000000000000000000, 0.9330127018922192983, 0.9330127018922194093 ) ) 
 REPRESENTATION_ITEM ( '' )  );
#15366 = CARTESIAN_POINT ( 'NONE',  ( 10.56230152254411081, 0.000000000000000000, -3.037499998771009402 ) ) ;
#15367 = LINE ( 'NONE', #15555, #1100 ) ;
#15368 = CARTESIAN_POINT ( 'NONE',  ( -20.86978604919638869, 194.8026013911397456, -17.51182792271053046 ) ) ;
#15369 = CARTESIAN_POINT ( 'NONE',  ( -9.465287035748106703, 24.60231371789854649, 2.064181346179061460 ) ) ;
#15370 = CARTESIAN_POINT ( 'NONE',  ( -27.24356964374999279, 197.1968750006145115, 15.72908226750539384 ) ) ;
#15372 = VERTEX_POINT ( 'NONE', #7753 ) ;
#15371 = ORIENTED_EDGE ( 'NONE', *, *, #23681, .T. ) ;
#15373 = COLOUR_RGB ( '',0.8941176470588234615, 0.8941176470588234615, 0.8941176470588234615 ) ;
#15374 = CARTESIAN_POINT ( 'NONE',  ( 21.00000000000000000, 246.2593750006145115, 6.646953231504538984 ) ) ;
#15375 = CARTESIAN_POINT ( 'NONE',  ( 11.48171059495408208, 19.71481371789854364, -4.944772684328420986 ) ) ;
#15376 = CARTESIAN_POINT ( 'NONE',  ( 26.75643035624999655, 7.049594010296217766E-16, -2.165624999385467930 ) ) ;
#15377 = CARTESIAN_POINT ( 'NONE',  ( -6.092822981423666739, 137.0148137178985621, -14.25334919248795096 ) ) ;
#15378 = CARTESIAN_POINT ( 'NONE',  ( 21.00000000000000000, -6.928203230275506996, -6.581249998770967835 ) ) ;
#15379 = CARTESIAN_POINT ( 'NONE',  ( 16.56230152254410726, 6.928203230275506996, -8.099999998770989862 ) ) ;
#15380 = VERTEX_POINT ( 'NONE', #2427 ) ;
#15381 = CARTESIAN_POINT ( 'NONE',  ( 10.31873187879410736, -3.604726614523244610, -6.909374999385496707 ) ) ;
#15382 = CARTESIAN_POINT ( 'NONE',  ( -13.62178482187498396, 197.6281250006145171, 23.59362340125808188 ) ) ;
#15383 = CARTESIAN_POINT ( 'NONE',  ( 12.50000000000000355, 136.9101862821014777, 0.1745138560725507937 ) ) ;
#15384 = CARTESIAN_POINT ( 'NONE',  ( 27.86752052465190133, -5.407089921784865361, 164.3145826479452296 ) ) ;
#15385 = ADVANCED_FACE ( 'NONE', ( #34083 ), #16665, .F. ) ;
#15386 =( BOUNDED_CURVE ( )  B_SPLINE_CURVE ( 2, ( #14333, #17183, #20584, #14516, #25887, #31943, #6356 ),
 .UNSPECIFIED., .F., .F. ) 
 B_SPLINE_CURVE_WITH_KNOTS ( ( 3, 2, 2, 3 ),
 ( 0.3043478260869552088, 0.3115942028985494994, 0.3188405797101437900, 0.3260869565217381361 ),
 .UNSPECIFIED. ) 
 CURVE ( )  GEOMETRIC_REPRESENTATION_ITEM ( )  RATIONAL_B_SPLINE_CURVE ( ( 1.000000000000024647, 0.8660254037844140607, 1.000000000000000000, 0.8660254037844387076, 1.000000000000000000, 0.8660254037844571373, 0.9999999999999815703 ) ) 
 REPRESENTATION_ITEM ( '' )  );
#15387 = CARTESIAN_POINT ( 'NONE',  ( -59.49627896937850835, 201.4690446883607251, -2.162041339862721845 ) ) ;
#15388 = CARTESIAN_POINT ( 'NONE',  ( 15.24356964374999990, 245.6593750006145740, -3.323476615752268604 ) ) ;
#15389 = SHAPE_REPRESENTATION_RELATIONSHIP ( 'NONE' , 'NONE' ,  #36285, #18760 ) ;
#15390 = CARTESIAN_POINT ( 'NONE',  ( 13.49999999999999645, 196.7000000000000171, -23.38268590217984766 ) ) ;
#15391 = CARTESIAN_POINT ( 'NONE',  ( -41.28794563604517265, 206.7903428501025758, 3.378800118222471838 ) ) ;
#15392 = DIRECTION ( 'NONE',  ( 0.000000000000000000, -0.000000000000000000, 1.000000000000000000 ) ) ;
#15393 = CARTESIAN_POINT ( 'NONE',  ( 34.25565102910361759, -5.407089921784855591, 165.6943207089371981 ) ) ;
#15394 = ORIENTED_EDGE ( 'NONE', *, *, #15931, .F. ) ;
#15395 = CARTESIAN_POINT ( 'NONE',  ( 24.00000000000000000, 247.9562500012290229, 5.196152422706629359 ) ) ;
#15396 = CARTESIAN_POINT ( 'NONE',  ( 2.908627838312118019, 138.9226862821014663, 15.53471296425195369 ) ) ;
#15397 = COLOUR_RGB ( '',0.8941176470588234615, 0.8941176470588234615, 0.8941176470588234615 ) ;
#15398 = CARTESIAN_POINT ( 'NONE',  ( -47.23288769728824121, 201.5309553116392181, -2.393094931466246855 ) ) ;
#15399 = AXIS2_PLACEMENT_3D ( 'NONE', #23267, #2788, #3162 ) ;
#15400 = CARTESIAN_POINT ( 'NONE',  ( -8.710071997420127943, 123.6851862821014549, -3.796722387233380402 ) ) ;
#15401 = AXIS2_PLACEMENT_3D ( 'NONE', #18040, #25485, #14996 ) ;
#15402 = CARTESIAN_POINT ( 'NONE',  ( 15.00000000000000000, 249.1187500012290741, -3.464101615137752610 ) ) ;
#15403 = CARTESIAN_POINT ( 'NONE',  ( 12.46528703574805874, 35.99768628210144072, 2.660918448318279950 ) ) ;
#15404 = ADVANCED_FACE ( 'NONE', ( #21981 ), #27201, .T. ) ;
#15405 = CARTESIAN_POINT ( 'NONE',  ( 10.56230152254410726, 0.000000000000000000, -6.300000000000055778 ) ) ;
#15406 = EDGE_LOOP ( 'NONE', ( #8472, #22000, #12085, #7611 ) ) ;
#15407 = CARTESIAN_POINT ( 'NONE',  ( 10.49999999999999822, 210.0000000000000284, 2.500000000000000000 ) ) ;
#15408 = CARTESIAN_POINT ( 'NONE',  ( -11.08355503943142573, 121.9601862821014606, 10.83675517735155402 ) ) ;
#15409 = SURFACE_SIDE_STYLE ('',( #18254 ) ) ;
#15410 = CARTESIAN_POINT ( 'NONE',  ( 2.064181346179272847, 6.097686282101443922, -9.465287035748065847 ) ) ;
#15411 = CARTESIAN_POINT ( 'NONE',  ( -1.926257025242585782E-15, 197.4406250006145740, -31.45816453501075927 ) ) ;
#15412 = CARTESIAN_POINT ( 'NONE',  ( 3.061616997868383043E-15, 200.0000000000000000, 25.00000000000000000 ) ) ;
#15413 = CARTESIAN_POINT ( 'NONE',  ( 22.56378207682202586, 0.6013373594316471227, -10.00000000000000000 ) ) ;
#15414 = CARTESIAN_POINT ( 'NONE',  ( 15.81644453130096828, -3.010575440655008261, -7.999999999999994671 ) ) ;
#15415 = DIRECTION ( 'NONE',  ( 0.9961946980917462113, 0.000000000000000000, -0.08715574274765118534 ) ) ;
#15416 = CARTESIAN_POINT ( 'NONE',  ( -5.233372021372612259, 78.65231371789856496, 8.152565276336593669 ) ) ;
#15417 = DIRECTION ( 'NONE',  ( -0.000000000000000000, -1.000000000000000000, -0.000000000000000000 ) ) ;
#15418 = ORIENTED_EDGE ( 'NONE', *, *, #26483, .F. ) ;
#15419 = CARTESIAN_POINT ( 'NONE',  ( 18.00000000000000000, 245.0312500012290400, -5.196152422706630247 ) ) ;
#15420 = CARTESIAN_POINT ( 'NONE',  ( -0.1745138560722763466, 73.18981371789855928, -12.50000000000000355 ) ) ;
#15421 = CARTESIAN_POINT ( 'NONE',  ( 10.31873187879411091, -3.604726614523244610, -2.859374999385534633 ) ) ;
#15422 = CARTESIAN_POINT ( 'NONE',  ( -10.08800066309955490, 142.9999999999999147, 9.061245623615871381 ) ) ;
#15423 = CARTESIAN_POINT ( 'NONE',  ( 23.87821517812499650, 4.985214923628404904, -4.453124999385494220 ) ) ;
#15424 = CARTESIAN_POINT ( 'NONE',  ( 8.962234695871567070, 39.83981371789855075, 8.715434833792127023 ) ) ;
#15425 = ORIENTED_EDGE ( 'NONE', *, *, #22157, .T. ) ;
#15426 = VERTEX_POINT ( 'NONE', #17948 ) ;
#15427 = CARTESIAN_POINT ( 'NONE',  ( 28.01580572647793943, -5.196152422706632912, 164.6121661366736078 ) ) ;
#15428 = CARTESIAN_POINT ( 'NONE',  ( 18.12178482187500350, 243.5218750006145001, 4.985214923628407568 ) ) ;
#15429 = EDGE_CURVE ( 'NONE', #13097, #33922, #11686, .T. ) ;
#15430 = CARTESIAN_POINT ( 'NONE',  ( 2.311890736173175753, 28.52268628210144641, 12.53471296425194836 ) ) ;
#15431 = CARTESIAN_POINT ( 'NONE',  ( -31.59002896937850124, 204.4285982733020433, 3.350049139982171020 ) ) ;
#15432 = CARTESIAN_POINT ( 'NONE',  ( 10.31873187879410736, 3.604726614523236616, -0.1781249993854788494 ) ) ;
#15433 = CARTESIAN_POINT ( 'NONE',  ( -61.67336230271183695, 215.6869285224997270, 3.149950860017831200 ) ) ;
#15434 = DIRECTION ( 'NONE',  ( 0.000000000000000000, 1.000000000000000000, 0.000000000000000000 ) ) ;
#15435 = CARTESIAN_POINT ( 'NONE',  ( -2.660918448318004614, 91.30231371789857064, -12.46528703574811558 ) ) ;
#15436 = CARTESIAN_POINT ( 'NONE',  ( -45.05580436395490551, 214.5000000000000284, 0.1155267958017899832 ) ) ;
#15437 = CARTESIAN_POINT ( 'NONE',  ( -69.20163769728823411, 215.6869285224996986, -3.149950860017881382 ) ) ;
#15438 = CARTESIAN_POINT ( 'NONE',  ( 20.99999999999999645, -6.646953231504538984, -6.890624999385480898 ) ) ;
#15439 = CARTESIAN_POINT ( 'NONE',  ( -68.00669563604516554, 209.8844732041982013, -6.500000000000000888 ) ) ;
#15440 = CARTESIAN_POINT ( 'NONE',  ( -5.770363421894122880, 59.96481371789855075, 14.38691631536194393 ) ) ;
#15441 = CARTESIAN_POINT ( 'NONE',  ( -49.99627896937850835, 201.4690446883607251, -2.162041339862721845 ) ) ;
#15442 = CARTESIAN_POINT ( 'NONE',  ( 36.83448269341756998, -3.464101615137414214, 162.1466858989149102 ) ) ;
#15443 = CARTESIAN_POINT ( 'NONE',  ( -11.61527771782819940, 85.73518628210143788, 4.622313124798574258 ) ) ;
#15444 = CARTESIAN_POINT ( 'NONE',  ( -15.50000000000000533, 21.91018628210143859, -0.1745138560725808530 ) ) ;
#15445 = CARTESIAN_POINT ( 'NONE',  ( 10.56230152254410726, 0.000000000000000000, -0.9000000000000396572 ) ) ;
#15446 = CARTESIAN_POINT ( 'NONE',  ( 20.99999999999999645, 185.0294372515228645, 5.999999999999999112 ) ) ;
#15447 = ORIENTED_EDGE ( 'NONE', *, *, #30218, .F. ) ;
#15448 = CARTESIAN_POINT ( 'NONE',  ( 14.38691631536207538, 44.33518628210144641, -5.770363421893813793 ) ) ;
#15449 = CARTESIAN_POINT ( 'NONE',  ( -27.24356964375000345, 197.0656250006145171, -15.72908226750537786 ) ) ;
#15450 = CARTESIAN_POINT ( 'NONE',  ( -81.72704584564829133, 216.6260876520869658, 7.500000000000000000 ) ) ;
#15451 = CARTESIAN_POINT ( 'NONE',  ( 15.00000000000000355, 7.347880794884112834E-16, -8.000000000000000000 ) ) ;
#15452 = CARTESIAN_POINT ( 'NONE',  ( -37.53497103062156981, 204.4285982733020148, -3.350049139982115509 ) ) ;
#15453 = CARTESIAN_POINT ( 'NONE',  ( 12.50000000000000355, 26.51018628210144357, 0.1745138560725507937 ) ) ;
#15454 = VECTOR ( 'NONE', #18932, 1000.000000000000000 ) ;
#15455 = CARTESIAN_POINT ( 'NONE',  ( 26.75643035624999655, 249.5968750006145171, 3.323476615752267715 ) ) ;
#15456 = CARTESIAN_POINT ( 'NONE',  ( 9.465287035748106703, 139.6023137178985394, -2.064181346179063237 ) ) ;
#15457 = CARTESIAN_POINT ( 'NONE',  ( 18.12178482187500350, 245.8843750006145115, 4.985214923628407568 ) ) ;
#15458 = EDGE_LOOP ( 'NONE', ( #25706, #4690, #657, #31084 ) ) ;
#15459 = CARTESIAN_POINT ( 'NONE',  ( 15.00000000000000000, 3.464101615137752166, -7.237499999999992717 ) ) ;
#15460 = CARTESIAN_POINT ( 'NONE',  ( 15.00000000000000000, 0.000000000000000000, -4.500000000000003553 ) ) ;
#15461 = CARTESIAN_POINT ( 'NONE',  ( -10.49813415416004858, 134.4273137178985564, 7.228626920338840023 ) ) ;
#15462 = CARTESIAN_POINT ( 'NONE',  ( 22.80587116629410716, 3.604726614523238837, -7.528124999385559235 ) ) ;
#15463 = CARTESIAN_POINT ( 'NONE',  ( 24.87364111904954811, 0.000000000000000000, 165.9128483146287465 ) ) ;
#15464 = CARTESIAN_POINT ( 'NONE',  ( -27.24356964375000345, 199.8031250006145285, 0.000000000000000000 ) ) ;
#15465 = CARTESIAN_POINT ( 'NONE',  ( -26.99999999999998934, 199.1375000000000171, 15.58845726811991561 ) ) ;
#15466 = CARTESIAN_POINT ( 'NONE',  ( -10.69584247140444866, 48.64768628210144641, 6.932735513423972762 ) ) ;
#15467 = ORIENTED_EDGE ( 'NONE', *, *, #34443, .T. ) ;
#15468 = ORIENTED_EDGE ( 'NONE', *, *, #18627, .T. ) ;
#15469 = CARTESIAN_POINT ( 'NONE',  ( 29.51984228635672380, 5.908847293266075162, 159.3365288790247121 ) ) ;
#15470 = CARTESIAN_POINT ( 'NONE',  ( 20.99999999999999645, -6.928203230275506996, -2.587499999999983480 ) ) ;
#15471 = CARTESIAN_POINT ( 'NONE',  ( 16.56230152254410726, 0.000000000000000000, -10.00000000000000000 ) ) ;
#15472 = CARTESIAN_POINT ( 'NONE',  ( 22.60769515458670753, 243.1174038105676516, -6.000000000000011546 ) ) ;
#15473 = CARTESIAN_POINT ( 'NONE',  ( 15.24356964374999990, 3.323476615752268604, -8.278124999385466865 ) ) ;
#15474 = CARTESIAN_POINT ( 'NONE',  ( 8.715434833791931624, 101.2601862821014578, 8.962234695871760692 ) ) ;
#15475 = CARTESIAN_POINT ( 'NONE',  ( 15.53471296425188797, 29.77731371789854364, 2.908627838312457747 ) ) ;
#15476 = CARTESIAN_POINT ( 'NONE',  ( 19.56230152254412147, -5.196152422706635576, -5.700000000000065903 ) ) ;
#15477 = CARTESIAN_POINT ( 'NONE',  ( 19.44430458907412174, 214.1485210958030052, 5.808099892140972109 ) ) ;
#15478 = CARTESIAN_POINT ( 'NONE',  ( -67.21502896937850835, 213.8393509191290889, -2.350049139982142155 ) ) ;
#15479 = CARTESIAN_POINT ( 'NONE',  ( 0.000000000000000000, 210.0000000000000284, 0.000000000000000000 ) ) ;
#15480 = CARTESIAN_POINT ( 'NONE',  ( 28.17268606342371129, -5.196152422706632912, 166.4053165932387515 ) ) ;
#15481 = CARTESIAN_POINT ( 'NONE',  ( 9.534712964251900402, 11.37731371789854506, 1.715153634034445540 ) ) ;
#15482 = CARTESIAN_POINT ( 'NONE',  ( -50.99330436395489841, 210.1155267958017134, -6.500000000000000888 ) ) ;
#15483 = CARTESIAN_POINT ( 'NONE',  ( -35.54836230271182984, 202.5810206699313767, -4.149950860017804111 ) ) ;
#15484 = VECTOR ( 'NONE', #35123, 1000.000000000000000 ) ;
#15485 = ITEM_DEFINED_TRANSFORMATION ( 'NONE', 'NONE', #23870,  #17215 ) ;
#15486 = CARTESIAN_POINT ( 'NONE',  ( 23.99999999999999645, 247.1500000000000057, -5.196152422706631135 ) ) ;
#15487 = CARTESIAN_POINT ( 'NONE',  ( -27.24356964374999990, 198.4156250006145399, -15.72908226750537786 ) ) ;
#15488 = CARTESIAN_POINT ( 'NONE',  ( -15.46528703574811736, 107.4023137178985650, 3.257655550456946436 ) ) ;
#15489 = CARTESIAN_POINT ( 'NONE',  ( -59.10044563604516554, 205.1570982666397072, -4.673758765035155527 ) ) ;
#15490 = ORIENTED_EDGE ( 'NONE', *, *, #12903, .F. ) ;
#15491 = CARTESIAN_POINT ( 'NONE',  ( -4.944772684328673229, 29.38518628210144712, 11.48171059495397728 ) ) ;
#15492 = CARTESIAN_POINT ( 'NONE',  ( 26.99999999999967670, 3.464101615137938683, -7.837500000000005684 ) ) ;
#15493 = DIRECTION ( 'NONE',  ( -0.000000000000000000, 0.000000000000000000, 1.000000000000000000 ) ) ;
#15494 = CARTESIAN_POINT ( 'NONE',  ( 28.18128119854344860, -5.407089921784865361, 167.9008835610755455 ) ) ;
#15495 = CARTESIAN_POINT ( 'NONE',  ( 14.38691631536207538, 108.7351862821014663, -5.770363421893813793 ) ) ;
#15496 = CARTESIAN_POINT ( 'NONE',  ( -65.83705436395489130, 205.3262412349647548, -4.842901733360204908 ) ) ;
#15497 = EDGE_CURVE ( 'NONE', #20530, #13274, #9050, .T. ) ;
#15498 = CARTESIAN_POINT ( 'NONE',  ( 10.31873187879410914, 0.000000000000000000, -3.740624999385516958 ) ) ;
#15499 = CARTESIAN_POINT ( 'NONE',  ( -3.796722387233375073, 66.18518628210145494, 8.710071997420127943 ) ) ;
#15500 = DIRECTION ( 'NONE',  ( -0.000000000000000000, -0.000000000000000000, 1.000000000000000000 ) ) ;
#15501 = CARTESIAN_POINT ( 'NONE',  ( -34.76413769728823411, 214.1499508600179240, 7.418979330068584233 ) ) ;
#15502 = EDGE_CURVE ( 'NONE', #2909, #25376, #26979, .T. ) ;
#15503 = DIRECTION ( 'NONE',  ( 0.000000000000000000, 0.000000000000000000, 1.000000000000000000 ) ) ;
#15504 = CARTESIAN_POINT ( 'NONE',  ( 11.48171059495397728, 73.08518628210144641, 4.944772684328674117 ) ) ;
#15505 = DIRECTION ( 'NONE',  ( 0.9961946980917462113, 0.000000000000000000, -0.08715574274765178209 ) ) ;
#15506 = PLANE ( 'NONE',  #25053 ) ;
#15508 = CARTESIAN_POINT ( 'NONE',  ( 10.56230152254410903, 0.000000000000000000, -1.800000000000051559 ) ) ;
#15507 = CARTESIAN_POINT ( 'NONE',  ( 8.152565276336714462, 44.04768628210143788, -5.233372021372432847 ) ) ;
#15509 = CARTESIAN_POINT ( 'NONE',  ( 23.99999999999999645, 244.9562500012290513, -5.196152422706631135 ) ) ;
#15510 = CARTESIAN_POINT ( 'NONE',  ( 23.87821517812500005, -4.985214923628404016, -9.440624999385471838 ) ) ;
#15511 = CARTESIAN_POINT ( 'NONE',  ( -27.00000000000000355, 198.2750000012290172, -15.58845726811989429 ) ) ;
#15512 = CARTESIAN_POINT ( 'NONE',  ( 37.24626209435294300, -3.604726614523238837, 164.0586977410752638 ) ) ;
#15513 = CARTESIAN_POINT ( 'NONE',  ( 33.88511868327108090, 5.196152422706637353, 162.8564407400748451 ) ) ;
#15514 = CARTESIAN_POINT ( 'NONE',  ( 21.00000000000000000, 245.8374999999999773, -6.928203230275506996 ) ) ;
#15515 = CARTESIAN_POINT ( 'NONE',  ( 27.24356964375000345, 197.3281250006145342, -3.336375036156643733E-15 ) ) ;
#15516 = AXIS2_PLACEMENT_3D ( 'NONE', #22959, #5501, #5878 ) ;
#15517 = ADVANCED_FACE ( 'NONE', ( #26458 ), #28931, .F. ) ;
#15518 = CARTESIAN_POINT ( 'NONE',  ( -12.46528703574811558, 98.20231371789856212, 2.660918448318003726 ) ) ;
#15519 = CARTESIAN_POINT ( 'NONE',  ( 10.49813415415989581, 100.9726862821014635, 7.228626920339069173 ) ) ;
#15520 = VERTEX_POINT ( 'NONE', #3154 ) ;
#15521 = ORIENTED_EDGE ( 'NONE', *, *, #33476, .F. ) ;
#15522 = CARTESIAN_POINT ( 'NONE',  ( 27.24356964375000345, 196.4281250006145569, -3.336375036156643733E-15 ) ) ;
#15523 = CARTESIAN_POINT ( 'NONE',  ( 13.56230152254411614, -5.196152422706632912, -9.262499998771044574 ) ) ;
#15524 = CARTESIAN_POINT ( 'NONE',  ( 5.770363421894130873, 73.76481371789856212, -14.38691631536193860 ) ) ;
#15525 = CARTESIAN_POINT ( 'NONE',  ( 15.24356964374999990, 3.323476615752268604, -5.690624999385482496 ) ) ;
#15526 = CARTESIAN_POINT ( 'NONE',  ( 15.24356964375000167, 245.8468750006145171, 3.323476615752272600 ) ) ;
#15527 = CARTESIAN_POINT ( 'NONE',  ( 0.1745138560725194299, 107.0101862821014578, -9.500000000000005329 ) ) ;
#15528 = FACE_BOUND ( 'NONE', #22217, .T. ) ;
#15529 = CARTESIAN_POINT ( 'NONE',  ( -8.710071997420207879, 51.91481371789856070, 3.796722387233182339 ) ) ;
#15530 = CARTESIAN_POINT ( 'NONE',  ( 16.56230152254411081, 7.209453229046475009, -5.653124999385517491 ) ) ;
#15531 = CARTESIAN_POINT ( 'NONE',  ( -3.474262827703527901, 115.1648137178985678, 8.843639120294245259 ) ) ;
#15532 = DIRECTION ( 'NONE',  ( 0.08715574274765150453, 0.000000000000000000, 0.9961946980917461003 ) ) ;
#15533 = CARTESIAN_POINT ( 'NONE',  ( -11.48171059495408208, 24.31481371789855217, 4.944772684328421875 ) ) ;
#15534 = CARTESIAN_POINT ( 'NONE',  ( 37.18746345154525557, -3.464101615137590073, 166.1812744261865191 ) ) ;
#15535 = CARTESIAN_POINT ( 'NONE',  ( 8.715434833791931624, 73.66018628210144925, 8.962234695871760692 ) ) ;
#15536 = CARTESIAN_POINT ( 'NONE',  ( 19.56230152254410726, 5.196152422706631135, -6.787499998771012955 ) ) ;
#15537 = DIRECTION ( 'NONE',  ( 0.000000000000000000, 0.000000000000000000, 1.000000000000000000 ) ) ;
#15538 = CARTESIAN_POINT ( 'NONE',  ( 30.98559686366965238, -7.209453229046475009, 164.1358944260424835 ) ) ;
#15539 = CARTESIAN_POINT ( 'NONE',  ( 13.44051670066911086, 5.407089921784862696, -3.421874999385537741 ) ) ;
#15540 = CARTESIAN_POINT ( 'NONE',  ( 19.56230152254410370, 5.196152422706631135, -3.187499998770992882 ) ) ;
#15541 = CARTESIAN_POINT ( 'NONE',  ( 20.99999999999999645, 242.0687500012290059, 5.999999999999998224 ) ) ;
#15542 = CARTESIAN_POINT ( 'NONE',  ( 15.00000000000000178, 244.1875000000000000, 3.464101615137757051 ) ) ;
#15543 = CARTESIAN_POINT ( 'NONE',  ( -6.840914352312096547, 112.7601862821014720, 6.594114490232313663 ) ) ;
#15544 = CARTESIAN_POINT ( 'NONE',  ( 7.234628195640318005, 199.0799038117967541, -26.99999999999999645 ) ) ;
#15545 = CARTESIAN_POINT ( 'NONE',  ( -12.46528703574805697, 132.5976862821014777, -2.660918448318280838 ) ) ;
#15546 = CARTESIAN_POINT ( 'NONE',  ( -27.24356964375000345, 196.2593750006145399, 0.000000000000000000 ) ) ;
#15547 = CARTESIAN_POINT ( 'NONE',  ( 23.87821517812500005, 249.1093750006145342, 4.985214923628404016 ) ) ;
#15548 = VERTEX_POINT ( 'NONE', #34804 ) ;
#15549 = CARTESIAN_POINT ( 'NONE',  ( 25.07300988058479874, -3.604726614523240613, 168.1916436865135722 ) ) ;
#15550 = CARTESIAN_POINT ( 'NONE',  ( 21.00000000000000000, -6.646953231504538984, -2.278124999385469529 ) ) ;
#15551 = AXIS2_PLACEMENT_3D ( 'NONE', #20103, #16708, #11377 ) ;
#15552 = CYLINDRICAL_SURFACE ( 'NONE', #13225, 5.999999999999994671 ) ;
#15553 = CARTESIAN_POINT ( 'NONE',  ( 24.34069010239548447, -4.874609697617195536, -8.000000000000003553 ) ) ;
#15554 = FACE_OUTER_BOUND ( 'NONE', #17468, .T. ) ;
#15555 = CARTESIAN_POINT ( 'NONE',  ( -6.000000000000000888, -30.00000000000000000, -19.99999999999999289 ) ) ;
#15556 = DIRECTION ( 'NONE',  ( 0.9961946980917462113, 0.000000000000000000, -0.08715574274765118534 ) ) ;
#15557 = CARTESIAN_POINT ( 'NONE',  ( -9.534712964251895073, 15.97731371789853405, -1.715153634034446428 ) ) ;
#15558 = CARTESIAN_POINT ( 'NONE',  ( 27.24356964374999279, 196.9718750006145456, -15.72908226750539207 ) ) ;
#15560 = ORIENTED_EDGE ( 'NONE', *, *, #29857, .T. ) ;
#15559 = ORIENTED_EDGE ( 'NONE', *, *, #32387, .T. ) ;
#15561 = CARTESIAN_POINT ( 'NONE',  ( 23.87821517812499650, 247.7968750006145058, -4.985214923628404904 ) ) ;
#15562 = CARTESIAN_POINT ( 'NONE',  ( -4.944772684328424539, 26.61481371789854578, -11.48171059495408031 ) ) ;
#15563 = CARTESIAN_POINT ( 'NONE',  ( 23.87821517812500005, -4.985214923628404016, -2.690624999385465621 ) ) ;
#15564 = CARTESIAN_POINT ( 'NONE',  ( -3.257655550456946880, 137.3023137178985564, -15.46528703574811736 ) ) ;
#15565 = CARTESIAN_POINT ( 'NONE',  ( 15.00000000000000000, 3.464101615137752166, -10.33124999877095362 ) ) ;
#15566 = CARTESIAN_POINT ( 'NONE',  ( -27.00000000000000355, 199.6625000012290343, 0.000000000000000000 ) ) ;
#15567 = ORIENTED_EDGE ( 'NONE', *, *, #751, .T. ) ;
#15568 = CARTESIAN_POINT ( 'NONE',  ( 22.80587116629411781, -3.604726614523238837, -5.859374999385516425 ) ) ;
#15569 = ORIENTED_EDGE ( 'NONE', *, *, #19616, .F. ) ;
#15570 = CARTESIAN_POINT ( 'NONE',  ( -27.24356964374999635, 197.5906250006145228, 15.72908226750539384 ) ) ;
#15571 = CARTESIAN_POINT ( 'NONE',  ( -2.311890736173176641, 134.3226862821014436, -12.53471296425194836 ) ) ;
#15572 = CARTESIAN_POINT ( 'NONE',  ( 24.71185827157421855, 0.000000000000000000, 164.0636619062959483 ) ) ;
#15573 = CARTESIAN_POINT ( 'NONE',  ( -57.71502896937850835, 217.3034525342667962, -4.350049139982195001 ) ) ;
#15574 = CARTESIAN_POINT ( 'NONE',  ( 15.24356964375000167, 246.6343750006145115, 3.323476615752272600 ) ) ;
#15575 =( NAMED_UNIT ( * ) PLANE_ANGLE_UNIT ( ) SI_UNIT ( $, .RADIAN. ) );
#15576 = CIRCLE ( 'NONE', #30110, 3.500000000000002665 ) ;
#15577 = CARTESIAN_POINT ( 'NONE',  ( -13.49999999999998401, 199.2875000012290627, 23.38268590217985476 ) ) ;
#15578 = CARTESIAN_POINT ( 'NONE',  ( -44.45461230271183695, 208.6787018382582346, -4.469044688360757966 ) ) ;
#15579 = CARTESIAN_POINT ( 'NONE',  ( 4.622313124798573369, 129.4351862821014549, 11.61527771782819940 ) ) ;
#15580 = CARTESIAN_POINT ( 'NONE',  ( 37.48975345065418452, 7.646167579472015790E-16, 166.8418166788690655 ) ) ;
#15581 = VERTEX_POINT ( 'NONE', #32146 ) ;
#15582 = CARTESIAN_POINT ( 'NONE',  ( 20.99999999999998579, 248.5374999999999659, -5.999999999999997335 ) ) ;
#15583 = CARTESIAN_POINT ( 'NONE',  ( 15.53471296425188797, 11.37731371789854506, 2.908627838312457747 ) ) ;
#15584 = CARTESIAN_POINT ( 'NONE',  ( -47.43080436395489841, 201.5000000000000000, -0.1155267958017054536 ) ) ;
#15585 = CARTESIAN_POINT ( 'NONE',  ( 5.233372021372432847, 119.9476862821014294, 8.152565276336710909 ) ) ;
#15586 =( BOUNDED_CURVE ( )  B_SPLINE_CURVE ( 2, ( #21643, #18051, #15390, #33196, #26747, #7237, #779, #26937, #7424 ),
 .UNSPECIFIED., .F., .F. ) 
 B_SPLINE_CURVE_WITH_KNOTS ( ( 3, 2, 2, 2, 3 ),
 ( 0.6041666666666667407, 0.6111111111111111605, 0.6250000000000000000, 0.6388888888888888395, 0.6458333333333333703 ),
 .UNSPECIFIED. ) 
 CURVE ( )  GEOMETRIC_REPRESENTATION_ITEM ( )  RATIONAL_B_SPLINE_CURVE ( ( 0.9330127018922192983, 0.9330127018922198534, 1.000000000000000000, 0.8660254037844387076, 1.000000000000000000, 0.8660254037844387076, 1.000000000000000000, 0.9330127018922187432, 0.9330127018922192983 ) ) 
 REPRESENTATION_ITEM ( '' )  );
#15587 = CARTESIAN_POINT ( 'NONE',  ( 20.99999999999995381, 241.5625000000000000, 5.999999999999998224 ) ) ;
#15588 = CARTESIAN_POINT ( 'NONE',  ( 4.622313124798573369, 37.43518628210144783, 11.61527771782819940 ) ) ;
#15589 = CARTESIAN_POINT ( 'NONE',  ( 22.56230152254411792, 7.347880794884125653E-16, -6.075000000000052580 ) ) ;
#15590 = VERTEX_POINT ( 'NONE', #14537 ) ;
#15591 = SURFACE_STYLE_USAGE ( .BOTH. , #20909 ) ;
#15592 = CARTESIAN_POINT ( 'NONE',  ( -10.83675517735155047, 124.2601862821014578, -11.08355503943142750 ) ) ;
#15593 = FACE_OUTER_BOUND ( 'NONE', #3190, .T. ) ;
#15594 = CARTESIAN_POINT ( 'NONE',  ( 1.715153634034233487, 10.12268628210144428, 9.534712964251941258 ) ) ;
#15595 = CARTESIAN_POINT ( 'NONE',  ( 27.24356964374999635, 197.8156250006145171, -15.72908226750539029 ) ) ;
#15596 = CYLINDRICAL_SURFACE ( 'NONE', #27454, 5.999999999999998224 ) ;
#15597 = CARTESIAN_POINT ( 'NONE',  ( -20.68320088531713452, 194.9994763905949924, -17.35526436380663284 ) ) ;
#15598 = CARTESIAN_POINT ( 'NONE',  ( 36.98482634954957859, 7.347880794884125653E-16, 163.8651217518988688 ) ) ;
#15599 = CARTESIAN_POINT ( 'NONE',  ( 15.20137627347641285, 1.191849618220900631, -7.999999999999998224 ) ) ;
#15600 = CYLINDRICAL_SURFACE ( 'NONE', #23628, 5.999999999999994671 ) ;
#15601 = CARTESIAN_POINT ( 'NONE',  ( -0.1745138560723084320, 82.38981371789856212, -9.500000000000005329 ) ) ;
#15602 = VERTEX_POINT ( 'NONE', #492 ) ;
#15603 = CARTESIAN_POINT ( 'NONE',  ( 21.00000000000000000, 244.9937500012290741, -6.928203230275506996 ) ) ;
#15604 = CARTESIAN_POINT ( 'NONE',  ( 12.50000000000000355, 75.48981371789855643, -0.1745138560722771515 ) ) ;
#15605 = CARTESIAN_POINT ( 'NONE',  ( 13.44051670066910908, 5.407089921784862696, -4.321874999385522109 ) ) ;
#15606 = CARTESIAN_POINT ( 'NONE',  ( 20.99999999999999289, 242.6875000000000000, -5.999999999999997335 ) ) ;
#15607 = CARTESIAN_POINT ( 'NONE',  ( 26.75643035624999655, -3.323476615752267715, -3.665624999385485694 ) ) ;
#15608 = CARTESIAN_POINT ( 'NONE',  ( -10.49813415416004858, 42.42731371789855643, 7.228626920338839135 ) ) ;
#15609 =( BOUNDED_CURVE ( )  B_SPLINE_CURVE ( 2, ( #17537, #2928, #16976, #28519, #11645, #20567, #23403 ),
 .UNSPECIFIED., .F., .F. ) 
 B_SPLINE_CURVE_WITH_KNOTS ( ( 3, 2, 2, 3 ),
 ( 0.04347826086956579211, 0.05072463768116009658, 0.05797101449275439411, 0.06521739130434869858 ),
 .UNSPECIFIED. ) 
 CURVE ( )  GEOMETRIC_REPRESENTATION_ITEM ( )  RATIONAL_B_SPLINE_CURVE ( ( 0.9999999999999893419, 0.8660254037844493658, 1.000000000000000000, 0.8660254037844387076, 1.000000000000000000, 0.8660254037844226094, 1.000000000000016209 ) ) 
 REPRESENTATION_ITEM ( '' )  );
#15610 = VERTEX_POINT ( 'NONE', #26271 ) ;
#15611 = CARTESIAN_POINT ( 'NONE',  ( 15.24356964374999990, 0.000000000000000000, -7.340624999385481075 ) ) ;
#15612 = CARTESIAN_POINT ( 'NONE',  ( 21.00000000000000000, 244.2343750006145626, -6.646953231504538984 ) ) ;
#15613 = CARTESIAN_POINT ( 'NONE',  ( 0.1745138560725515708, 15.01018628210143468, -12.50000000000000355 ) ) ;
#15614 = EDGE_CURVE ( 'NONE', #25852, #34104, #5387, .T. ) ;
#15615 = CARTESIAN_POINT ( 'NONE',  ( -42.47544563604516554, 214.8429017333602360, 4.673758765035156415 ) ) ;
#15616 = CARTESIAN_POINT ( 'NONE',  ( -59.10044563604516554, 205.1570982666397072, -4.673758765035155527 ) ) ;
#15617 =( NAMED_UNIT ( * ) PLANE_ANGLE_UNIT ( ) SI_UNIT ( $, .RADIAN. ) );
#15618 = CARTESIAN_POINT ( 'NONE',  ( 33.64652983760650073, -5.196152422706629359, 160.1293577552730483 ) ) ;
#15619 = CARTESIAN_POINT ( 'NONE',  ( 11.48171059495408208, 84.11481371789855643, -4.944772684328420986 ) ) ;
#15620 = CARTESIAN_POINT ( 'NONE',  ( -46.04538769728823411, 211.3212981617418222, -4.469044688360751749 ) ) ;
#15621 = CARTESIAN_POINT ( 'NONE',  ( -37.33705436395491262, 203.8621396198270475, -6.307003348497942419 ) ) ;
#15622 = EDGE_CURVE ( 'NONE', #32805, #13180, #17760, .T. ) ;
#15623 = CARTESIAN_POINT ( 'NONE',  ( 26.75643035624999655, 3.323476615752271268, -6.740624999385493865 ) ) ;
#15624 = DIRECTION ( 'NONE',  ( 0.000000000000000000, 0.000000000000000000, 1.000000000000000000 ) ) ;
#15625 = CARTESIAN_POINT ( 'NONE',  ( -10.83675517735179028, 51.33981371789855785, 11.08355503943118947 ) ) ;
#15626 = CARTESIAN_POINT ( 'NONE',  ( -46.43377896937850835, 207.8379586601372750, 8.530955311639258909 ) ) ;
#15627 = CARTESIAN_POINT ( 'NONE',  ( -7.234628195640302017, 198.2924038105676630, 27.00000000000000711 ) ) ;
#15628 = CARTESIAN_POINT ( 'NONE',  ( 11.48171059495397728, 91.48518628210145209, 4.944772684328674117 ) ) ;
#15629 = CARTESIAN_POINT ( 'NONE',  ( -15.46528703574804986, 22.19768628210144001, -3.257655550457287497 ) ) ;
#15630 = ADVANCED_FACE ( 'NONE', ( #14908 ), #17391, .F. ) ;
#15631 = PLANE ( 'NONE',  #9590 ) ;
#15632 = LINE ( 'NONE', #18109, #12536 ) ;
#15633 = ORIENTED_EDGE ( 'NONE', *, *, #16918, .F. ) ;
#15634 = AXIS2_PLACEMENT_3D ( 'NONE', #30524, #33731, #36562 ) ;
#15635 = CARTESIAN_POINT ( 'NONE',  ( -2.908627838312119351, 42.32268628210145067, -15.53471296425195369 ) ) ;
#15636 = CARTESIAN_POINT ( 'NONE',  ( -13.62178482187500528, 197.9281250006145569, -23.59362340125807123 ) ) ;
#15637 = ADVANCED_FACE ( 'NONE', ( #32520 ), #32337, .F. ) ;
#15638 = DIRECTION ( 'NONE',  ( 0.000000000000000000, 0.000000000000000000, 1.000000000000000000 ) ) ;
#15639 = CARTESIAN_POINT ( 'NONE',  ( 24.66770419336863185, 0.000000000000000000, 160.7643302352881278 ) ) ;
#15640 = CARTESIAN_POINT ( 'NONE',  ( -38.72247103062156981, 206.6499508600178672, 5.571401726697986057 ) ) ;
#15641 = CARTESIAN_POINT ( 'NONE',  ( 24.99999999999998934, 2.343145750507540814, 49.65004534589634488 ) ) ;
#15642 = CARTESIAN_POINT ( 'NONE',  ( -8.715434833791929847, 23.06018628210145138, -8.962234695871762469 ) ) ;
#15643 = CARTESIAN_POINT ( 'NONE',  ( 15.24356964375000167, 249.4468750006145399, 3.323476615752272600 ) ) ;
#15644 = CARTESIAN_POINT ( 'NONE',  ( 3.474262827703532341, 138.1648137178985678, -8.843639120294245259 ) ) ;
#15645 = CARTESIAN_POINT ( 'NONE',  ( 15.24356964374999990, 244.8718750006145797, -3.323476615752268604 ) ) ;
#15646 = ORIENTED_EDGE ( 'NONE', *, *, #16439, .T. ) ;
#15647 = CARTESIAN_POINT ( 'NONE',  ( 26.99999999999999645, 3.464101615137755275, -6.487500000000020250 ) ) ;
#15648 =( BOUNDED_CURVE ( )  B_SPLINE_CURVE ( 2, ( #11620, #17322, #34743, #17509, #20358, #28494, #3089, #2537, #11069 ),
 .UNSPECIFIED., .F., .F. ) 
 B_SPLINE_CURVE_WITH_KNOTS ( ( 3, 2, 2, 2, 3 ),
 ( 0.4375000000000000000, 0.4444444444444444198, 0.4583333333333333148, 0.4722222222222222099, 0.4791666666666666852 ),
 .UNSPECIFIED. ) 
 CURVE ( )  GEOMETRIC_REPRESENTATION_ITEM ( )  RATIONAL_B_SPLINE_CURVE ( ( 0.9330127018922194093, 0.9330127018922194093, 1.000000000000000000, 0.8660254037844387076, 1.000000000000000000, 0.8660254037844387076, 1.000000000000000000, 0.9330127018922190762, 0.9330127018922194093 ) ) 
 REPRESENTATION_ITEM ( '' )  );
#15649 = LINE ( 'NONE', #27197, #27490 ) ;
#15650 = CARTESIAN_POINT ( 'NONE',  ( 12.46528703574811558, 130.4023137178985792, -2.660918448318005947 ) ) ;
#15651 = CARTESIAN_POINT ( 'NONE',  ( 22.80587116629410360, 3.604726614523238837, -7.078124999385530636 ) ) ;
#15652 = CARTESIAN_POINT ( 'NONE',  ( 31.10325711637897328, -7.209453229046475009, 165.4807572684663342 ) ) ;
#15653 = CARTESIAN_POINT ( 'NONE',  ( 22.56230152254289578, -3.464101615138448054, -2.399999998770984799 ) ) ;
#15654 = CARTESIAN_POINT ( 'NONE',  ( -27.00000000000000355, 199.0999999999999943, 0.000000000000000000 ) ) ;
#15655 = EDGE_LOOP ( 'NONE', ( #6072, #2294, #1188 ) ) ;
#15656 = CARTESIAN_POINT ( 'NONE',  ( -10.49813415415989404, 50.37268628210145494, -7.228626920339069173 ) ) ;
#15657 = EDGE_LOOP ( 'NONE', ( #17287, #5740, #33747, #4630, #31255, #3547, #28055 ) ) ;
#15658 = VECTOR ( 'NONE', #35527, 1000.000000000000000 ) ;
#15659 = ORIENTED_EDGE ( 'NONE', *, *, #33716, .T. ) ;
#15660 = DIRECTION ( 'NONE',  ( 0.000000000000000000, 0.000000000000000000, 1.000000000000000000 ) ) ;
#15661 = DIRECTION ( 'NONE',  ( -1.000000000000000000, 0.000000000000000000, 0.000000000000000000 ) ) ;
#15662 = CARTESIAN_POINT ( 'NONE',  ( -27.00000000000000355, 199.2125000012290457, 0.000000000000000000 ) ) ;
#15663 = CARTESIAN_POINT ( 'NONE',  ( 15.24356964374999990, 3.323476615752268604, -9.628124999385486049 ) ) ;
#15664 = CARTESIAN_POINT ( 'NONE',  ( 8.715434833791931624, 73.66018628210144925, 8.962234695871760692 ) ) ;
#15665 = CARTESIAN_POINT ( 'NONE',  ( -5.770363421894122880, 13.96481371789853831, 14.38691631536194393 ) ) ;
#15666 = CARTESIAN_POINT ( 'NONE',  ( 0.000000000000000000, 200.0000000000000000, -27.00000000000000355 ) ) ;
#15667 = CARTESIAN_POINT ( 'NONE',  ( 14.06021656787942753, 216.9397834321235621, 0.8200469388724418440 ) ) ;
#15668 = CARTESIAN_POINT ( 'NONE',  ( -50.98586230271183695, 207.8500491399821613, 3.954877714930852495 ) ) ;
#15669 = DIRECTION ( 'NONE',  ( 0.9961946980917462113, 0.000000000000000000, -0.08715574274765178209 ) ) ;
#15670 = CARTESIAN_POINT ( 'NONE',  ( 28.29034631613303929, -5.196152422706632912, 167.7501794356626306 ) ) ;
#15671 = CARTESIAN_POINT ( 'NONE',  ( 8.710071997420211432, 10.51481371789855679, -3.796722387233181895 ) ) ;
#15672 = ADVANCED_FACE ( 'NONE', ( #6564 ), #35360, .T. ) ;
#15673 = CARTESIAN_POINT ( 'NONE',  ( -45.45163769728822700, 215.6869285224996986, -3.149950860017881382 ) ) ;
#15674 = CARTESIAN_POINT ( 'NONE',  ( -64.25372103062157692, 218.5309553116391896, -2.162041339862839084 ) ) ;
#15675 = EDGE_CURVE ( 'NONE', #2680, #37220, #19414, .T. ) ;
#15676 = ITEM_DEFINED_TRANSFORMATION ( 'NONE', 'NONE', #11761,  #17215 ) ;
#15677 = CARTESIAN_POINT ( 'NONE',  ( 5.778771075727756162E-15, 197.6656250006145399, 31.45816453501075927 ) ) ;
#15678 = CARTESIAN_POINT ( 'NONE',  ( -0.1745138560722442889, 109.9898137178985706, -15.50000000000000533 ) ) ;
#15679 = CARTESIAN_POINT ( 'NONE',  ( -42.07961230271182984, 211.8571965466040297, 6.469044688360755302 ) ) ;
#15680 = EDGE_CURVE ( 'NONE', #13498, #17027, #17028, .T. ) ;
#15681 = ORIENTED_EDGE ( 'NONE', *, *, #36955, .F. ) ;
#15682 = CARTESIAN_POINT ( 'NONE',  ( -11.61527771782819940, 21.33518628210144641, 4.622313124798574258 ) ) ;
#15683 = CARTESIAN_POINT ( 'NONE',  ( -89.83814373643217266, 60.44923248139874516, -5.000000000000000000 ) ) ;
#15684 = CARTESIAN_POINT ( 'NONE',  ( 37.30839204460733782, 7.347880794884117764E-16, 167.5634945697888440 ) ) ;
#15685 = CARTESIAN_POINT ( 'NONE',  ( 37.36719068741531657, 7.646167579472024665E-16, 165.4409178846775603 ) ) ;
#15686 = CARTESIAN_POINT ( 'NONE',  ( -13.04141134922759804, 105.5726862821014294, -8.927990412390657937 ) ) ;
#15687 = CARTESIAN_POINT ( 'NONE',  ( -49.80580436395490551, 216.5000000000000000, 0.1155267958017343610 ) ) ;
#15688 = EDGE_CURVE ( 'NONE', #33455, #6605, #18247, .T. ) ;
#15689 = CARTESIAN_POINT ( 'NONE',  ( 22.80587116629411426, 3.604726614523238837, -3.928124999385561367 ) ) ;
#15690 = CARTESIAN_POINT ( 'NONE',  ( -2.064181346179269738, 38.29768628210144499, 9.465287035748067623 ) ) ;
#15691 = DIRECTION ( 'NONE',  ( 0.08715574274765150453, 0.000000000000000000, 0.9961946980917461003 ) ) ;
#15692 = CARTESIAN_POINT ( 'NONE',  ( -37.73288769728823411, 201.5309553116392181, -2.393094931466246855 ) ) ;
#15693 = CARTESIAN_POINT ( 'NONE',  ( 36.71028575989448228, 7.347880794884125653E-16, 160.7271084529098744 ) ) ;
#15694 = CARTESIAN_POINT ( 'NONE',  ( 2.660918448318279950, 79.69768628210144357, -12.46528703574805697 ) ) ;
#15695 = CARTESIAN_POINT ( 'NONE',  ( 27.00000000000000355, 199.7750000000000057, -3.306546357697854128E-15 ) ) ;
#15696 = LINE ( 'NONE', #3741, #28661 ) ;
#15698 = ORIENTED_EDGE ( 'NONE', *, *, #19610, .F. ) ;
#15697 = CARTESIAN_POINT ( 'NONE',  ( -6.594114490232312775, 50.66018628210144925, -6.840914352312096547 ) ) ;
#15699 = LINE ( 'NONE', #27250, #33605 ) ;
#15700 = ORIENTED_EDGE ( 'NONE', *, *, #2267, .T. ) ;
#15701 = CARTESIAN_POINT ( 'NONE',  ( 21.00000000000000000, -6.928203230275506996, -0.7875000000000005329 ) ) ;
#15702 = CARTESIAN_POINT ( 'NONE',  ( -1.045839947578415010E-13, 195.7250000012290343, 27.00000000000000355 ) ) ;
#15703 = CARTESIAN_POINT ( 'NONE',  ( 33.95006120609467359, 5.407089921784862696, 162.2014130487530110 ) ) ;
#15704 = CARTESIAN_POINT ( 'NONE',  ( 33.75438506914960612, -5.196152422706635576, 161.3621486929372111 ) ) ;
#15705 = CARTESIAN_POINT ( 'NONE',  ( 15.00000000000000000, 245.9125000000000227, -3.464101615137752166 ) ) ;
#15706 = CARTESIAN_POINT ( 'NONE',  ( -13.62178482187500528, 195.2281250006145399, -23.59362340125807123 ) ) ;
#15707 = CARTESIAN_POINT ( 'NONE',  ( 12.53471296425189330, 94.17731371789857064, 2.311890736173451977 ) ) ;
#15708 = CARTESIAN_POINT ( 'NONE',  ( -6.932735513423968321, 106.1476862821014606, -10.69584247140445221 ) ) ;
#15709 = ORIENTED_EDGE ( 'NONE', *, *, #21328, .F. ) ;
#15710 = ORIENTED_EDGE ( 'NONE', *, *, #29602, .F. ) ;
#15711 = CARTESIAN_POINT ( 'NONE',  ( -26.99999999999998934, 197.9000000012290172, 15.58845726811991561 ) ) ;
#15712 = CARTESIAN_POINT ( 'NONE',  ( -47.00000000000000711, 237.0000000000000000, 5.000000000000000000 ) ) ;
#15713 = CARTESIAN_POINT ( 'NONE',  ( -3.257655550456946880, 72.90231371789855075, -15.46528703574811736 ) ) ;
#15714 = CARTESIAN_POINT ( 'NONE',  ( 21.00000000000000000, 6.646953231504538984, -6.665624999385467930 ) ) ;
#15715 = CARTESIAN_POINT ( 'NONE',  ( 26.75643035624999655, 244.2718750006145001, -3.323476615752271712 ) ) ;
#15716 = CARTESIAN_POINT ( 'NONE',  ( -3.796722387233375073, 93.78518628210144925, 8.710071997420127943 ) ) ;
#15717 = CARTESIAN_POINT ( 'NONE',  ( 0.000000000000000000, 141.0000000000000000, 0.000000000000000000 ) ) ;
#15718 = EDGE_CURVE ( 'NONE', #19052, #37126, #6953, .T. ) ;
#15719 = CARTESIAN_POINT ( 'NONE',  ( -6.594114490232462877, 51.33981371789855785, 6.840914352311949109 ) ) ;
#15720 = CARTESIAN_POINT ( 'NONE',  ( 10.31873187879411091, -3.604726614523240613, -8.653124999385532590 ) ) ;
#15721 = CARTESIAN_POINT ( 'NONE',  ( 6.594114490232462877, 111.1398137178985621, -6.840914352311949109 ) ) ;
#15722 = CARTESIAN_POINT ( 'NONE',  ( 26.99999999999999645, 198.0125000000000739, -15.58845726811990495 ) ) ;
#15723 = CARTESIAN_POINT ( 'NONE',  ( 8.962234695871567070, 21.43981371789854862, 8.715434833792127023 ) ) ;
#15724 = CARTESIAN_POINT ( 'NONE',  ( -10.49813415415989581, 87.17268628210143788, -7.228626920339068285 ) ) ;
#15725 = CARTESIAN_POINT ( 'NONE',  ( 16.56230152254410726, -6.928203230275506996, -6.074999998771025034 ) ) ;
#15726 = DIRECTION ( 'NONE',  ( 1.000000000000000000, 0.000000000000000000, 1.636531581110199847E-16 ) ) ;
#15727 = CARTESIAN_POINT ( 'NONE',  ( 37.21521286099908110, 7.646167579472015790E-16, 163.7038033798800711 ) ) ;
#15728 = CARTESIAN_POINT ( 'NONE',  ( 16.56230152254411436, -7.209453229046482114, -4.584374999385491201 ) ) ;
#15729 = CARTESIAN_POINT ( 'NONE',  ( -13.49999999999998401, 197.8249999999999886, 23.38268590217985476 ) ) ;
#15730 = FACE_OUTER_BOUND ( 'NONE', #28677, .T. ) ;
#15731 = FACE_OUTER_BOUND ( 'NONE', #32238, .T. ) ;
#15732 = CARTESIAN_POINT ( 'NONE',  ( -7.954856959092191815, 96.37268628210144072, -5.529263428287477744 ) ) ;
#15733 = CARTESIAN_POINT ( 'NONE',  ( 25.01079625726091749, 203.5081962293401148, 3.000000000000000000 ) ) ;
#15734 = CARTESIAN_POINT ( 'NONE',  ( 12.50000000000000355, 136.9101862821014777, 0.1745138560725507937 ) ) ;
#15735 = CARTESIAN_POINT ( 'NONE',  ( -6.589905998207248317, 143.0000000000000284, 10.14935392281090287 ) ) ;
#15736 = CARTESIAN_POINT ( 'NONE',  ( 21.00000000000000000, 248.8468750006145456, -6.646953231504538984 ) ) ;
#15737 = ORIENTED_EDGE ( 'NONE', *, *, #11097, .F. ) ;
#15738 = CARTESIAN_POINT ( 'NONE',  ( 28.02930337212723089, -5.407089921784859143, 166.1637690562780278 ) ) ;
#15739 = CARTESIAN_POINT ( 'NONE',  ( 23.87821517812500005, -4.985214923628404016, -3.590624999385477523 ) ) ;
#15740 = CARTESIAN_POINT ( 'NONE',  ( 13.62178482187499640, 199.2593750006145399, -23.59362340125807123 ) ) ;
#15741 = CARTESIAN_POINT ( 'NONE',  ( 24.90318630322867932, -4.417295604025225586, -7.999999999999998224 ) ) ;
#15742 = CARTESIAN_POINT ( 'NONE',  ( 34.34268633269625326, -5.196152422706635576, 168.0864629050564929 ) ) ;
#15743 = CARTESIAN_POINT ( 'NONE',  ( 3.253724281355069334E-15, 199.5500000012290513, -27.00000000000000000 ) ) ;
#15744 = CARTESIAN_POINT ( 'NONE',  ( 21.00000000000000000, 242.9968750006145228, -6.646953231504538984 ) ) ;
#15745 = CARTESIAN_POINT ( 'NONE',  ( 22.80587116629410716, 3.604726614523238837, -0.3281249993855308578 ) ) ;
#15746 = CARTESIAN_POINT ( 'NONE',  ( 3.474262827703532341, 18.56481371789855928, -8.843639120294245259 ) ) ;
#15747 = CARTESIAN_POINT ( 'NONE',  ( 27.24356964374999279, 198.3218750006145399, -15.72908226750539207 ) ) ;
#15748 = AXIS2_PLACEMENT_3D ( 'NONE', #11609, #20347, #8585 ) ;
#15750 = ORIENTED_EDGE ( 'NONE', *, *, #29030, .T. ) ;
#15749 = ORIENTED_EDGE ( 'NONE', *, *, #13033, .T. ) ;
#15751 = CARTESIAN_POINT ( 'NONE',  ( 21.00000000000000000, 245.8093750006144944, 6.646953231504538984 ) ) ;
#15752 = CARTESIAN_POINT ( 'NONE',  ( -0.1745138560722763466, 27.18981371789855217, -12.50000000000000355 ) ) ;
#15753 = CARTESIAN_POINT ( 'NONE',  ( 21.00000000000000000, -6.646953231504538984, -0.9281249993854503444 ) ) ;
#15754 = CARTESIAN_POINT ( 'NONE',  ( -8.927990412390371944, 127.5273137178985792, -13.04141134922778988 ) ) ;
#15755 = EDGE_CURVE ( 'NONE', #23005, #36021, #31299, .T. ) ;
#15756 = CARTESIAN_POINT ( 'NONE',  ( 21.00000000000000000, -6.928203230275506996, -8.831249998770948295 ) ) ;
#15757 = VERTEX_POINT ( 'NONE', #15853 ) ;
#15758 = CARTESIAN_POINT ( 'NONE',  ( 19.68408634441912142, -5.407089921784861808, -7.246874999385532590 ) ) ;
#15759 = EDGE_CURVE ( 'NONE', #24412, #35079, #3715, .T. ) ;
#15760 = VERTEX_POINT ( 'NONE', #21173 ) ;
#15761 = CARTESIAN_POINT ( 'NONE',  ( -13.62178482187500528, 197.4781250006145399, -23.59362340125807123 ) ) ;
#15762 = CIRCLE ( 'NONE', #19975, 3.500000000000002220 ) ;
#15763 = CARTESIAN_POINT ( 'NONE',  ( 11.48171059495397728, 137.4851862821014663, 4.944772684328674117 ) ) ;
#15764 = CARTESIAN_POINT ( 'NONE',  ( 34.09386818162830224, -5.407089921784861808, 163.8451343006043999 ) ) ;
#15765 = EDGE_CURVE ( 'NONE', #12608, #31196, #1072, .T. ) ;
#15766 = CARTESIAN_POINT ( 'NONE',  ( -54.35044563604515844, 203.6929966515019430, -6.137860380172892150 ) ) ;
#15767 = CARTESIAN_POINT ( 'NONE',  ( 26.75643035624999655, 246.8593750006145342, -3.323476615752271268 ) ) ;
#15768 = CARTESIAN_POINT ( 'NONE',  ( 0.000000000000000000, 0.000000000000000000, 0.000000000000000000 ) ) ;
#15769 = CARTESIAN_POINT ( 'NONE',  ( -27.00000000000000355, 199.1750000012290513, -15.58845726811989429 ) ) ;
#15770 = CARTESIAN_POINT ( 'NONE',  ( -46.43377896937850835, 208.9097554298617183, 4.530955311639234040 ) ) ;
#15771 = CARTESIAN_POINT ( 'NONE',  ( -2.311890736173176641, 134.3226862821014436, -12.53471296425194836 ) ) ;
#15772 = CARTESIAN_POINT ( 'NONE',  ( 28.01623001071507701, 5.407089921784856479, 166.0143398515642730 ) ) ;
#15773 = ORIENTED_EDGE ( 'NONE', *, *, #32719, .F. ) ;
#15774 = CARTESIAN_POINT ( 'NONE',  ( 7.234628195640363302, 195.4799038117967029, -26.99999999999996803 ) ) ;
#15775 = AXIS2_PLACEMENT_3D ( 'NONE', #36230, #10089, #21846 ) ;
#15776 = CARTESIAN_POINT ( 'NONE',  ( 10.83675517735155225, 138.0601862821014549, 11.08355503943142573 ) ) ;
#15777 = CARTESIAN_POINT ( 'NONE',  ( -49.01413769728823411, 214.1499508600179240, 7.418979330068584233 ) ) ;
#15778 = CARTESIAN_POINT ( 'NONE',  ( -8.152565276336710909, 113.0476862821014663, 5.233372021372435512 ) ) ;
#15779 = CARTESIAN_POINT ( 'NONE',  ( 18.00000000000000000, 241.3750000000000000, -5.196152422706630247 ) ) ;
#15780 = CARTESIAN_POINT ( 'NONE',  ( 8.962234695871762469, 25.36018628210144499, -8.715434833791931624 ) ) ;
#15781 = CARTESIAN_POINT ( 'NONE',  ( 16.56230152254411081, -6.928203230275514990, -6.637500000000041034 ) ) ;
#15782 = UNCERTAINTY_MEASURE_WITH_UNIT (LENGTH_MEASURE( 1.000000000000000082E-05 ), #10665, 'distance_accuracy_value', 'NONE');
#15783 = ORIENTED_EDGE ( 'NONE', *, *, #24836, .T. ) ;
#15784 = CARTESIAN_POINT ( 'NONE',  ( -35.35788769728823411, 216.4690446883607535, 1.857196546604031662 ) ) ;
#15785 = CARTESIAN_POINT ( 'NONE',  ( 13.23911966647218996, 126.8476862821014635, -8.632099005475504683 ) ) ;
#15786 = FACE_OUTER_BOUND ( 'NONE', #15225, .T. ) ;
#15787 = CARTESIAN_POINT ( 'NONE',  ( -7.954856959092309943, 143.6273137178985451, 5.529263428287300108 ) ) ;
#15788 = CARTESIAN_POINT ( 'NONE',  ( 5.778771075727756162E-15, 198.5656250006145171, 31.45816453501075927 ) ) ;
#15789 = CARTESIAN_POINT ( 'NONE',  ( 15.00000000000000000, 0.000000000000000000, -5.849999999999994316 ) ) ;
#15790 = CARTESIAN_POINT ( 'NONE',  ( 13.49999999999999645, 195.8000000000000114, -23.38268590217984766 ) ) ;
#15791 = CARTESIAN_POINT ( 'NONE',  ( 22.56230152254247301, 3.464101615138709178, -5.587500000000009237 ) ) ;
#15792 = CARTESIAN_POINT ( 'NONE',  ( 30.74292259240310443, 6.928203230275514990, 161.3621148129311109 ) ) ;
#15793 = CARTESIAN_POINT ( 'NONE',  ( -5.233372021372612259, 69.45231371789853370, 8.152565276336593669 ) ) ;
#15794 = ORIENTED_EDGE ( 'NONE', *, *, #19765, .F. ) ;
#15795 = CARTESIAN_POINT ( 'NONE',  ( 26.99999999999999645, 244.8812500012290343, -7.347880794884117764E-16 ) ) ;
#15796 = CARTESIAN_POINT ( 'NONE',  ( -12.46528703574811558, 79.80231371789855643, 2.660918448318004170 ) ) ;
#15797 = CARTESIAN_POINT ( 'NONE',  ( 10.31873187879410558, 3.604726614523240613, -4.734374999385511984 ) ) ;
#15798 = CARTESIAN_POINT ( 'NONE',  ( -6.543039160116403075, 143.0000000000000284, 10.81689977700826866 ) ) ;
#15799 = CARTESIAN_POINT ( 'NONE',  ( 15.24356964374999990, 3.323476615752268604, -5.240624999385486760 ) ) ;
#15800 = CARTESIAN_POINT ( 'NONE',  ( 4.622313124798831829, 55.36481371789855643, -11.61527771782809282 ) ) ;
#15801 = ORIENTED_EDGE ( 'NONE', *, *, #8322, .T. ) ;
#15802 = DIRECTION ( 'NONE',  ( -0.000000000000000000, 1.000000000000000000, -0.000000000000000000 ) ) ;
#15803 = CARTESIAN_POINT ( 'NONE',  ( 21.00000000000000000, 243.7843750006144887, -6.646953231504538984 ) ) ;
#15804 = CARTESIAN_POINT ( 'NONE',  ( 8.962234695871762469, 16.16018628210144570, -8.715434833791931624 ) ) ;
#15805 = CARTESIAN_POINT ( 'NONE',  ( -35.74627896937850124, 203.4690446883607535, -1.626142955000504209 ) ) ;
#15806 = CARTESIAN_POINT ( 'NONE',  ( -50.19419563604517265, 203.5000000000000000, 0.1155267958017914542 ) ) ;
#15807 = SHAPE_REPRESENTATION_RELATIONSHIP ( 'NONE' , 'NONE' ,  #9842, #21035 ) ;
#15808 = CARTESIAN_POINT ( 'NONE',  ( 20.99999999999999645, 185.0294372515228645, 0.000000000000000000 ) ) ;
#15809 = CARTESIAN_POINT ( 'NONE',  ( -2.311890736173448424, 78.07731371789856212, 12.53471296425189330 ) ) ;
#15810 = CARTESIAN_POINT ( 'NONE',  ( -49.80580436395490551, 214.5000000000000284, 0.1155267958017899832 ) ) ;
#15811 =( BOUNDED_CURVE ( )  B_SPLINE_CURVE ( 2, ( #23372, #34922, #8966, #6110, #17692, #31522, #29231 ),
 .UNSPECIFIED., .F., .F. ) 
 B_SPLINE_CURVE_WITH_KNOTS ( ( 3, 2, 2, 3 ),
 ( 0.1086956521739126380, 0.1159420289855069286, 0.1231884057971012053, 0.1304347826086954820 ),
 .UNSPECIFIED. ) 
 CURVE ( )  GEOMETRIC_REPRESENTATION_ITEM ( )  RATIONAL_B_SPLINE_CURVE ( ( 1.000000000000007327, 0.8660254037844312691, 1.000000000000000000, 0.8660254037844387076, 1.000000000000000000, 0.8660254037844418162, 0.9999999999999968914 ) ) 
 REPRESENTATION_ITEM ( '' )  );
#15812 = CARTESIAN_POINT ( 'NONE',  ( -60.88913769728823411, 206.8500491399821044, -5.686928522499717253 ) ) ;
#15813 = CARTESIAN_POINT ( 'NONE',  ( 10.56230152254410903, 0.000000000000000000, -0.4500000000000614619 ) ) ;
#15814 = CARTESIAN_POINT ( 'NONE',  ( -6.092822981423666739, 63.41481371789855359, -14.25334919248795096 ) ) ;
#15815 = CARTESIAN_POINT ( 'NONE',  ( -49.79836230271183695, 202.5810206699313767, -4.149950860017804111 ) ) ;
#15816 = FACE_OUTER_BOUND ( 'NONE', #33, .T. ) ;
#15817 = CARTESIAN_POINT ( 'NONE',  ( 2.311890736173175753, 92.92268628210145209, 12.53471296425194836 ) ) ;
#15818 = CARTESIAN_POINT ( 'NONE',  ( 15.50000000000000533, 26.51018628210144001, 0.1745138560725827404 ) ) ;
#15819 = CARTESIAN_POINT ( 'NONE',  ( 20.99999999999999645, 185.0294372515228645, -5.999999999999999112 ) ) ;
#15820 = CARTESIAN_POINT ( 'NONE',  ( 20.99999999999999645, 0.000000000000000000, -8.000000000000000000 ) ) ;
#15821 = ORIENTED_EDGE ( 'NONE', *, *, #13589, .T. ) ;
#15822 = CARTESIAN_POINT ( 'NONE',  ( 10.83675517735155225, 46.06018628210144072, 11.08355503943142573 ) ) ;
#15823 = CARTESIAN_POINT ( 'NONE',  ( 13.62178482187499640, 196.9531250006145342, -23.59362340125807123 ) ) ;
#15824 = CARTESIAN_POINT ( 'NONE',  ( 0.3500000000000069722, 244.5000000000000000, -2.499999999999999556 ) ) ;
#15825 = DIRECTION ( 'NONE',  ( 0.000000000000000000, 0.000000000000000000, 1.000000000000000000 ) ) ;
#15826 = CARTESIAN_POINT ( 'NONE',  ( -34.76413769728823411, 213.1499508600178672, 5.686928522499718142 ) ) ;
#15827 = EDGE_CURVE ( 'NONE', #8395, #21882, #33932, .T. ) ;
#15828 = CARTESIAN_POINT ( 'NONE',  ( 1.120210788295102201E-13, 195.3875000000000455, -27.00000000000000711 ) ) ;
#15829 = CARTESIAN_POINT ( 'NONE',  ( -2.660918448318275509, 19.89768628210143575, 12.46528703574805874 ) ) ;
#15830 =( BOUNDED_CURVE ( )  B_SPLINE_CURVE ( 2, ( #30055, #18516, #19267, #4829, #4089, #21355, #22098 ),
 .UNSPECIFIED., .F., .F. ) 
 B_SPLINE_CURVE_WITH_KNOTS ( ( 3, 2, 2, 3 ),
 ( 0.1086956521739118053, 0.1159420289855061098, 0.1231884057971004143, 0.1304347826086947049 ),
 .UNSPECIFIED. ) 
 CURVE ( )  GEOMETRIC_REPRESENTATION_ITEM ( )  RATIONAL_B_SPLINE_CURVE ( ( 1.000000000000022871, 0.8660254037844159480, 1.000000000000000000, 0.8660254037844387076, 1.000000000000000000, 0.8660254037844561381, 0.9999999999999825695 ) ) 
 REPRESENTATION_ITEM ( '' )  );
#15831 = CARTESIAN_POINT ( 'NONE',  ( 18.12178482187500350, 249.0343750006145456, 4.985214923628407568 ) ) ;
#15832 = CARTESIAN_POINT ( 'NONE',  ( 8.152565276336593669, 131.5523137178985564, 5.233372021372610483 ) ) ;
#15833 = CARTESIAN_POINT ( 'NONE',  ( 15.24356964374999990, 244.4218750006145058, -3.323476615752268604 ) ) ;
#15834 = EDGE_LOOP ( 'NONE', ( #22330, #32816, #20344, #22835 ) ) ;
#15835 = DIRECTION ( 'NONE',  ( 0.000000000000000000, 0.000000000000000000, 1.000000000000000000 ) ) ;
#15836 = CARTESIAN_POINT ( 'NONE',  ( -4.944772684328424539, 127.8148137178985735, -11.48171059495408031 ) ) ;
#15837 = CARTESIAN_POINT ( 'NONE',  ( 13.44051670066910908, 5.407089921784856479, -7.865624999385534721 ) ) ;
#15838 = CARTESIAN_POINT ( 'NONE',  ( 24.83115269446006934, 3.604726614523236616, 165.4272033993090076 ) ) ;
#15839 = DIRECTION ( 'NONE',  ( 0.000000000000000000, 0.000000000000000000, 1.000000000000000000 ) ) ;
#15840 = CARTESIAN_POINT ( 'NONE',  ( 5.727106289114498080E-15, 196.5125000000000171, 31.17691453623979214 ) ) ;
#15841 = ORIENTED_EDGE ( 'NONE', *, *, #21063, .F. ) ;
#15842 = CARTESIAN_POINT ( 'NONE',  ( -4.944772684328673229, 38.58518628210144641, 11.48171059495397728 ) ) ;
#15843 = VERTEX_POINT ( 'NONE', #15286 ) ;
#15844 = ORIENTED_EDGE ( 'NONE', *, *, #5730, .T. ) ;
#15845 = DIRECTION ( 'NONE',  ( -0.000000000000000000, 1.000000000000000000, -0.000000000000000000 ) ) ;
#15846 = CARTESIAN_POINT ( 'NONE',  ( -6.000000000000000888, -20.00000000000000000, -19.99999999999999289 ) ) ;
#15847 = CARTESIAN_POINT ( 'NONE',  ( 20.99999999999999645, 249.2687500012290513, 5.999999999999998224 ) ) ;
#15848 = DIRECTION ( 'NONE',  ( 0.08715574274765150453, 0.000000000000000000, 0.9961946980917461003 ) ) ;
#15849 = CARTESIAN_POINT ( 'NONE',  ( 26.75643035624999655, -3.323476615752267715, -9.853124999385466154 ) ) ;
#15850 = VECTOR ( 'NONE', #3701, 1000.000000000000000 ) ;
#15851 = CARTESIAN_POINT ( 'NONE',  ( -12.50000000000000355, 77.11018628210145209, -0.1745138560725492671 ) ) ;
#15852 = CARTESIAN_POINT ( 'NONE',  ( 15.50000000000000533, 11.08981371789854897, -0.1745138560722452326 ) ) ;
#15853 = CARTESIAN_POINT ( 'NONE',  ( 25.22171936664797798, 0.000000000000000000, 169.8914008901326724 ) ) ;
#15854 = EDGE_CURVE ( 'NONE', #16407, #9264, #34942, .T. ) ;
#15855 = CARTESIAN_POINT ( 'NONE',  ( 15.90209636607598931, 223.5944096904600542, 3.170162721592977739 ) ) ;
#15856 = CARTESIAN_POINT ( 'NONE',  ( -54.15252896937849414, 207.6499508600178387, -3.839350919129087547 ) ) ;
#15857 = AXIS2_PLACEMENT_3D ( 'NONE', #23792, #466, #33069 ) ;
#15858 = CARTESIAN_POINT ( 'NONE',  ( 15.00000000000000000, 245.5000000000000000, 0.000000000000000000 ) ) ;
#15859 = CARTESIAN_POINT ( 'NONE',  ( 31.28219875076131018, -6.928203230275506996, 167.5260695085981411 ) ) ;
#15860 = CARTESIAN_POINT ( 'NONE',  ( -12.50000000000000355, 144.4898137178985564, 0.1745138560722786503 ) ) ;
#15861 = CARTESIAN_POINT ( 'NONE',  ( -42.08705436395489841, 205.3262412349647263, -4.842901733360204020 ) ) ;
#15862 = CARTESIAN_POINT ( 'NONE',  ( -58.90997103062156981, 217.3034525342668815, 4.350049139982096413 ) ) ;
#15863 = EDGE_CURVE ( 'NONE', #16407, #15581, #29871, .T. ) ;
#15865 = SHAPE_DEFINITION_REPRESENTATION ( #26507, #6520 ) ;
#15864 =( REPRESENTATION_RELATIONSHIP ('NONE','NONE', #4304, #10397 ) REPRESENTATION_RELATIONSHIP_WITH_TRANSFORMATION ( #28337 )SHAPE_REPRESENTATION_RELATIONSHIP( ) );
#15866 = FACE_OUTER_BOUND ( 'NONE', #11795, .T. ) ;
#15867 = CARTESIAN_POINT ( 'NONE',  ( 27.24356964374999635, 199.6156250006145285, -15.72908226750539029 ) ) ;
#15868 = CARTESIAN_POINT ( 'NONE',  ( -13.23911966647199812, 108.5523137178985422, -8.632099005475788900 ) ) ;
#15869 = CARTESIAN_POINT ( 'NONE',  ( -39.90252896937850124, 206.6499508600178387, -5.571401726697954970 ) ) ;
#15870 = ORIENTED_EDGE ( 'NONE', *, *, #31837, .F. ) ;
#15871 = CARTESIAN_POINT ( 'NONE',  ( -7.234628195640316228, 195.9700961906613372, -27.00000000000000000 ) ) ;
#15872 = CARTESIAN_POINT ( 'NONE',  ( -47.00000000000000711, 244.5000000000000000, 2.500000000000000000 ) ) ;
#15873 = CARTESIAN_POINT ( 'NONE',  ( 37.17435860658612512, 3.604726614523243278, 163.2368371151495694 ) ) ;
#15874 = CARTESIAN_POINT ( 'NONE',  ( 6.092822981423978490, 98.38518628210145778, -14.25334919248782306 ) ) ;
#15876 = CIRCLE ( 'NONE', #724, 2.649999999999985700 ) ;
#15875 =( BOUNDED_CURVE ( )  B_SPLINE_CURVE ( 2, ( #10644, #33774, #2112, #9900, #21484, #20309, #28267, #34140, #22594 ),
 .UNSPECIFIED., .F., .F. ) 
 B_SPLINE_CURVE_WITH_KNOTS ( ( 3, 2, 2, 2, 3 ),
 ( 0.2500000000000000000, 0.2536231884057971175, 0.2608695652173912971, 0.2681159420289855322, 0.2717391304347825942 ),
 .UNSPECIFIED. ) 
 CURVE ( )  GEOMETRIC_REPRESENTATION_ITEM ( )  RATIONAL_B_SPLINE_CURVE ( ( 0.9330127018922194093, 0.9330127018922190762, 1.000000000000000000, 0.8660254037844387076, 1.000000000000000000, 0.8660254037844387076, 1.000000000000000000, 0.9330127018922198534, 0.9330127018922191873 ) ) 
 REPRESENTATION_ITEM ( '' )  );
#15877 = CARTESIAN_POINT ( 'NONE',  ( -59.10788769728823411, 216.4690446883607535, 1.857196546604031662 ) ) ;
#15878 = CARTESIAN_POINT ( 'NONE',  ( 22.80587116629410360, 3.604726614523238837, -3.478124999385532767 ) ) ;
#15879 = CARTESIAN_POINT ( 'NONE',  ( 0.1745138560725194299, 42.61018628210144499, -9.500000000000005329 ) ) ;
#15880 = FACE_OUTER_BOUND ( 'NONE', #136, .T. ) ;
#15881 = CARTESIAN_POINT ( 'NONE',  ( -39.11830436395489841, 209.8844732041983150, 8.500000000000003553 ) ) ;
#15882 = DIRECTION ( 'NONE',  ( -1.000000000000000000, 0.000000000000000000, 0.000000000000000000 ) ) ;
#15883 = CARTESIAN_POINT ( 'NONE',  ( 10.49813415415989581, 82.57268628210145778, 7.228626920339068285 ) ) ;
#15884 = CARTESIAN_POINT ( 'NONE',  ( 13.49999999999999645, 199.4000000000000341, -23.38268590217984766 ) ) ;
#15885 = CARTESIAN_POINT ( 'NONE',  ( 15.00000000000000000, 0.000000000000000000, -4.443749998770951670 ) ) ;
#15887 = EDGE_LOOP ( 'NONE', ( #1025, #980, #13462, #33477 ) ) ;
#15886 = CARTESIAN_POINT ( 'NONE',  ( -5.233372021372430183, 41.74768628210143362, -8.152565276336710909 ) ) ;
#15888 = CARTESIAN_POINT ( 'NONE',  ( 20.99999999999999289, 241.7874999999999659, -5.999999999999997335 ) ) ;
#15889 = ORIENTED_EDGE ( 'NONE', *, *, #25804, .T. ) ;
#15890 = CARTESIAN_POINT ( 'NONE',  ( 26.99999999999999645, 7.347880794884117764E-16, -2.024999999999999023 ) ) ;
#15891 = CARTESIAN_POINT ( 'NONE',  ( -61.28497103062156981, 204.4285982733020148, -3.350049139982115509 ) ) ;
#15892 = CARTESIAN_POINT ( 'NONE',  ( 30.80420397407610622, 7.209453229046482114, 162.0625642106390956 ) ) ;
#15893 = CARTESIAN_POINT ( 'NONE',  ( 36.67433401601106624, 3.464101615137759271, 160.3161781399470271 ) ) ;
#15894 = CARTESIAN_POINT ( 'NONE',  ( 15.00000000000000178, 246.8874999999999886, 3.464101615137757051 ) ) ;
#15895 = CARTESIAN_POINT ( 'NONE',  ( 36.71028575989448228, 7.347880794884125653E-16, 160.7271084529098744 ) ) ;
#15896 = CARTESIAN_POINT ( 'NONE',  ( -11.61527771782809282, 89.86481371789855643, -4.622313124798832717 ) ) ;
#15897 = CARTESIAN_POINT ( 'NONE',  ( -12.46528703574805874, 104.9976862821014549, -2.660918448318280838 ) ) ;
#15898 = ORIENTED_EDGE ( 'NONE', *, *, #28459, .T. ) ;
#15899 = EDGE_LOOP ( 'NONE', ( #35215, #18022 ) ) ;
#15900 = CARTESIAN_POINT ( 'NONE',  ( 27.00000000000001066, 198.9500000012290570, 15.58845726811988897 ) ) ;
#15901 = CARTESIAN_POINT ( 'NONE',  ( 21.00000000000000355, 0.000000000000000000, 50.00000000000001421 ) ) ;
#15902 = EDGE_CURVE ( 'NONE', #20414, #32797, #14558, .T. ) ;
#15903 = CARTESIAN_POINT ( 'NONE',  ( -13.04141134922778456, 51.62731371789855928, 8.927990412390377273 ) ) ;
#15904 = CARTESIAN_POINT ( 'NONE',  ( 18.12178482187500350, -4.985214923628407568, -6.028124999385486404 ) ) ;
#15905 = CARTESIAN_POINT ( 'NONE',  ( 15.24356964374999990, 246.2593750006145399, 0.000000000000000000 ) ) ;
#15906 = CARTESIAN_POINT ( 'NONE',  ( -62.86830436395490551, 209.8844732041982297, 4.499999999999996447 ) ) ;
#15907 = ADVANCED_FACE ( 'NONE', ( #12628, #19454, #27780 ), #2553, .T. ) ;
#15908 = DIRECTION ( 'NONE',  ( 0.000000000000000000, -0.000000000000000000, 1.000000000000000000 ) ) ;
#15909 = CARTESIAN_POINT ( 'NONE',  ( 6.840914352311949109, 49.03981371789855359, 6.594114490232462877 ) ) ;
#15910 = CARTESIAN_POINT ( 'NONE',  ( 10.31873187879411091, -3.604726614523240613, -7.303124999385512517 ) ) ;
#15911 = CARTESIAN_POINT ( 'NONE',  ( -7.954856959092309943, 116.0273137178985792, 5.529263428287300108 ) ) ;
#15912 = CARTESIAN_POINT ( 'NONE',  ( 18.12178482187499640, 239.7718750006145001, -4.985214923628404904 ) ) ;
#15913 = CARTESIAN_POINT ( 'NONE',  ( -7.228626920338836470, 35.52731371789855075, -10.49813415416005213 ) ) ;
#15914 = CARTESIAN_POINT ( 'NONE',  ( -2.311890736173176641, 88.32268628210144357, -12.53471296425194836 ) ) ;
#15915 = CARTESIAN_POINT ( 'NONE',  ( 16.56230152254411081, -6.928203230275506996, -8.774999998770997678 ) ) ;
#15916 = EDGE_CURVE ( 'NONE', #29947, #14550, #71, .T. ) ;
#15917 = CARTESIAN_POINT ( 'NONE',  ( 27.00000000000000355, 196.1750000000000114, -3.306546357697854128E-15 ) ) ;
#15918 = CARTESIAN_POINT ( 'NONE',  ( 27.78090950529641745, 5.407089921784856479, 163.3246141667165716 ) ) ;
#15919 = CARTESIAN_POINT ( 'NONE',  ( 10.31873187879410558, 3.604726614523240613, -4.734374999385511984 ) ) ;
#15920 = SURFACE_STYLE_USAGE ( .BOTH. , #18585 ) ;
#15921 = CARTESIAN_POINT ( 'NONE',  ( 15.00000000000034461, -3.464101615137956003, -3.956249998770951404 ) ) ;
#15922 = LINE ( 'NONE', #33903, #7871 ) ;
#15923 = CARTESIAN_POINT ( 'NONE',  ( 5.529263428287477744, 89.47268628210143504, -7.954856959092191815 ) ) ;
#15924 = DIRECTION ( 'NONE',  ( -0.000000000000000000, -1.000000000000000000, -0.000000000000000000 ) ) ;
#15925 = CARTESIAN_POINT ( 'NONE',  ( -7.228626920339069173, 140.0726862821014720, 10.49813415415989581 ) ) ;
#15926 = CARTESIAN_POINT ( 'NONE',  ( 19.56230152254412502, 5.196152422706637353, -4.650000000000070521 ) ) ;
#15927 = CARTESIAN_POINT ( 'NONE',  ( 18.12178482187500350, 249.4843750006145342, 4.985214923628407568 ) ) ;
#15928 = ORIENTED_EDGE ( 'NONE', *, *, #30706, .F. ) ;
#15929 = CARTESIAN_POINT ( 'NONE',  ( 24.71349244175073778, 3.604726614523236616, 164.0823405568851570 ) ) ;
#15930 = CARTESIAN_POINT ( 'NONE',  ( 18.12178482187499640, 4.985214923628404904, -2.015624999385456917 ) ) ;
#15931 = EDGE_CURVE ( 'NONE', #27686, #20044, #12929, .T. ) ;
#15932 = CARTESIAN_POINT ( 'NONE',  ( 27.24356964375000700, 196.8968750006144717, 15.72908226750537075 ) ) ;
#15933 = CARTESIAN_POINT ( 'NONE',  ( 25.47825260081467036, 3.464101615137757051, 170.0289409263170626 ) ) ;
#15934 = LINE ( 'NONE', #10233, #36805 ) ;
#15935 = CARTESIAN_POINT ( 'NONE',  ( 26.75643035624999655, 243.3718750006145228, -3.323476615752271712 ) ) ;
#15936 = VECTOR ( 'NONE', #36942, 1000.000000000000000 ) ;
#15937 = CARTESIAN_POINT ( 'NONE',  ( 16.56230152254411436, 7.209453229046475009, -1.153124999385528371 ) ) ;
#15938 = CARTESIAN_POINT ( 'NONE',  ( 8.710071997420211432, 10.51481371789855679, -3.796722387233181895 ) ) ;
#15939 = CARTESIAN_POINT ( 'NONE',  ( 27.24356964374999279, 197.4218750006145342, -15.72908226750539207 ) ) ;
#15941 = EDGE_LOOP ( 'NONE', ( #13295, #30197, #11348, #9359 ) ) ;
#15940 = ORIENTED_EDGE ( 'NONE', *, *, #25175, .F. ) ;
#15942 = CARTESIAN_POINT ( 'NONE',  ( 15.24356964374999990, 247.4968750006145228, 0.000000000000000000 ) ) ;
#15943 = CARTESIAN_POINT ( 'NONE',  ( -2.311890736173447980, 32.07731371789855501, 12.53471296425189330 ) ) ;
#15944 = CARTESIAN_POINT ( 'NONE',  ( 23.87821517812500005, -4.985214923628404016, -3.590624999385477523 ) ) ;
#15945 = CARTESIAN_POINT ( 'NONE',  ( 6.092822981423662299, 123.2148137178985792, 14.25334919248795096 ) ) ;
#15946 = CARTESIAN_POINT ( 'NONE',  ( 18.00000000000000000, 5.196152422706630247, -9.018749998770946519 ) ) ;
#15947 = ORIENTED_EDGE ( 'NONE', *, *, #10404, .T. ) ;
#15948 = CARTESIAN_POINT ( 'NONE',  ( 22.80587116629411426, 7.646167579472024665E-16, -6.271874999385529392 ) ) ;
#15949 = MECHANICAL_DESIGN_GEOMETRIC_PRESENTATION_REPRESENTATION (  '', ( #11092 ), #31695 ) ;
#15950 = VERTEX_POINT ( 'NONE', #25067 ) ;
#15951 = CARTESIAN_POINT ( 'NONE',  ( -27.24356964374999635, 197.1406250006145058, 15.72908226750539384 ) ) ;
#15952 = CARTESIAN_POINT ( 'NONE',  ( -10.69584247140444866, 140.6476862821014890, 6.932735513423972762 ) ) ;
#15953 = CARTESIAN_POINT ( 'NONE',  ( 27.59297993499679791, -5.407089921784865361, 161.1765693489562352 ) ) ;
#15954 = CARTESIAN_POINT ( 'NONE',  ( -60.88169563604516554, 210.1155267958018271, 8.500000000000003553 ) ) ;
#15955 = CARTESIAN_POINT ( 'NONE',  ( 23.87821517812500005, 247.1968750006145115, 4.985214923628404016 ) ) ;
#15956 = CARTESIAN_POINT ( 'NONE',  ( -47.00000000000000711, 244.5000000000000000, -0.4999999999999978351 ) ) ;
#15957 = CARTESIAN_POINT ( 'NONE',  ( -47.81919563604517265, 214.5000000000000284, -0.1155267958017627827 ) ) ;
#15958 = CARTESIAN_POINT ( 'NONE',  ( 20.99999999999997868, 246.0625000000000284, 5.999999999999999112 ) ) ;
#15959 = CARTESIAN_POINT ( 'NONE',  ( 10.31873187879410558, 3.604726614523240613, -10.13437499938549280 ) ) ;
#15960 = ORIENTED_EDGE ( 'NONE', *, *, #22903, .T. ) ;
#15961 = AXIS2_PLACEMENT_3D ( 'NONE', #13125, #24679, #13492 ) ;
#15962 = DIRECTION ( 'NONE',  ( 0.9961946980917462113, 0.000000000000000000, -0.08715574274765118534 ) ) ;
#15963 = CARTESIAN_POINT ( 'NONE',  ( 15.50000000000000533, 127.7101862821014606, 0.1745138560725827404 ) ) ;
#15964 = CARTESIAN_POINT ( 'NONE',  ( -49.21205436395490551, 216.1378603801730094, 6.307003348497944195 ) ) ;
#15965 = CARTESIAN_POINT ( 'NONE',  ( -6.594114490232312775, 115.0601862821014691, -6.840914352312096547 ) ) ;
#15966 = ADVANCED_FACE ( 'NONE', ( #19032 ), #2506, .F. ) ;
#15967 = CARTESIAN_POINT ( 'NONE',  ( 13.49999999999999645, 199.4000000000000341, -23.38268590217984766 ) ) ;
#15968 = CARTESIAN_POINT ( 'NONE',  ( 11.61527771782819940, 16.73518628210143788, -4.622313124798573369 ) ) ;
#15969 = CARTESIAN_POINT ( 'NONE',  ( 22.56230152254412147, 7.347880794884125653E-16, -8.325000000000027711 ) ) ;
#15970 = ORIENTED_EDGE ( 'NONE', *, *, #6796, .F. ) ;
#15971 = CARTESIAN_POINT ( 'NONE',  ( 16.56230152254411436, -6.928203230275514990, -7.987500000000027356 ) ) ;
#15972 = CARTESIAN_POINT ( 'NONE',  ( -3.796722387233375073, 84.58518628210146062, 8.710071997420127943 ) ) ;
#15973 =( GEOMETRIC_REPRESENTATION_CONTEXT ( 3 ) GLOBAL_UNCERTAINTY_ASSIGNED_CONTEXT ( ( #21478 ) ) GLOBAL_UNIT_ASSIGNED_CONTEXT ( ( #33793, #13145, #22054 ) ) REPRESENTATION_CONTEXT ( 'NONE', 'WORKASPACE' ) );
#15974 = FACE_OUTER_BOUND ( 'NONE', #30433, .T. ) ;
#15975 = CARTESIAN_POINT ( 'NONE',  ( 3.796722387233182339, 132.4148137178985678, 8.710071997420207879 ) ) ;
#15976 = EDGE_CURVE ( 'NONE', #32727, #35189, #4232, .T. ) ;
#15977 = CARTESIAN_POINT ( 'NONE',  ( 27.24356964375000700, 199.0906250006145228, 15.72908226750537075 ) ) ;
#15978 = CARTESIAN_POINT ( 'NONE',  ( 19.39230484541326049, 244.9575961894323086, -5.999999999999997335 ) ) ;
#15979 = CARTESIAN_POINT ( 'NONE',  ( 5.778771075727756162E-15, 197.2718750006145569, 31.45816453501075927 ) ) ;
#15980 = CARTESIAN_POINT ( 'NONE',  ( 21.00000000000000355, 0.000000000000000000, 50.00000000000001421 ) ) ;
#15981 = VECTOR ( 'NONE', #28535, 1000.000000000000000 ) ;
#15982 = ADVANCED_FACE ( 'NONE', ( #32667, #18280 ), #29824, .T. ) ;
#15983 = CARTESIAN_POINT ( 'NONE',  ( 26.99999999999999645, 242.1625000000000227, -3.464101615137755275 ) ) ;
#15984 = CARTESIAN_POINT ( 'NONE',  ( -0.1745138560723084320, 73.18981371789854506, -9.500000000000005329 ) ) ;
#15985 = EDGE_LOOP ( 'NONE', ( #28319, #7402, #28925, #7046 ) ) ;
#15986 = CARTESIAN_POINT ( 'NONE',  ( 24.00000000000000000, 243.4562500012290513, 5.196152422706629359 ) ) ;
#15987 = CARTESIAN_POINT ( 'NONE',  ( -8.715434833792127023, 88.13981371789856212, 8.962234695871568846 ) ) ;
#15988 = CARTESIAN_POINT ( 'NONE',  ( 22.80587116629412847, -3.604726614523238837, -4.059374999385534366 ) ) ;
#15989 = CARTESIAN_POINT ( 'NONE',  ( -11.68933346642354998, 143.0000000000000000, 7.290916064140882114 ) ) ;
#15990 = CARTESIAN_POINT ( 'NONE',  ( 21.00000000000000000, -6.646953231504538984, -4.640624999385471128 ) ) ;
#15991 = CARTESIAN_POINT ( 'NONE',  ( 12.46528703574811558, 47.60231371789855359, -2.660918448318005503 ) ) ;
#15992 = VERTEX_POINT ( 'NONE', #18664 ) ;
#15993 = B_SPLINE_CURVE_WITH_KNOTS ( 'NONE', 1,
 ( #33481, #14138 ),
 .UNSPECIFIED., .F., .F.,
 ( 2, 2 ),
 ( 0.000000000000000000, 1.000000000000000000 ),
 .UNSPECIFIED. ) ;
#15994 = CARTESIAN_POINT ( 'NONE',  ( 20.99999999999999645, 6.646953231504538984, -6.553124999385445903 ) ) ;
#15995 = CARTESIAN_POINT ( 'NONE',  ( 26.75643035624999655, 244.6093750006145342, -3.323476615752271712 ) ) ;
#15996 = CARTESIAN_POINT ( 'NONE',  ( 11.61527771782819940, 25.93518628210143717, -4.622313124798573369 ) ) ;
#15997 = CARTESIAN_POINT ( 'NONE',  ( -37.72544563604516554, 214.8429017333602360, 4.673758765035156415 ) ) ;
#15998 = CARTESIAN_POINT ( 'NONE',  ( -60.88169563604516554, 210.1155267958017703, 6.500000000000000888 ) ) ;
#15999 = PRODUCT_DEFINITION_FORMATION_WITH_SPECIFIED_SOURCE ( 'ANY', '', #3198, .NOT_KNOWN. ) ;
#16000 = CARTESIAN_POINT ( 'NONE',  ( 10.56230152254410726, 0.000000000000000000, -8.100000000000024514 ) ) ;
#16001 = CARTESIAN_POINT ( 'NONE',  ( -10.69584247140429412, 62.55231371789856354, -6.932735513424201024 ) ) ;
#16002 = CARTESIAN_POINT ( 'NONE',  ( -43.67038769728823411, 208.6787018382581778, 4.469044688360752637 ) ) ;
#16003 = VECTOR ( 'NONE', #1625, 1000.000000000000000 ) ;
#16004 = CARTESIAN_POINT ( 'NONE',  ( -59.89955436395490551, 214.8429017333601792, -4.673758765035196383 ) ) ;
#16005 = CARTESIAN_POINT ( 'NONE',  ( 26.99999999999999645, 195.8750000012290400, -15.58845726811990495 ) ) ;
#16006 = DIRECTION ( 'NONE',  ( -0.000000000000000000, -1.000000000000000000, -0.000000000000000000 ) ) ;
#16007 = CARTESIAN_POINT ( 'NONE',  ( 0.1745138560722461762, 40.98981371789854933, 15.50000000000000533 ) ) ;
#16008 = CARTESIAN_POINT ( 'NONE',  ( -45.44419563604516554, 201.5000000000000000, 0.1155267958018195706 ) ) ;
#16009 = CARTESIAN_POINT ( 'NONE',  ( 26.97716818855048260, 0.000000000000000000, 49.47706554351410801 ) ) ;
#16010 = CARTESIAN_POINT ( 'NONE',  ( -0.1745138560725500443, 74.81018628210145494, 12.50000000000000355 ) ) ;
#16011 = CARTESIAN_POINT ( 'NONE',  ( -5.770363421893818234, 32.83518628210143930, -14.38691631536207005 ) ) ;
#16012 = LINE ( 'NONE', #12975, #5949 ) ;
#16013 = CARTESIAN_POINT ( 'NONE',  ( -28.78598427599741072, 202.8118011321232643, -3.549815969672131200 ) ) ;
#16014 = ORIENTED_EDGE ( 'NONE', *, *, #36792, .F. ) ;
#16015 = CARTESIAN_POINT ( 'NONE',  ( 14.25334919248782661, 27.08518628210144996, 6.092822981423971385 ) ) ;
#16016 = CARTESIAN_POINT ( 'NONE',  ( -27.24356964375000345, 196.6531250006145513, 0.000000000000000000 ) ) ;
#16017 = DIRECTION ( 'NONE',  ( 0.000000000000000000, 1.000000000000000000, -2.168404344971006896E-16 ) ) ;
#16018 = LINE ( 'NONE', #22446, #17174 ) ;
#16019 = CARTESIAN_POINT ( 'NONE',  ( -37.13913769728823411, 206.8500491399821044, -5.686928522499717253 ) ) ;
#16020 = CARTESIAN_POINT ( 'NONE',  ( 16.56230152254411436, 6.928203230275506996, -7.649999998770994125 ) ) ;
#16021 = CARTESIAN_POINT ( 'NONE',  ( -44.35000000000001563, 244.5000000000000000, 5.000000000000000000 ) ) ;
#16022 = CARTESIAN_POINT ( 'NONE',  ( 9.534712964251900402, 130.9773137178985394, 1.715153634034445540 ) ) ;
#16023 = CARTESIAN_POINT ( 'NONE',  ( 23.87821517812500005, 245.0593750006145228, 4.985214923628404016 ) ) ;
#16024 = VERTEX_POINT ( 'NONE', #16000 ) ;
#16025 = FACE_OUTER_BOUND ( 'NONE', #32112, .T. ) ;
#16026 = FACE_OUTER_BOUND ( 'NONE', #22641, .T. ) ;
#16027 = CARTESIAN_POINT ( 'NONE',  ( 12.46528703574811558, 139.6023137178985678, -2.660918448318005947 ) ) ;
#16028 = CARTESIAN_POINT ( 'NONE',  ( 16.56230152254411081, -7.209453229046475009, -5.878124999385531346 ) ) ;
#16029 = CARTESIAN_POINT ( 'NONE',  ( 27.99008328789078703, -5.407089921784859143, 165.7154814421367348 ) ) ;
#16030 = CARTESIAN_POINT ( 'NONE',  ( 23.99999999999999645, 5.196152422706631135, -1.950000000000007283 ) ) ;
#16031 = CARTESIAN_POINT ( 'NONE',  ( -13.50000000000000533, 198.5749999999999886, -23.38268590217984411 ) ) ;
#16032 = ORIENTED_EDGE ( 'NONE', *, *, #20856, .F. ) ;
#16033 = CARTESIAN_POINT ( 'NONE',  ( -2.660918448318275509, 29.09768628210144925, 12.46528703574805874 ) ) ;
#16034 = EDGE_LOOP ( 'NONE', ( #32366, #6168, #6261, #10472 ) ) ;
#16035 = VERTEX_POINT ( 'NONE', #26794 ) ;
#16036 = CARTESIAN_POINT ( 'NONE',  ( -1.045839947578415010E-13, 196.0625000000000284, 27.00000000000000355 ) ) ;
#16037 = CARTESIAN_POINT ( 'NONE',  ( 26.75643035624999655, -3.323476615752267271, -0.8531249993854884694 ) ) ;
#16038 = CARTESIAN_POINT ( 'NONE',  ( 22.56230152254602928, -3.464101615136651713, -9.262499999999995737 ) ) ;
#16039 = CARTESIAN_POINT ( 'NONE',  ( -1.045839947578415010E-13, 196.5125000000000455, 27.00000000000000355 ) ) ;
#16040 = CARTESIAN_POINT ( 'NONE',  ( 18.12178482187500350, -4.985214923628407568, -8.615624999385479654 ) ) ;
#16041 = CARTESIAN_POINT ( 'NONE',  ( 12.46528703574805874, 81.99768628210146915, 2.660918448318279950 ) ) ;
#16042 = CARTESIAN_POINT ( 'NONE',  ( -11.08355503943118592, 7.639813717898540801, -10.83675517735179383 ) ) ;
#16043 =( BOUNDED_CURVE ( )  B_SPLINE_CURVE ( 2, ( #23811, #14394, #25951, #15470, #14212, #27024, #2823 ),
 .UNSPECIFIED., .F., .F. ) 
 B_SPLINE_CURVE_WITH_KNOTS ( ( 3, 2, 2, 3 ),
 ( 0.2391304347826092025, 0.2463768115942035208, 0.2536231884057978392, 0.2608695652173921298 ),
 .UNSPECIFIED. ) 
 CURVE ( )  GEOMETRIC_REPRESENTATION_ITEM ( )  RATIONAL_B_SPLINE_CURVE ( ( 0.9999999999999907851, 0.8660254037844479225, 1.000000000000000000, 0.8660254037844387076, 1.000000000000000000, 0.8660254037844232755, 1.000000000000015321 ) ) 
 REPRESENTATION_ITEM ( '' )  );
#16044 = CARTESIAN_POINT ( 'NONE',  ( 22.56230152254411792, 7.347880794884125653E-16, -5.625000000000018652 ) ) ;
#16045 = CARTESIAN_POINT ( 'NONE',  ( 8.945811011644241972, 214.5203208706332418, 3.964960503605297948 ) ) ;
#16046 = CARTESIAN_POINT ( 'NONE',  ( -54.94419563604517265, 205.4999999999999716, 0.1155267958017633378 ) ) ;
#16047 = CARTESIAN_POINT ( 'NONE',  ( 0.000000000000000000, 0.000000000000000000, 0.000000000000000000 ) ) ;
#16048 = CARTESIAN_POINT ( 'NONE',  ( 37.15151170766156952, 7.347880794884117764E-16, 165.7703441132237003 ) ) ;
#16049 = CARTESIAN_POINT ( 'NONE',  ( -2.660918448318004614, 128.1023137178985678, -12.46528703574811558 ) ) ;
#16050 = CARTESIAN_POINT ( 'NONE',  ( -46.83705436395489841, 205.3262412349647263, -4.842901733360204020 ) ) ;
#16051 = CARTESIAN_POINT ( 'NONE',  ( -51.98288769728823411, 201.5309553116392181, -2.393094931466246855 ) ) ;
#16052 = SHAPE_DEFINITION_REPRESENTATION ( #22565, #35512 ) ;
#16053 = CARTESIAN_POINT ( 'NONE',  ( 20.99999999999999645, 6.646953231504538984, -1.265624999385487115 ) ) ;
#16054 = CARTESIAN_POINT ( 'NONE',  ( 27.24356964374999635, 196.9156250006145399, -15.72908226750539029 ) ) ;
#16055 = CARTESIAN_POINT ( 'NONE',  ( -14.38691631536193860, 108.2648137178985621, -5.770363421894132649 ) ) ;
#16056 = CARTESIAN_POINT ( 'NONE',  ( -51.18377896937847993, 208.3738570449995109, 6.530955311639247363 ) ) ;
#16057 = ORIENTED_EDGE ( 'NONE', *, *, #7625, .T. ) ;
#16058 = VECTOR ( 'NONE', #10423, 1000.000000000000000 ) ;
#16059 = CARTESIAN_POINT ( 'NONE',  ( 8.715434833791931624, 128.8601862821014663, 8.962234695871760692 ) ) ;
#16060 = CARTESIAN_POINT ( 'NONE',  ( 3.257655550457285720, 79.69768628210141515, -15.46528703574804986 ) ) ;
#16061 = CARTESIAN_POINT ( 'NONE',  ( -77.00000000000002842, 210.0000000000000000, 0.000000000000000000 ) ) ;
#16062 =( BOUNDED_CURVE ( )  B_SPLINE_CURVE ( 2, ( #1252, #26657, #24202, #24389, #3723, #21558, #33103, #32347, #15296, #687, #23828, #26849, #12258, #7147, #30262, #16611, #36863, #24754, #13765, #1816, #36304, #13574, #25311, #7889, #4474, #19282, #36683, #16053, #5031, #2374, #21741, #10908, #13949, #22485, #36124, #13385, #21925, #30822, #24937, #1632, #10165, #36492, #33472, #34031, #27601, #8075, #30457, #10535, #19650, #10721, #22295, #33290, #33848, #7516, #19088, #31192, #22112, #33660, #18904, #7700, #19463, #7331, #2184, #4845, #16424, #30640, #31010, #13204, #27970, #2001, #10352, #25127, #4656, #16239, #27789, #5217, #28153, #16793, #28338, #17536, #31925, #19834, #25686, #6142, #34769, #23402, #3300, #34951, #22853, #2560, #23220, #29070, #2742, #14495, #8811, #31555, #25497, #11644, #14130, #34403, #34216, #11285, #31374, #37235, #8441, #17719, #23036, #11466, #5957, #26230, #20009, #3114, #28706, #5579, #29260, #20384, #17165, #5395, #8261, #14315, #25868, #37050, #20566, #31742, #17350, #14681, #268, #37416, #11098, #34582, #8624, #20192, #5770, #28892, #2927, #26052, #80, #11831, #8996, #32109, #22671, #16975, #28517, #35132, #18669, #26609, #3488, #14871, #24343, #4050, #35884, #18480, #1200, #18101, #7100, #30020, #30211, #12397, #26418, #33053, #26798, #830, #9558, #29642, #21134, #3865, #32671, #18286, #638, #29828, #3679, #12207, #452, #15623, #24153, #20752, #35513, #15438, #32298, #21321, #12021, #9928, #9748, #12773, #17909, #6714, #6527, #26987, #23970, #1014, #9184, #35696, #23590, #21509, #12587, #15059, #6338, #32861, #35318, #23780, #6908, #27176, #29453, #9373, #20947, #32480, #15247, #30593, #19042 ),
 .UNSPECIFIED., .F., .F. ) 
 B_SPLINE_CURVE_WITH_KNOTS ( ( 3, 2, 2, 2, 2, 2, 2, 2, 2, 2, 2, 2, 2, 2, 2, 2, 2, 2, 2, 2, 2, 2, 2, 2, 2, 2, 2, 2, 2, 2, 2, 2, 2, 2, 2, 2, 2, 2, 2, 2, 2, 2, 2, 2, 2, 2, 2, 2, 2, 2, 2, 2, 2, 2, 2, 2, 2, 2, 2, 2, 2, 2, 2, 2, 2, 2, 2, 2, 2, 2, 2, 2, 2, 2, 2, 2, 2, 2, 2, 2, 2, 2, 2, 2, 2, 2, 2, 2, 2, 2, 2, 2, 2, 2, 2, 2, 2, 2, 2, 2, 2, 2, 2, 2, 3 ),
 ( 0.000000000000000000, 0.007246376811594203854, 0.01449275362318840771, 0.02173913043478261156, 0.02898550724637681542, 0.03623188405797101580, 0.04347826086956522312, 0.05072463768115942351, 0.05797101449275363083, 0.06521739130434782428, 0.07246376811594203160, 0.07971014492753622505, 0.08695652173913044625, 0.09420289855072463969, 0.1014492753623188470, 0.1086956521739130266, 0.1159420289855072617, 0.1231884057971014551, 0.1304347826086956486, 0.1376811594202898559, 0.1449275362318840632, 0.1521739130434782705, 0.1594202898550724501, 0.1666666666666666574, 0.1739130434782608925, 0.1811594202898550721, 0.1884057971014492794, 0.1956521739130434867, 0.2028985507246376940, 0.2101449275362318736, 0.2173913043478260532, 0.2246376811594203160, 0.2318840579710145233, 0.2391304347826087029, 0.2463768115942029102, 0.2536231884057971175, 0.2608695652173912971, 0.2681159420289855322, 0.2753623188405797118, 0.2826086956521738913, 0.2898550724637681264, 0.2971014492753623060, 0.3043478260869565410, 0.3115942028985507206, 0.3188405797101449002, 0.3260869565217391353, 0.3333333333333333148, 0.3405797101449275499, 0.3478260869565217850, 0.3550724637681159090, 0.3623188405797101441, 0.3695652173913043237, 0.3768115942028985588, 0.3840579710144927383, 0.3913043478260869734, 0.3985507246376811530, 0.4057971014492753881, 0.4130434782608695676, 0.4202898550724637472, 0.4275362318840579823, 0.4347826086956521063, 0.4420289855072463969, 0.4492753623188406320, 0.4565217391304347561, 0.4637681159420290466, 0.4710144927536231707, 0.4782608695652174058, 0.4855072463768115854, 0.4927536231884058204, 0.5000000000000000000, 0.5072463768115942351, 0.5144927536231883591, 0.5217391304347825942, 0.5289855072463768293, 0.5362318840579710644, 0.5434782608695651884, 0.5507246376811594235, 0.5579710144927536586, 0.5652173913043477826, 0.5724637681159420177, 0.5797101449275362528, 0.5869565217391304879, 0.5942028985507246119, 0.6014492753623188470, 0.6086956521739130821, 0.6159420289855072062, 0.6231884057971014412, 0.6304347826086956763, 0.6376811594202898004, 0.6449275362318840354, 0.6521739130434782705, 0.6594202898550725056, 0.6666666666666666297, 0.6739130434782608647, 0.6811594202898550998, 0.6884057971014492239, 0.6956521739130435700, 0.7028985507246376940, 0.7101449275362318181, 0.7173913043478260532, 0.7246376811594202882, 0.7318840579710145233, 0.7391304347826086474, 0.7463768115942028825, 0.7485758418660213298 ),
 .UNSPECIFIED. ) 
 CURVE ( )  GEOMETRIC_REPRESENTATION_ITEM ( )  RATIONAL_B_SPLINE_CURVE ( ( 1.000000000000000000, 0.8660254037844387076, 1.000000000000000000, 0.8660254037844387076, 1.000000000000000000, 0.8660254037844387076, 1.000000000000000000, 0.8660254037844387076, 1.000000000000000000, 0.8660254037844387076, 1.000000000000000000, 0.8660254037844387076, 1.000000000000000000, 0.8660254037844387076, 1.000000000000000000, 0.8660254037844387076, 1.000000000000000000, 0.8660254037844387076, 1.000000000000000000, 0.8660254037844387076, 1.000000000000000000, 0.8660254037844387076, 1.000000000000000000, 0.8660254037844387076, 1.000000000000000000, 0.8660254037844387076, 1.000000000000000000, 0.8660254037844387076, 1.000000000000000000, 0.8660254037844387076, 1.000000000000000000, 0.8660254037844387076, 1.000000000000000000, 0.8660254037844387076, 1.000000000000000000, 0.8660254037844387076, 1.000000000000000000, 0.8660254037844387076, 1.000000000000000000, 0.8660254037844387076, 1.000000000000000000, 0.8660254037844387076, 1.000000000000000000, 0.8660254037844387076, 1.000000000000000000, 0.8660254037844387076, 1.000000000000000000, 0.8660254037844387076, 1.000000000000000000, 0.8660254037844387076, 1.000000000000000000, 0.8660254037844387076, 1.000000000000000000, 0.8660254037844387076, 1.000000000000000000, 0.8660254037844387076, 1.000000000000000000, 0.8660254037844387076, 1.000000000000000000, 0.8660254037844387076, 1.000000000000000000, 0.8660254037844387076, 1.000000000000000000, 0.8660254037844387076, 1.000000000000000000, 0.8660254037844387076, 1.000000000000000000, 0.8660254037844387076, 1.000000000000000000, 0.8660254037844387076, 1.000000000000000000, 0.8660254037844387076, 1.000000000000000000, 0.8660254037844387076, 1.000000000000000000, 0.8660254037844387076, 1.000000000000000000, 0.8660254037844387076, 1.000000000000000000, 0.8660254037844387076, 1.000000000000000000, 0.8660254037844387076, 1.000000000000000000, 0.8660254037844387076, 1.000000000000000000, 0.8660254037844387076, 1.000000000000000000, 0.8660254037844387076, 1.000000000000000000, 0.8660254037844387076, 1.000000000000000000, 0.8660254037844387076, 1.000000000000000000, 0.8660254037844387076, 1.000000000000000000, 0.8660254037844387076, 1.000000000000000000, 0.8660254037844387076, 1.000000000000000000, 0.8660254037844387076, 1.000000000000000000, 0.8660254037844387076, 1.000000000000000000, 0.8660254037844387076, 1.000000000000000000, 0.8660254037844387076, 1.000000000000000000, 0.8660254037844387076, 1.000000000000000000, 0.8660254037844387076, 1.000000000000000000, 0.8660254037844387076, 1.000000000000000000, 0.8660254037844387076, 1.000000000000000000, 0.8660254037844387076, 1.000000000000000000, 0.8660254037844387076, 1.000000000000000000, 0.8660254037844387076, 1.000000000000000000, 0.8660254037844387076, 1.000000000000000000, 0.8660254037844387076, 1.000000000000000000, 0.8660254037844387076, 1.000000000000000000, 0.8660254037844387076, 1.000000000000000000, 0.8660254037844387076, 1.000000000000000000, 0.8660254037844387076, 1.000000000000000000, 0.8660254037844387076, 1.000000000000000000, 0.8660254037844387076, 1.000000000000000000, 0.8660254037844387076, 1.000000000000000000, 0.8660254037844387076, 1.000000000000000000, 0.8660254037844387076, 1.000000000000000000, 0.8660254037844387076, 1.000000000000000000, 0.8660254037844387076, 1.000000000000000000, 0.8660254037844387076, 1.000000000000000000, 0.8660254037844387076, 1.000000000000000000, 0.8660254037844387076, 1.000000000000000000, 0.8660254037844387076, 1.000000000000000000, 0.8660254037844387076, 1.000000000000000000, 0.8660254037844387076, 1.000000000000000000, 0.8660254037844387076, 1.000000000000000000, 0.8660254037844387076, 1.000000000000000000, 0.8660254037844387076, 1.000000000000000000, 0.8660254037844387076, 1.000000000000000000, 0.8660254037844387076, 1.000000000000000000, 0.8660254037844387076, 1.000000000000000000, 0.8660254037844387076, 1.000000000000000000, 0.8660254037844387076, 1.000000000000000000, 0.8660254037844387076, 1.000000000000000000, 0.8660254037844387076, 1.000000000000000000, 0.8660254037844387076, 1.000000000000000000, 0.8660254037844387076, 1.000000000000000000, 0.8660254037844387076, 1.000000000000000000, 0.8660254037844387076, 1.000000000000000000, 0.8660254037844387076, 1.000000000000000000, 0.8660254037844387076, 1.000000000000000000, 0.8660254037844387076, 1.000000000000000000, 0.8660254037844387076, 1.000000000000000000, 0.8660254037844387076, 1.000000000000000000, 0.8660254037844387076, 1.000000000000000000, 0.8660254037844387076, 1.000000000000000000, 0.8660254037844387076, 1.000000000000000000, 0.8660254037844387076, 1.000000000000000000, 0.8660254037844387076, 1.000000000000000000, 0.9593432414028914001, 0.9433623850486823059 ) ) 
 REPRESENTATION_ITEM ( '' )  );
#16063 = CARTESIAN_POINT ( 'NONE',  ( 31.03952447949476223, 7.209453229046482114, 164.7522898954867401 ) ) ;
#16064 = CARTESIAN_POINT ( 'NONE',  ( -14.38691631536207183, 85.73518628210145209, 5.770363421893814682 ) ) ;
#16065 = CARTESIAN_POINT ( 'NONE',  ( -53.56622103062156981, 211.6261429550005744, 6.530955311639228711 ) ) ;
#16066 = CARTESIAN_POINT ( 'NONE',  ( 10.31873187879411091, 0.000000000000000000, -4.640624999385528859 ) ) ;
#16067 = CARTESIAN_POINT ( 'NONE',  ( -2.064181346179269738, 47.49768628210145494, 9.465287035748067623 ) ) ;
#16068 = DIRECTION ( 'NONE',  ( 0.000000000000000000, 0.000000000000000000, -1.000000000000000000 ) ) ;
#16069 = CARTESIAN_POINT ( 'NONE',  ( -38.12872103062156270, 201.4690446883607819, 2.162041339862843525 ) ) ;
#16070 = CARTESIAN_POINT ( 'NONE',  ( 10.31873187879410381, 0.000000000000000000, -9.646874999385518734 ) ) ;
#16071 = CARTESIAN_POINT ( 'NONE',  ( -12.50000000000000355, 67.91018628210144925, -0.1745138560725492671 ) ) ;
#16072 = CARTESIAN_POINT ( 'NONE',  ( 26.99999999999999645, 199.8125000000000000, -15.58845726811990495 ) ) ;
#16073 = CARTESIAN_POINT ( 'NONE',  ( -27.24356964375000345, 199.8312500006145171, 0.000000000000000000 ) ) ;
#16075 = CARTESIAN_POINT ( 'NONE',  ( 22.80587116629411781, -3.604726614523238837, -0.9093749993854999270 ) ) ;
#16074 = CARTESIAN_POINT ( 'NONE',  ( 5.233372021372432847, 37.14768628210143220, 8.152565276336710909 ) ) ;
#16076 = CARTESIAN_POINT ( 'NONE',  ( 2.999999999999997335, 244.5000000000000000, 5.000000000000000000 ) ) ;
#16077 = ORIENTED_EDGE ( 'NONE', *, *, #4990, .T. ) ;
#16078 = CARTESIAN_POINT ( 'NONE',  ( 15.00000000000000178, -3.464101615137757051, -3.112500000000005596 ) ) ;
#16079 = CARTESIAN_POINT ( 'NONE',  ( 37.09591843811324452, 3.604726614523243278, 162.3402618868670118 ) ) ;
#16080 = CARTESIAN_POINT ( 'NONE',  ( 33.67594490067671842, -5.196152422706635576, 160.4655734646546534 ) ) ;
#16081 = CARTESIAN_POINT ( 'NONE',  ( 26.99999999999999645, 244.7874999999999943, 3.464101615137751278 ) ) ;
#16082 = DIRECTION ( 'NONE',  ( 0.000000000000000000, 0.000000000000000000, -1.000000000000000000 ) ) ;
#16083 = CARTESIAN_POINT ( 'NONE',  ( 6.932735513424201024, 92.45231371789856212, -10.69584247140429412 ) ) ;
#16084 = CARTESIAN_POINT ( 'NONE',  ( -8.715434833791929847, 78.26018628210144357, -8.962234695871762469 ) ) ;
#16085 = ORIENTED_EDGE ( 'NONE', *, *, #23832, .T. ) ;
#16086 = ORIENTED_EDGE ( 'NONE', *, *, #29560, .F. ) ;
#16087 = CARTESIAN_POINT ( 'NONE',  ( 26.99999999999999645, 199.4750000012290343, -15.58845726811990495 ) ) ;
#16088 = CARTESIAN_POINT ( 'NONE',  ( 13.04141134922778988, 56.22731371789854649, -8.927990412390371944 ) ) ;
#16089 = CARTESIAN_POINT ( 'NONE',  ( 18.12178482187499640, 4.985214923628404904, -7.528124999385488181 ) ) ;
#16090 = VECTOR ( 'NONE', #32509, 1000.000000000000000 ) ;
#16091 = CARTESIAN_POINT ( 'NONE',  ( 15.24356964375000167, 246.2968750006145626, 3.323476615752272600 ) ) ;
#16092 = CARTESIAN_POINT ( 'NONE',  ( -50.79538769728824121, 211.3212981617418222, -4.469044688360751749 ) ) ;
#16093 = CARTESIAN_POINT ( 'NONE',  ( -27.00000000000000355, 199.5124999999999886, -15.58845726811989429 ) ) ;
#16094 = CARTESIAN_POINT ( 'NONE',  ( 9.534712964251900402, 66.57731371789853370, 1.715153634034445540 ) ) ;
#16095 = CARTESIAN_POINT ( 'NONE',  ( 22.80587116629411071, 7.646167579472015790E-16, -8.915624999385585170 ) ) ;
#16096 = ADVANCED_FACE ( 'NONE', ( #15243 ), #30205, .F. ) ;
#16097 = CARTESIAN_POINT ( 'NONE',  ( -6.594114490232462877, 97.33981371789856496, 6.840914352311949109 ) ) ;
#16098 = CARTESIAN_POINT ( 'NONE',  ( 13.50000000000001421, 197.9000000000000341, 23.38268590217984055 ) ) ;
#16099 = CARTESIAN_POINT ( 'NONE',  ( 4.622313124798831829, 27.76481371789854435, -11.61527771782809282 ) ) ;
#16100 =( BOUNDED_CURVE ( )  B_SPLINE_CURVE ( 2, ( #33665, #33478, #18537, #33297, #7706, #7153, #24578 ),
 .UNSPECIFIED., .F., .F. ) 
 B_SPLINE_CURVE_WITH_KNOTS ( ( 3, 2, 2, 3 ),
 ( 0.7608695652173899093, 0.7681159420289840334, 0.7753623188405783795, 0.7826086956521726146 ),
 .UNSPECIFIED. ) 
 CURVE ( )  GEOMETRIC_REPRESENTATION_ITEM ( )  RATIONAL_B_SPLINE_CURVE ( ( 1.000000000000026645, 0.8660254037844120623, 1.000000000000000000, 0.8660254037844387076, 1.000000000000000000, 0.8660254037844633546, 0.9999999999999753530 ) ) 
 REPRESENTATION_ITEM ( '' )  );
#16101 = CARTESIAN_POINT ( 'NONE',  ( -11.61527771782819940, 76.53518628210146346, 4.622313124798574258 ) ) ;
#16102 = CARTESIAN_POINT ( 'NONE',  ( 10.56230152254410903, 3.464101615137752166, -8.924999998771019349 ) ) ;
#16103 = EDGE_CURVE ( 'NONE', #2107, #13050, #10264, .T. ) ;
#16104 = DIRECTION ( 'NONE',  ( 0.000000000000000000, 0.000000000000000000, -1.000000000000000000 ) ) ;
#16105 = CARTESIAN_POINT ( 'NONE',  ( 30.75027635825099281, -7.209453229046475009, 161.4461687411947821 ) ) ;
#16106 = CARTESIAN_POINT ( 'NONE',  ( 16.56230152254411081, 7.209453229046482114, -5.709374999385496530 ) ) ;
#16107 = CARTESIAN_POINT ( 'NONE',  ( 24.89321967762106169, 0.000000000000000000, 163.3419840153761982 ) ) ;
#16108 = LINE ( 'NONE', #27841, #18186 ) ;
#16109 = CARTESIAN_POINT ( 'NONE',  ( 6.594114490232313663, 92.06018628210145494, 6.840914352312096547 ) ) ;
#16110 = DIRECTION ( 'NONE',  ( 0.8083506638593009885, 0.5887012860850800999, 0.000000000000000000 ) ) ;
#16111 = CARTESIAN_POINT ( 'NONE',  ( -10.69584247140444866, 140.6476862821014890, 6.932735513423972762 ) ) ;
#16112 = CARTESIAN_POINT ( 'NONE',  ( 20.99999999999999289, 240.4937500012290457, -5.999999999999997335 ) ) ;
#16113 = CARTESIAN_POINT ( 'NONE',  ( 23.87821517812500005, 249.5593750006145228, 4.985214923628404016 ) ) ;
#16114 = VERTEX_POINT ( 'NONE', #34348 ) ;
#16115 = CARTESIAN_POINT ( 'NONE',  ( 37.13350435217314782, -3.604726614523235284, 162.7698708504190392 ) ) ;
#16116 = CARTESIAN_POINT ( 'NONE',  ( 21.00000000000000000, 6.646953231504538984, -4.753124999385462068 ) ) ;
#16117 = ADVANCED_FACE ( 'NONE', ( #5160 ), #33976, .T. ) ;
#16118 = CARTESIAN_POINT ( 'NONE',  ( -27.24356964374999279, 196.7468750006145513, 15.72908226750539384 ) ) ;
#16119 = CARTESIAN_POINT ( 'NONE',  ( 37.34107544803060108, 3.464101615137759271, 167.9370675803488666 ) ) ;
#16120 = LINE ( 'NONE', #1510, #31968 ) ;
#16121 = CARTESIAN_POINT ( 'NONE',  ( 26.75643035624999655, 242.4343750006145513, -7.049594010296217766E-16 ) ) ;
#16122 = CARTESIAN_POINT ( 'NONE',  ( 25.05990503573306682, 0.000000000000000000, 165.2472063767010013 ) ) ;
#16123 = CARTESIAN_POINT ( 'NONE',  ( 8.962234695871567070, 141.0398137178985678, 8.715434833792127023 ) ) ;
#16124 = CARTESIAN_POINT ( 'NONE',  ( 13.62178482187499640, 195.6593750006145456, -23.59362340125807123 ) ) ;
#16126 = ORIENTED_EDGE ( 'NONE', *, *, #5885, .F. ) ;
#16125 = ORIENTED_EDGE ( 'NONE', *, *, #23212, .T. ) ;
#16127 = CARTESIAN_POINT ( 'NONE',  ( 23.87821517812500005, 245.3968750006145285, 4.985214923628404016 ) ) ;
#16128 = AXIS2_PLACEMENT_3D ( 'NONE', #2101, #19188, #19377 ) ;
#16129 = CARTESIAN_POINT ( 'NONE',  ( 12.50000000000000355, 11.08981371789855075, -0.1745138560722771515 ) ) ;
#16130 = CARTESIAN_POINT ( 'NONE',  ( 21.00000000000000000, 6.646953231504538984, -3.853124999385470595 ) ) ;
#16131 = CARTESIAN_POINT ( 'NONE',  ( -3.257655550456946880, 109.7023137178985479, -15.46528703574811736 ) ) ;
#16132 = CARTESIAN_POINT ( 'NONE',  ( 21.00000000000000000, -6.928203230275506996, -9.281249998770942256 ) ) ;
#16133 = CARTESIAN_POINT ( 'NONE',  ( 22.80587116629411781, 7.646167579472024665E-16, -5.821874999385522997 ) ) ;
#16134 = ORIENTED_EDGE ( 'NONE', *, *, #9448, .T. ) ;
#16135 = CARTESIAN_POINT ( 'NONE',  ( 27.24356964375000700, 195.9406250006145456, 15.72908226750537075 ) ) ;
#16136 = CARTESIAN_POINT ( 'NONE',  ( -2.311890736173176641, 125.1226862821014549, -12.53471296425194836 ) ) ;
#16137 = CARTESIAN_POINT ( 'NONE',  ( 13.44051670066911619, -5.407089921784859143, -0.9656249993855170466 ) ) ;
#16138 = CARTESIAN_POINT ( 'NONE',  ( 24.51248951003896437, 3.604726614523240613, 161.7848665344110657 ) ) ;
#16139 = PRESENTATION_LAYER_ASSIGNMENT (  '', '', ( #26392 ) ) ;
#16140 = CARTESIAN_POINT ( 'NONE',  ( -54.54836230271183695, 202.5810206699313767, -4.149950860017804111 ) ) ;
#16141 = CARTESIAN_POINT ( 'NONE',  ( 26.75643035624999655, 245.9218750006145342, -7.049594010296217766E-16 ) ) ;
#16142 = DIRECTION ( 'NONE',  ( -0.000000000000000000, 0.000000000000000000, -1.000000000000000000 ) ) ;
#16143 = ADVANCED_FACE ( 'NONE', ( #16369 ), #22615, .F. ) ;
#16144 = CARTESIAN_POINT ( 'NONE',  ( -34.75669563604515844, 209.8844732041982297, -4.499999999999996447 ) ) ;
#16145 =( BOUNDED_CURVE ( )  B_SPLINE_CURVE ( 2, ( #20959, #32120, #34964, #14508, #19708, #8822, #17547 ),
 .UNSPECIFIED., .F., .F. ) 
 B_SPLINE_CURVE_WITH_KNOTS ( ( 3, 2, 2, 3 ),
 ( 0.8958333333333333703, 0.9027777777777777901, 0.9166666666666666297, 0.9258785558287927486 ),
 .UNSPECIFIED. ) 
 CURVE ( )  GEOMETRIC_REPRESENTATION_ITEM ( )  RATIONAL_B_SPLINE_CURVE ( ( 0.9330127018922192983, 0.9330127018922198534, 1.000000000000000000, 0.8660254037844387076, 1.000000000000000000, 0.9111405425767590271, 0.9401542252352144136 ) ) 
 REPRESENTATION_ITEM ( '' )  );
#16146 = CARTESIAN_POINT ( 'NONE',  ( 12.46528703574805874, 137.1976862821014720, 2.660918448318279950 ) ) ;
#16147 = CARTESIAN_POINT ( 'NONE',  ( 10.56230152254410903, 3.464101615137752166, -2.174999998770987375 ) ) ;
#16148 = ORIENTED_EDGE ( 'NONE', *, *, #29038, .T. ) ;
#16149 = DIRECTION ( 'NONE',  ( 0.000000000000000000, 0.000000000000000000, -1.000000000000000000 ) ) ;
#16150 = CARTESIAN_POINT ( 'NONE',  ( 15.00000000000000178, 244.6375000000000171, 3.464101615137757051 ) ) ;
#16151 = CARTESIAN_POINT ( 'NONE',  ( 8.927990412390657937, 117.0726862821014294, -13.04141134922759804 ) ) ;
#16152 = VECTOR ( 'NONE', #19557, 1000.000000000000000 ) ;
#16153 = CARTESIAN_POINT ( 'NONE',  ( 1.715153634034233487, 111.3226862821014578, 9.534712964251941258 ) ) ;
#16154 = CARTESIAN_POINT ( 'NONE',  ( 7.234628195640318005, 199.4174038105677198, -26.99999999999999645 ) ) ;
#16155 = CARTESIAN_POINT ( 'NONE',  ( -4.622313124798576922, 14.43518628210144250, -11.61527771782819762 ) ) ;
#16156 = CARTESIAN_POINT ( 'NONE',  ( 22.56230152254412147, -3.464101615137755275, -9.262500000000022382 ) ) ;
#16157 = EDGE_LOOP ( 'NONE', ( #12431, #31701, #5519, #31306 ) ) ;
#16158 = DIRECTION ( 'NONE',  ( -0.000000000000000000, -1.000000000000000000, -0.000000000000000000 ) ) ;
#16159 = CARTESIAN_POINT ( 'NONE',  ( -9.534712964251941258, 76.82268628210144357, 1.715153634034234154 ) ) ;
#16160 = FILL_AREA_STYLE ('',( #7995 ) ) ;
#16161 = CARTESIAN_POINT ( 'NONE',  ( 0.1745138560723095977, 123.7898137178985678, 9.500000000000005329 ) ) ;
#16162 = CARTESIAN_POINT ( 'NONE',  ( 27.24356964375000700, 196.3906250006145058, 15.72908226750537075 ) ) ;
#16163 = LINE ( 'NONE', #4950, #9914 ) ;
#16164 = CARTESIAN_POINT ( 'NONE',  ( 13.62178482187499640, 197.0093750006145399, -23.59362340125807123 ) ) ;
#16165 = CARTESIAN_POINT ( 'NONE',  ( 10.56230152254410903, 0.000000000000000000, 10.00000000000000000 ) ) ;
#16166 = CYLINDRICAL_SURFACE ( 'NONE', #25432, 6.000000000000005329 ) ;
#16167 = SHAPE_REPRESENTATION ( 'handle link', ( #17215 ), #9874 ) ;
#16168 = CARTESIAN_POINT ( 'NONE',  ( 9.534712964251900402, 57.37731371789855928, 1.715153634034445540 ) ) ;
#16169 = ORIENTED_EDGE ( 'NONE', *, *, #6580, .T. ) ;
#16170 = CARTESIAN_POINT ( 'NONE',  ( 24.00000000000000000, 241.6562500012290400, 5.196152422706629359 ) ) ;
#16171 = CARTESIAN_POINT ( 'NONE',  ( 12.53471296425189330, 75.77731371789856496, 2.311890736173451533 ) ) ;
#16172 = CARTESIAN_POINT ( 'NONE',  ( 10.31873187879410558, 3.604726614523240613, -5.634374999385534544 ) ) ;
#16173 = CARTESIAN_POINT ( 'NONE',  ( 27.24356964375000345, 199.5781250006145342, -3.336375036156643733E-15 ) ) ;
#16174 = CARTESIAN_POINT ( 'NONE',  ( 21.00000000000000000, -6.646953231504538984, -5.990624999385490312 ) ) ;
#16175 = CARTESIAN_POINT ( 'NONE',  ( -2.311890736173448424, 22.87731371789854151, 12.53471296425189330 ) ) ;
#16176 = EDGE_CURVE ( 'NONE', #16460, #5564, #14076, .T. ) ;
#16177 = ORIENTED_EDGE ( 'NONE', *, *, #11731, .T. ) ;
#16178 = CARTESIAN_POINT ( 'NONE',  ( 26.75643035624999655, 7.049594010296217766E-16, -7.565624999385455851 ) ) ;
#16179 = AXIS2_PLACEMENT_3D ( 'NONE', #23781, #35514, #6909 ) ;
#16180 = CARTESIAN_POINT ( 'NONE',  ( -4.944772684328673229, 20.18518628210144783, 11.48171059495397728 ) ) ;
#16181 = CARTESIAN_POINT ( 'NONE',  ( 34.48606902399273366, -5.407089921784861808, 168.3280104420172449 ) ) ;
#16182 = CARTESIAN_POINT ( 'NONE',  ( -49.79836230271183695, 204.3130714775002446, -3.149950860017828091 ) ) ;
#16183 = CARTESIAN_POINT ( 'NONE',  ( -7.234628195640354420, 196.4924038105676800, 26.99999999999996803 ) ) ;
#16184 = CARTESIAN_POINT ( 'NONE',  ( 8.962234695871567070, 58.23981371789854933, 8.715434833792127023 ) ) ;
#16185 = EDGE_CURVE ( 'NONE', #30240, #31488, #13338, .T. ) ;
#16186 = CARTESIAN_POINT ( 'NONE',  ( -49.21205436395490551, 213.2096571498974242, 3.378800118222489601 ) ) ;
#16187 = CARTESIAN_POINT ( 'NONE',  ( -58.71205436395488420, 214.6737587650352168, 4.842901733360204908 ) ) ;
#16188 = CARTESIAN_POINT ( 'NONE',  ( 16.56230152254410726, 0.000000000000000000, -10.00000000000000000 ) ) ;
#16189 = CARTESIAN_POINT ( 'NONE',  ( 22.56230152254428489, -3.464101615137663348, -6.112500000000050449 ) ) ;
#16190 = EDGE_CURVE ( 'NONE', #25502, #11580, #7836, .T. ) ;
#16191 = CARTESIAN_POINT ( 'NONE',  ( -15.46528703574811736, 33.80231371789854222, 3.257655550456946436 ) ) ;
#16192 = CARTESIAN_POINT ( 'NONE',  ( -49.20461230271185116, 207.6069050685336492, -8.469044688360751749 ) ) ;
#16193 = LINE ( 'NONE', #27743, #8674 ) ;
#16194 = CARTESIAN_POINT ( 'NONE',  ( 8.715434833791931624, 64.46018628210146062, 8.962234695871760692 ) ) ;
#16195 = CARTESIAN_POINT ( 'NONE',  ( 10.83675517735155225, 9.260186282101427580, 11.08355503943142573 ) ) ;
#16196 = CARTESIAN_POINT ( 'NONE',  ( 19.56230152254412502, -5.196152422706635576, -1.650000000000068079 ) ) ;
#16197 = DIRECTION ( 'NONE',  ( 0.08715574274765150453, 0.000000000000000000, 0.9961946980917461003 ) ) ;
#16198 = ORIENTED_EDGE ( 'NONE', *, *, #37122, .F. ) ;
#16199 = CARTESIAN_POINT ( 'NONE',  ( -15.50000000000000533, 21.91018628210143859, -0.1745138560725808530 ) ) ;
#16200 = AXIS2_PLACEMENT_3D ( 'NONE', #36555, #11712, #17416 ) ;
#16201 = CARTESIAN_POINT ( 'NONE',  ( 27.24356964374999279, 198.7156250006145513, -15.72908226750539207 ) ) ;
#16202 = CARTESIAN_POINT ( 'NONE',  ( -27.24356964374999635, 197.1968750006145115, 15.72908226750539384 ) ) ;
#16203 = CARTESIAN_POINT ( 'NONE',  ( -27.00000000000000355, 199.0999999999999943, 0.000000000000000000 ) ) ;
#16204 = CARTESIAN_POINT ( 'NONE',  ( 5.000000000000127010, 225.9999999999999432, 7.999999999999943157 ) ) ;
#16205 = DIRECTION ( 'NONE',  ( 0.000000000000000000, 0.000000000000000000, 1.000000000000000000 ) ) ;
#16206 = CARTESIAN_POINT ( 'NONE',  ( 2.660918448318279950, 6.097686282101443922, -12.46528703574805697 ) ) ;
#16207 = CARTESIAN_POINT ( 'NONE',  ( 23.87821517812500005, 248.6593750006145171, 4.985214923628404016 ) ) ;
#16208 = CARTESIAN_POINT ( 'NONE',  ( 9.534712964251900402, 103.3773137178985451, 1.715153634034445540 ) ) ;
#16209 = CARTESIAN_POINT ( 'NONE',  ( 26.75643035624999655, 243.3718750006145228, -3.323476615752271268 ) ) ;
#16210 = ORIENTED_EDGE ( 'NONE', *, *, #26275, .T. ) ;
#16211 = CARTESIAN_POINT ( 'NONE',  ( 20.99999999999999645, 241.1125000000000114, 5.999999999999998224 ) ) ;
#16212 = CARTESIAN_POINT ( 'NONE',  ( 8.962234695871567070, 141.0398137178985678, 8.715434833792127023 ) ) ;
#16213 = CARTESIAN_POINT ( 'NONE',  ( 16.56230152254411081, 7.209453229046475009, -8.803124999385520510 ) ) ;
#16214 = CARTESIAN_POINT ( 'NONE',  ( 31.02481694790609268, -7.209453229046475009, 164.5841820401837765 ) ) ;
#16215 = CARTESIAN_POINT ( 'NONE',  ( 8.562301522544109034, 9.797174393178823685E-16, -10.00000000000000000 ) ) ;
#16216 = CARTESIAN_POINT ( 'NONE',  ( -27.00000000000000355, 197.2624999999999886, -15.58845726811989429 ) ) ;
#16217 = ORIENTED_EDGE ( 'NONE', *, *, #19583, .T. ) ;
#16218 = CARTESIAN_POINT ( 'NONE',  ( -11.61527771782819940, 30.53518628210144570, 4.622313124798574258 ) ) ;
#16219 = ORIENTED_EDGE ( 'NONE', *, *, #3678, .F. ) ;
#16220 = VERTEX_POINT ( 'NONE', #11226 ) ;
#16221 = CARTESIAN_POINT ( 'NONE',  ( 26.99999999999999645, 3.464101615137755275, -5.981249998770952203 ) ) ;
#16222 = CARTESIAN_POINT ( 'NONE',  ( -77.00000000000002842, 210.0000000000000000, -3.000000000000000000 ) ) ;
#16223 = CARTESIAN_POINT ( 'NONE',  ( -7.234628195640302017, 199.3049038117967200, 27.00000000000000711 ) ) ;
#16224 = CARTESIAN_POINT ( 'NONE',  ( 26.97716818855048260, 0.000000000000000000, 49.47706554351410801 ) ) ;
#16225 = CARTESIAN_POINT ( 'NONE',  ( 26.75643035624999655, 7.049594010296217766E-16, -8.915624999385475036 ) ) ;
#16226 = CARTESIAN_POINT ( 'NONE',  ( -4.622313124798576922, 69.63518628210145778, -11.61527771782819762 ) ) ;
#16227 = CARTESIAN_POINT ( 'NONE',  ( 15.46528703574811736, 10.80231371789855466, -3.257655550456947768 ) ) ;
#16228 = ADVANCED_FACE ( 'NONE', ( #30768 ), #2324, .T. ) ;
#16229 = CARTESIAN_POINT ( 'NONE',  ( -61.27752896937850124, 213.3500491399821613, 5.571401726697954970 ) ) ;
#16230 = CARTESIAN_POINT ( 'NONE',  ( 15.07698242245262144, 225.7947135401293792, 0.9779651927385701882 ) ) ;
#16231 = CARTESIAN_POINT ( 'NONE',  ( -58.11086230271183695, 212.1499508600178387, -3.954877714930852495 ) ) ;
#16232 = SURFACE_SIDE_STYLE ('',( #16418 ) ) ;
#16233 = VECTOR ( 'NONE', #30462, 1000.000000000000000 ) ;
#16234 = CARTESIAN_POINT ( 'NONE',  ( 34.11717084844381986, -5.196152422706629359, 165.5088091249684510 ) ) ;
#16235 = CARTESIAN_POINT ( 'NONE',  ( -12.53471296425189152, 126.3773137178985593, -2.311890736173453753 ) ) ;
#16236 = CARTESIAN_POINT ( 'NONE',  ( -50.20163769728823411, 215.6869285224996986, -3.149950860017881382 ) ) ;
#16238 = EDGE_CURVE ( 'NONE', #30702, #29886, #23329, .T. ) ;
#16237 = CARTESIAN_POINT ( 'NONE',  ( -56.33705436395490551, 203.8621396198270475, -6.307003348497942419 ) ) ;
#16239 = CARTESIAN_POINT ( 'NONE',  ( 15.24356964374999990, 3.323476615752268604, -2.990624999385476102 ) ) ;
#16240 = CARTESIAN_POINT ( 'NONE',  ( -27.24356964374999635, 196.6906250006145456, 15.72908226750539384 ) ) ;
#16241 = VECTOR ( 'NONE', #6267, 1000.000000000000000 ) ;
#16242 = CARTESIAN_POINT ( 'NONE',  ( 0.1745138560722461762, 96.18981371789855928, 15.50000000000000533 ) ) ;
#16243 = CARTESIAN_POINT ( 'NONE',  ( -42.87127896937850124, 216.5309553116391612, 1.626142955000506873 ) ) ;
#16244 = VERTEX_POINT ( 'NONE', #1944 ) ;
#16245 = DIRECTION ( 'NONE',  ( -0.000000000000000000, 1.000000000000000000, -0.000000000000000000 ) ) ;
#16246 = CARTESIAN_POINT ( 'NONE',  ( 12.46528703574805874, 127.9976862821014407, 2.660918448318279950 ) ) ;
#16247 = CARTESIAN_POINT ( 'NONE',  ( -6.092822981423970496, 75.38518628210142936, 14.25334919248782661 ) ) ;
#16248 = CARTESIAN_POINT ( 'NONE',  ( 25.44556919728433542, -3.464101615137774814, 169.6553679145326612 ) ) ;
#16249 = CARTESIAN_POINT ( 'NONE',  ( 30.96108431102187808, 7.209453229046482114, 163.8557146672041824 ) ) ;
#16250 = CARTESIAN_POINT ( 'NONE',  ( 2.908627838312118019, 92.92268628210145209, 15.53471296425195369 ) ) ;
#16251 = CARTESIAN_POINT ( 'NONE',  ( -53.96205436395489130, 214.6737587650351884, 4.842901733360205796 ) ) ;
#16252 = CARTESIAN_POINT ( 'NONE',  ( 13.44051670066911619, -5.407089921784859143, -5.015624999385570604 ) ) ;
#16253 = CARTESIAN_POINT ( 'NONE',  ( -8.710071997420127943, 31.68518628210144428, -3.796722387233380402 ) ) ;
#16254 = CARTESIAN_POINT ( 'NONE',  ( 26.99999999999999645, 7.347880794884117764E-16, -6.918749998770956644 ) ) ;
#16255 = CARTESIAN_POINT ( 'NONE',  ( -62.86830436395490551, 209.8844732041982581, 6.500000000000000888 ) ) ;
#16256 = CARTESIAN_POINT ( 'NONE',  ( -12.46528703574805697, 49.79768628210145209, -2.660918448318280838 ) ) ;
#16257 = CARTESIAN_POINT ( 'NONE',  ( 24.00000000000000000, -5.196152422706629359, -7.893749998770960730 ) ) ;
#16258 = AXIS2_PLACEMENT_3D ( 'NONE', #14014, #31996, #25564 ) ;
#16259 = CARTESIAN_POINT ( 'NONE',  ( -47.00000000000000711, 244.5000000000000000, 5.000000000000000000 ) ) ;
#16261 = CARTESIAN_POINT ( 'NONE',  ( 10.31873187879410914, 0.000000000000000000, -1.996874999385528371 ) ) ;
#16260 = CARTESIAN_POINT ( 'NONE',  ( 8.152565276336714462, 53.24768628210144783, -5.233372021372432847 ) ) ;
#16262 = CARTESIAN_POINT ( 'NONE',  ( 0.3500000000000069722, 244.5000000000000000, 5.000000000000000000 ) ) ;
#16263 = EDGE_LOOP ( 'NONE', ( #2911, #1637, #1981, #4167, #21374 ) ) ;
#16264 = CARTESIAN_POINT ( 'NONE',  ( 26.99999999999999645, -3.464101615137751278, -1.612499999999998046 ) ) ;
#16265 = CARTESIAN_POINT ( 'NONE',  ( 27.85444716323975101, 5.407089921784862696, 164.1651534432314747 ) ) ;
#16266 = CARTESIAN_POINT ( 'NONE',  ( 24.69711925643884598, 0.000000000000000000, 161.1005459446697614 ) ) ;
#16267 =( BOUNDED_CURVE ( )  B_SPLINE_CURVE ( 2, ( #22776, #14422, #11203, #11764, #23147, #8736, #28813, #20116, #34881 ),
 .UNSPECIFIED., .F., .F. ) 
 B_SPLINE_CURVE_WITH_KNOTS ( ( 3, 2, 2, 2, 3 ),
 ( 0.8369565217391303769, 0.8405797101449274944, 0.8478260869565217295, 0.8550724637681159646, 0.8586956521739130821 ),
 .UNSPECIFIED. ) 
 CURVE ( )  GEOMETRIC_REPRESENTATION_ITEM ( )  RATIONAL_B_SPLINE_CURVE ( ( 0.9330127018922192983, 0.9330127018922182991, 1.000000000000000000, 0.8660254037844387076, 1.000000000000000000, 0.8660254037844387076, 1.000000000000000000, 0.9330127018922194093, 0.9330127018922194093 ) ) 
 REPRESENTATION_ITEM ( '' )  );
#16268 = CARTESIAN_POINT ( 'NONE',  ( 15.00000000000000000, 246.8125000000000000, -3.464101615137752166 ) ) ;
#16269 = CARTESIAN_POINT ( 'NONE',  ( 1.069080835302379631E-14, 198.7624999999999886, 27.00000000000000000 ) ) ;
#16270 = CARTESIAN_POINT ( 'NONE',  ( 8.962234695871567070, 85.83981371789856496, 8.715434833792127023 ) ) ;
#16271 = CARTESIAN_POINT ( 'NONE',  ( 2.660918448318279950, 88.89768628210146062, -12.46528703574805874 ) ) ;
#16272 = ORIENTED_EDGE ( 'NONE', *, *, #19380, .F. ) ;
#16273 = VECTOR ( 'NONE', #19127, 1000.000000000000000 ) ;
#16274 = EDGE_LOOP ( 'NONE', ( #25786, #19217, #28502 ) ) ;
#16275 = CARTESIAN_POINT ( 'NONE',  ( -1.909035429704832693E-15, 197.3000000012290513, -31.17691453623979214 ) ) ;
#16276 = CARTESIAN_POINT ( 'NONE',  ( 25.24620043574905282, 0.000000000000000000, 167.3765725426477502 ) ) ;
#16277 = CARTESIAN_POINT ( 'NONE',  ( -2.908627838312453306, 59.67731371789855643, 15.53471296425188797 ) ) ;
#16278 = CARTESIAN_POINT ( 'NONE',  ( 15.24356964374999990, 0.000000000000000000, -7.453124999385495997 ) ) ;
#16279 = CARTESIAN_POINT ( 'NONE',  ( 18.12178482187500350, 244.0843750006145285, 4.985214923628407568 ) ) ;
#16280 = CARTESIAN_POINT ( 'NONE',  ( -59.30580436395490551, 214.5000000000000284, 0.1155267958017899832 ) ) ;
#16281 = CARTESIAN_POINT ( 'NONE',  ( -8.710071997420207879, 42.71481371789855075, 3.796722387233182339 ) ) ;
#16282 = CARTESIAN_POINT ( 'NONE',  ( 22.80587116629410360, 3.604726614523238837, -7.078124999385530636 ) ) ;
#16283 = AXIS2_PLACEMENT_3D ( 'NONE', #36912, #28388, #14185 ) ;
#16284 = CARTESIAN_POINT ( 'NONE',  ( 8.152565276336593669, 94.75231371789854506, 5.233372021372610483 ) ) ;
#16285 = CARTESIAN_POINT ( 'NONE',  ( -13.62178482187500528, 197.9843750006145626, -23.59362340125807123 ) ) ;
#16286 = CARTESIAN_POINT ( 'NONE',  ( 12.50000000000000355, 11.08981371789855075, -0.1745138560722771515 ) ) ;
#16287 = CARTESIAN_POINT ( 'NONE',  ( -0.1745138560725500443, 74.81018628210145494, 12.50000000000000355 ) ) ;
#16288 = CARTESIAN_POINT ( 'NONE',  ( 22.56230152254410726, 7.347880794884117764E-16, -9.112499998771033560 ) ) ;
#16289 = DIRECTION ( 'NONE',  ( -0.000000000000000000, 1.000000000000000000, -0.000000000000000000 ) ) ;
#16290 = CARTESIAN_POINT ( 'NONE',  ( 24.48144027668511669, 0.000000000000000000, 161.4299721732159014 ) ) ;
#16291 = CARTESIAN_POINT ( 'NONE',  ( 23.99999999999999645, 5.196152422706631135, -0.9937499987709430549 ) ) ;
#16292 = CARTESIAN_POINT ( 'NONE',  ( 22.80587116629411426, -3.604726614523238837, -6.309374999385513050 ) ) ;
#16293 = CARTESIAN_POINT ( 'NONE',  ( 0.000000000000000000, 200.0000000000000000, -27.00000000000000355 ) ) ;
#16294 = CARTESIAN_POINT ( 'NONE',  ( 8.152565276336714462, 99.24768628210145494, -5.233372021372432847 ) ) ;
#16295 = DIRECTION ( 'NONE',  ( -0.000000000000000000, -0.000000000000000000, -1.000000000000000000 ) ) ;
#16296 = CARTESIAN_POINT ( 'NONE',  ( -12.50000000000000355, 104.7101862821014606, -0.1745138560725492671 ) ) ;
#16297 = CARTESIAN_POINT ( 'NONE',  ( -8.655134159629936264, 143.0000000000000284, 7.486361052592569010 ) ) ;
#16298 = CARTESIAN_POINT ( 'NONE',  ( 18.12178482187500350, 249.0343750006145456, 4.985214923628407568 ) ) ;
#16299 = ORIENTED_EDGE ( 'NONE', *, *, #7794, .F. ) ;
#16300 = CARTESIAN_POINT ( 'NONE',  ( 24.75598086634022010, 0.000000000000000000, 164.5679854722048958 ) ) ;
#16301 = CARTESIAN_POINT ( 'NONE',  ( 21.00000000000000000, -6.646953231504538984, -5.428124999385471661 ) ) ;
#16302 = CARTESIAN_POINT ( 'NONE',  ( -1.926257025242585782E-15, 198.8468750006145740, -31.45816453501076637 ) ) ;
#16303 = CARTESIAN_POINT ( 'NONE',  ( 17.39339328860229728, 4.563019727067374909, -8.000000000000001776 ) ) ;
#16304 = CARTESIAN_POINT ( 'NONE',  ( 31.37044394018619542, 6.928203230275514990, 168.5347166391916574 ) ) ;
#16305 = CARTESIAN_POINT ( 'NONE',  ( 24.69711925643884598, 0.000000000000000000, 161.1005459446697614 ) ) ;
#16306 = CARTESIAN_POINT ( 'NONE',  ( 18.12178482187500350, 244.0843750006145285, 4.985214923628407568 ) ) ;
#16307 = FACE_OUTER_BOUND ( 'NONE', #25109, .T. ) ;
#16308 = ADVANCED_FACE ( 'NONE', ( #33609 ), #13712, .F. ) ;
#16309 = CARTESIAN_POINT ( 'NONE',  ( -11.48171059495408208, 143.9148137178985678, 4.944772684328421875 ) ) ;
#16310 = CARTESIAN_POINT ( 'NONE',  ( -8.962234695871760692, 140.3601862821014379, 8.715434833791933400 ) ) ;
#16312 = ORIENTED_EDGE ( 'NONE', *, *, #10287, .T. ) ;
#16311 = EDGE_LOOP ( 'NONE', ( #20225, #27821, #8843, #7923 ) ) ;
#16313 = CARTESIAN_POINT ( 'NONE',  ( 23.87821517812500005, 244.0468750006145058, 4.985214923628404016 ) ) ;
#16314 = CARTESIAN_POINT ( 'NONE',  ( 15.02283181144952628, 7.347880794884122694E-16, 50.52293445648592751 ) ) ;
#16315 = CARTESIAN_POINT ( 'NONE',  ( 21.00000000000000000, -6.646953231504538984, -4.978124999385476812 ) ) ;
#16316 = CARTESIAN_POINT ( 'NONE',  ( -10.83675517735179028, 106.5398137178985536, 11.08355503943118947 ) ) ;
#16317 = CARTESIAN_POINT ( 'NONE',  ( 23.99999999999999645, 5.196152422706631135, -9.993749998770951493 ) ) ;
#16318 = CARTESIAN_POINT ( 'NONE',  ( 19.68408634441912142, -5.407089921784861808, -8.146874999385516958 ) ) ;
#16319 =( BOUNDED_CURVE ( )  B_SPLINE_CURVE ( 2, ( #2565, #5584, #17170, #33853, #5223, #28712, #14320 ),
 .UNSPECIFIED., .F., .F. ) 
 B_SPLINE_CURVE_WITH_KNOTS ( ( 3, 2, 2, 3 ),
 ( 0.5434782608695641892, 0.5507246376811585353, 0.5579710144927527704, 0.5652173913043470055 ),
 .UNSPECIFIED. ) 
 CURVE ( )  GEOMETRIC_REPRESENTATION_ITEM ( )  RATIONAL_B_SPLINE_CURVE ( ( 1.000000000000018430, 0.8660254037844202779, 1.000000000000000000, 0.8660254037844387076, 1.000000000000000000, 0.8660254037844530295, 0.9999999999999856781 ) ) 
 REPRESENTATION_ITEM ( '' )  );
#16320 = ORIENTED_EDGE ( 'NONE', *, *, #26959, .F. ) ;
#16321 = CARTESIAN_POINT ( 'NONE',  ( -27.00000000000000355, 198.7625000012290286, 0.000000000000000000 ) ) ;
#16322 = CARTESIAN_POINT ( 'NONE',  ( 8.715434833791931624, 119.6601862821014493, 8.962234695871760692 ) ) ;
#16323 = CARTESIAN_POINT ( 'NONE',  ( 19.68408634441910721, 5.407089921784857367, -1.640624999385525973 ) ) ;
#16324 = EDGE_CURVE ( 'NONE', #29619, #20388, #31090, .T. ) ;
#16325 = CARTESIAN_POINT ( 'NONE',  ( -45.84002896937850124, 202.6965474657332038, 4.350049139982197666 ) ) ;
#16326 = CARTESIAN_POINT ( 'NONE',  ( 18.12178482187500350, 243.9718750006145171, 4.985214923628407568 ) ) ;
#16327 = DIRECTION ( 'NONE',  ( 4.130293990420971855E-17, -1.000000000000000000, 0.000000000000000000 ) ) ;
#16328 = CARTESIAN_POINT ( 'NONE',  ( -37.13169563604516554, 210.1155267958017703, 4.499999999999996447 ) ) ;
#16329 = CARTESIAN_POINT ( 'NONE',  ( -11.61527771782819940, 140.9351862821014834, 4.622313124798574258 ) ) ;
#16330 = CARTESIAN_POINT ( 'NONE',  ( 22.56230152254410370, -3.464101615137751278, -2.399999998770968812 ) ) ;
#16332 = ORIENTED_EDGE ( 'NONE', *, *, #15497, .T. ) ;
#16331 = EDGE_CURVE ( 'NONE', #8598, #6593, #28884, .T. ) ;
#16333 = DIRECTION ( 'NONE',  ( 0.000000000000000000, 0.000000000000000000, 1.000000000000000000 ) ) ;
#16334 = CARTESIAN_POINT ( 'NONE',  ( 20.99999999999995381, 244.7125000000000057, 5.999999999999998224 ) ) ;
#16335 = CARTESIAN_POINT ( 'NONE',  ( 8.632099005475504683, 119.9476862821014294, 13.23911966647218996 ) ) ;
#16336 = CARTESIAN_POINT ( 'NONE',  ( 27.00000000000001421, 197.9375000000000284, 15.58845726811988897 ) ) ;
#16337 = CARTESIAN_POINT ( 'NONE',  ( -4.622313124798576922, 5.235186282101428112, -11.61527771782819762 ) ) ;
#16338 = CARTESIAN_POINT ( 'NONE',  ( 22.56230152254411436, 3.464101615137759271, -8.287500000000068923 ) ) ;
#16339 = EDGE_LOOP ( 'NONE', ( #29976, #36526, #5293, #16687 ) ) ;
#16340 = DIRECTION ( 'NONE',  ( 0.000000000000000000, 0.000000000000000000, 1.000000000000000000 ) ) ;
#16341 = CARTESIAN_POINT ( 'NONE',  ( 9.465287035748067623, 81.99768628210142651, 2.064181346179272847 ) ) ;
#16342 = DIRECTION ( 'NONE',  ( -0.000000000000000000, -1.000000000000000000, -0.000000000000000000 ) ) ;
#16343 = CARTESIAN_POINT ( 'NONE',  ( -3.474262827703527901, 133.5648137178985735, 8.843639120294245259 ) ) ;
#16344 = CARTESIAN_POINT ( 'NONE',  ( 27.24356964375000345, 195.5281250006145228, -3.336375036156643733E-15 ) ) ;
#16345 = CARTESIAN_POINT ( 'NONE',  ( 20.99999999999999289, 244.9374999999999716, -5.999999999999997335 ) ) ;
#16346 = CARTESIAN_POINT ( 'NONE',  ( 27.24356964374999635, 198.7718750006145569, -15.72908226750539029 ) ) ;
#16347 = CARTESIAN_POINT ( 'NONE',  ( -56.70466238434234185, 244.2363183625454894, 2.500000000000000000 ) ) ;
#16348 = CARTESIAN_POINT ( 'NONE',  ( 22.56230152254410370, 7.347880794884117764E-16, -6.862499998771004250 ) ) ;
#16349 = CARTESIAN_POINT ( 'NONE',  ( 6.594114490232462877, 55.93981371789855217, -6.840914352311949109 ) ) ;
#16350 = CARTESIAN_POINT ( 'NONE',  ( 18.00000000000000000, 5.196152422706630247, -9.525000000000005684 ) ) ;
#16351 = ORIENTED_EDGE ( 'NONE', *, *, #27045, .F. ) ;
#16352 = CARTESIAN_POINT ( 'NONE',  ( 26.99999999999999645, 241.2812500012290400, -7.347880794884117764E-16 ) ) ;
#16353 = CARTESIAN_POINT ( 'NONE',  ( -12.46528703574811558, 70.60231371789855359, 2.660918448318004170 ) ) ;
#16354 = ADVANCED_FACE ( 'NONE', ( #23351 ), #8946, .T. ) ;
#16355 = CARTESIAN_POINT ( 'NONE',  ( 19.68408634441912142, -5.407089921784861808, -6.796874999385527083 ) ) ;
#16356 = CARTESIAN_POINT ( 'NONE',  ( 27.24356964375000700, 198.6406250006145058, 15.72908226750537075 ) ) ;
#16357 = CARTESIAN_POINT ( 'NONE',  ( 23.87821517812499650, 4.985214923628404904, -6.703124999385495997 ) ) ;
#16358 = CARTESIAN_POINT ( 'NONE',  ( 10.49813415416005213, 37.82731371789854791, -7.228626920338837358 ) ) ;
#16359 = ORIENTED_EDGE ( 'NONE', *, *, #13888, .T. ) ;
#16360 = CARTESIAN_POINT ( 'NONE',  ( 22.80587116629411426, 7.646167579472024665E-16, -2.221874999385531346 ) ) ;
#16361 = CARTESIAN_POINT ( 'NONE',  ( 10.49813415415989581, 8.972686282101431487, 7.228626920339068285 ) ) ;
#16362 = ADVANCED_FACE ( 'NONE', ( #32059, #6088 ), #17672, .F. ) ;
#16363 =( BOUNDED_CURVE ( )  B_SPLINE_CURVE ( 2, ( #25422, #36974, #13489, #11018, #22592, #34138, #25605 ),
 .UNSPECIFIED., .F., .F. ) 
 B_SPLINE_CURVE_WITH_KNOTS ( ( 3, 2, 2, 3 ),
 ( 0.1739130434782631685, 0.1811594202898574590, 0.1884057971014517219, 0.1956521739130460125 ),
 .UNSPECIFIED. ) 
 CURVE ( )  GEOMETRIC_REPRESENTATION_ITEM ( )  RATIONAL_B_SPLINE_CURVE ( ( 0.9999999999999574785, 0.8660254037844813402, 1.000000000000000000, 0.8660254037844387076, 1.000000000000000000, 0.8660254037843919672, 1.000000000000046629 ) ) 
 REPRESENTATION_ITEM ( '' )  );
#16364 = CARTESIAN_POINT ( 'NONE',  ( -31.39211230271182629, 203.5309553116391896, 1.857196546604092724 ) ) ;
#16365 = VECTOR ( 'NONE', #9528, 1000.000000000000000 ) ;
#16366 = CARTESIAN_POINT ( 'NONE',  ( -54.15252896937850124, 206.6499508600178387, -5.571401726697954970 ) ) ;
#16367 = APPLICATION_PROTOCOL_DEFINITION ( 'draft international standard', 'automotive_design', 1998, #19027 ) ;
#16368 = ADVANCED_FACE ( 'NONE', ( #26369 ), #20701, .F. ) ;
#16369 = FACE_OUTER_BOUND ( 'NONE', #222, .T. ) ;
#16370 = CARTESIAN_POINT ( 'NONE',  ( 8.715434833792128799, 65.13981371789854791, -8.962234695871567070 ) ) ;
#16371 = CARTESIAN_POINT ( 'NONE',  ( -38.32663769728823411, 206.0451222850691408, 2.149950860017832532 ) ) ;
#16372 = CARTESIAN_POINT ( 'NONE',  ( -54.15997103062156981, 215.5714017266979852, 3.350049139982118618 ) ) ;
#16373 = CARTESIAN_POINT ( 'NONE',  ( 18.00000000000000000, 5.196152422706630247, -6.824999999999997513 ) ) ;
#16374 = CARTESIAN_POINT ( 'NONE',  ( 2.999999999999997335, 237.0000000000000000, 2.500000000000000000 ) ) ;
#16375 = CARTESIAN_POINT ( 'NONE',  ( -8.632099005475794229, 32.65231371789855075, 13.23911966647199812 ) ) ;
#16376 = CARTESIAN_POINT ( 'NONE',  ( -30.00669563604516554, 209.8844732041981729, -8.500000000000003553 ) ) ;
#16377 = CARTESIAN_POINT ( 'NONE',  ( 10.49813415415989581, 27.37268628210144783, 7.228626920339068285 ) ) ;
#16378 = DIRECTION ( 'NONE',  ( 0.000000000000000000, 0.000000000000000000, 1.000000000000000000 ) ) ;
#16379 = CARTESIAN_POINT ( 'NONE',  ( 2.660918448318279950, 61.29768628210143788, -12.46528703574805697 ) ) ;
#16380 = CARTESIAN_POINT ( 'NONE',  ( 10.83675517735155225, 18.46018628210144286, 11.08355503943142573 ) ) ;
#16382 = EDGE_CURVE ( 'NONE', #22329, #36867, #2733, .T. ) ;
#16381 = CARTESIAN_POINT ( 'NONE',  ( 22.56230152254412147, -3.464101615137755275, -1.612500000000030020 ) ) ;
#16383 =( BOUNDED_CURVE ( )  B_SPLINE_CURVE ( 2, ( #36720, #34066, #33508, #1667, #36529, #30491, #1853, #18755, #30297 ),
 .UNSPECIFIED., .F., .F. ) 
 B_SPLINE_CURVE_WITH_KNOTS ( ( 3, 2, 2, 2, 3 ),
 ( 0.5625000000000000000, 0.5694444444444444198, 0.5833333333333333703, 0.5972222222222222099, 0.6041666666666667407 ),
 .UNSPECIFIED. ) 
 CURVE ( )  GEOMETRIC_REPRESENTATION_ITEM ( )  RATIONAL_B_SPLINE_CURVE ( ( 0.9330127018922194093, 0.9330127018922194093, 1.000000000000000000, 0.8660254037844387076, 1.000000000000000000, 0.8660254037844387076, 1.000000000000000000, 0.9330127018922187432, 0.9330127018922192983 ) ) 
 REPRESENTATION_ITEM ( '' )  );
#16384 = CARTESIAN_POINT ( 'NONE',  ( -29.00000000000001066, 202.0000000000000000, -0.5248785063507624971 ) ) ;
#16385 = VERTEX_POINT ( 'NONE', #29405 ) ;
#16386 = CARTESIAN_POINT ( 'NONE',  ( -6.092822981423970496, 29.38518628210144712, 14.25334919248782661 ) ) ;
#16387 = CARTESIAN_POINT ( 'NONE',  ( -27.24356964375000345, 195.7531250006145456, 0.000000000000000000 ) ) ;
#16388 = CARTESIAN_POINT ( 'NONE',  ( -27.24356964374999635, 198.0968750006145456, 15.72908226750539384 ) ) ;
#16389 = DIRECTION ( 'NONE',  ( -1.000000000000000000, 0.000000000000000000, 0.000000000000000000 ) ) ;
#16390 = CARTESIAN_POINT ( 'NONE',  ( 26.99999999999999645, 195.4250000012290229, -15.58845726811990495 ) ) ;
#16391 = CARTESIAN_POINT ( 'NONE',  ( -26.99999999999999645, 195.0875000000000341, 15.58845726811991561 ) ) ;
#16392 = CARTESIAN_POINT ( 'NONE',  ( 4.622313124798573369, 9.835186282101449962, 11.61527771782819940 ) ) ;
#16393 = CARTESIAN_POINT ( 'NONE',  ( 15.24356964375000167, 247.6468750006145569, 3.323476615752272600 ) ) ;
#16394 = CARTESIAN_POINT ( 'NONE',  ( 2.064181346179061460, 105.1023137178985678, 9.465287035748106703 ) ) ;
#16395 = CARTESIAN_POINT ( 'NONE',  ( 18.12178482187499640, 243.0343750006145456, -4.985214923628404904 ) ) ;
#16396 = ORIENTED_EDGE ( 'NONE', *, *, #19461, .T. ) ;
#16397 = CARTESIAN_POINT ( 'NONE',  ( 26.99999999999999645, 248.4812500012290570, -7.347880794884117764E-16 ) ) ;
#16398 = EDGE_CURVE ( 'NONE', #815, #11530, #23730, .T. ) ;
#16399 = CARTESIAN_POINT ( 'NONE',  ( -12.46528703574811558, 125.8023137178985706, 2.660918448318004170 ) ) ;
#16400 = CARTESIAN_POINT ( 'NONE',  ( 10.31873187879411269, 0.000000000000000000, -10.04062499938554431 ) ) ;
#16401 = CARTESIAN_POINT ( 'NONE',  ( 36.94394061169700905, 3.604726614523238837, 160.6031473820695226 ) ) ;
#16402 = CARTESIAN_POINT ( 'NONE',  ( 15.24356964374999990, 3.323476615752268604, -0.7406249993854975289 ) ) ;
#16403 = CARTESIAN_POINT ( 'NONE',  ( -1.909035429704832693E-15, 198.0875000000000341, -31.17691453623979214 ) ) ;
#16404 = ORIENTED_EDGE ( 'NONE', *, *, #19300, .T. ) ;
#16405 = CARTESIAN_POINT ( 'NONE',  ( 10.49813415415989581, 27.37268628210144783, 7.228626920339069173 ) ) ;
#16406 = ORIENTED_EDGE ( 'NONE', *, *, #34019, .T. ) ;
#16407 = VERTEX_POINT ( 'NONE', #968 ) ;
#16408 = CARTESIAN_POINT ( 'NONE',  ( 24.00000000000000000, -5.196152422706629359, -5.193749998770952558 ) ) ;
#16409 = CARTESIAN_POINT ( 'NONE',  ( 23.87821517812500005, -4.985214923628404016, -0.8906249993854697955 ) ) ;
#16410 = CARTESIAN_POINT ( 'NONE',  ( 27.80663194388356629, 5.196152422706630247, 162.2212988612534730 ) ) ;
#16411 = CARTESIAN_POINT ( 'NONE',  ( 21.00000000000000000, 248.9593750006145285, 6.646953231504538984 ) ) ;
#16412 = CARTESIAN_POINT ( 'NONE',  ( -4.944772684328673229, 84.58518628210146062, 11.48171059495397728 ) ) ;
#16413 = CARTESIAN_POINT ( 'NONE',  ( 14.25334919248782661, 137.4851862821014379, 6.092822981423971385 ) ) ;
#16414 = CARTESIAN_POINT ( 'NONE',  ( -65.43377896937850835, 208.3738570449995109, 6.530955311639247363 ) ) ;
#16415 = CARTESIAN_POINT ( 'NONE',  ( 15.07698242245260722, 225.7947135401219612, -0.9779651927385025756 ) ) ;
#16416 = CARTESIAN_POINT ( 'NONE',  ( -52.96502896937850124, 213.8393509191290889, -2.350049139982142155 ) ) ;
#16417 = EDGE_CURVE ( 'NONE', #36062, #4383, #6663, .T. ) ;
#16418 = SURFACE_STYLE_FILL_AREA ( #22477 ) ;
#16419 = CARTESIAN_POINT ( 'NONE',  ( 33.99951059573448475, -5.196152422706629359, 164.1639462825446003 ) ) ;
#16420 = CARTESIAN_POINT ( 'NONE',  ( 8.715434833792128799, 120.3398137178985650, -8.962234695871567070 ) ) ;
#16421 = CARTESIAN_POINT ( 'NONE',  ( -39.51413769728823411, 213.1499508600178672, 5.686928522499718142 ) ) ;
#16422 = CARTESIAN_POINT ( 'NONE',  ( -62.07663769728824121, 202.5810206699313767, 4.149950860017909804 ) ) ;
#16423 = AXIS2_PLACEMENT_3D ( 'NONE', #5991, #17570, #14717 ) ;
#16424 = CARTESIAN_POINT ( 'NONE',  ( 23.87821517812499650, 4.985214923628404904, -2.653124999385497951 ) ) ;
#16425 = CARTESIAN_POINT ( 'NONE',  ( 27.24356964374999635, 196.0156250006145626, -15.72908226750539029 ) ) ;
#16426 = CARTESIAN_POINT ( 'NONE',  ( -3.257655550456946880, 91.30231371789854222, -15.46528703574811736 ) ) ;
#16427 = CARTESIAN_POINT ( 'NONE',  ( -41.28794563604515133, 205.3262412349647832, 4.842901733360250205 ) ) ;
#16428 = ORIENTED_EDGE ( 'NONE', *, *, #13178, .T. ) ;
#16429 = DIRECTION ( 'NONE',  ( -1.000000000000000000, 0.000000000000000000, 0.000000000000000000 ) ) ;
#16430 = CARTESIAN_POINT ( 'NONE',  ( 12.46528703574805874, 118.7976862821014663, 2.660918448318279950 ) ) ;
#16431 = CARTESIAN_POINT ( 'NONE',  ( 13.23911966647218996, 71.64768628210146062, -8.632099005475504683 ) ) ;
#16432 = DIRECTION ( 'NONE',  ( 0.000000000000000000, 1.000000000000000000, 0.000000000000000000 ) ) ;
#16433 = CARTESIAN_POINT ( 'NONE',  ( 27.97210741594907901, 5.407089921784862696, 165.5100162856553538 ) ) ;
#16434 = CARTESIAN_POINT ( 'NONE',  ( -11.08355503943142573, 85.16018628210146346, 10.83675517735155402 ) ) ;
#16435 = CARTESIAN_POINT ( 'NONE',  ( -55.94122103062156981, 208.3738570449994256, -6.530955311639227823 ) ) ;
#16436 = EDGE_CURVE ( 'NONE', #21538, #21530, #9756, .T. ) ;
#16437 = CARTESIAN_POINT ( 'NONE',  ( 13.44051670066911086, 5.407089921784856479, -6.515624999385543958 ) ) ;
#16438 = CARTESIAN_POINT ( 'NONE',  ( -8.843639120294326972, 39.73518628210145209, 3.474262827703335166 ) ) ;
#16439 = EDGE_CURVE ( 'NONE', #25531, #14300, #15364, .T. ) ;
#16440 = DIRECTION ( 'NONE',  ( -0.000000000000000000, -1.000000000000000000, -0.000000000000000000 ) ) ;
#16441 = CARTESIAN_POINT ( 'NONE',  ( -62.27455436395490551, 205.1570982666397356, 4.673758765035198159 ) ) ;
#16442 = SURFACE_STYLE_FILL_AREA ( #31391 ) ;
#16443 = CARTESIAN_POINT ( 'NONE',  ( -2.660918448318275509, 65.89768628210146062, 12.46528703574805874 ) ) ;
#16444 = CARTESIAN_POINT ( 'NONE',  ( -1.909035429704832693E-15, 198.9875000000000114, -31.17691453623979214 ) ) ;
#16445 = PLANE ( 'NONE',  #23251 ) ;
#16447 = CARTESIAN_POINT ( 'NONE',  ( 13.44051670066911086, 5.407089921784862696, -1.621874999385541916 ) ) ;
#16446 = CARTESIAN_POINT ( 'NONE',  ( -9.465287035748065847, 31.39768628210144286, -2.064181346179273735 ) ) ;
#16448 = CARTESIAN_POINT ( 'NONE',  ( 15.00000000000021316, -3.464101615137879620, -6.206249998770965171 ) ) ;
#16449 = ORIENTED_EDGE ( 'NONE', *, *, #16398, .F. ) ;
#16450 = CARTESIAN_POINT ( 'NONE',  ( 15.00000000000000178, -3.464101615137757051, -2.662500000000009415 ) ) ;
#16451 = CARTESIAN_POINT ( 'NONE',  ( 26.48145948632588187, -2.034413479899699340, -8.000000000000001776 ) ) ;
#16452 = CARTESIAN_POINT ( 'NONE',  ( 24.71185827157421855, 0.000000000000000000, 164.0636619062959483 ) ) ;
#16453 = CARTESIAN_POINT ( 'NONE',  ( 33.64979817785242489, 5.196152422706637353, 160.1667150552271437 ) ) ;
#16454 = CARTESIAN_POINT ( 'NONE',  ( 15.00000000000000000, 242.7999999999999829, 0.000000000000000000 ) ) ;
#16455 = CARTESIAN_POINT ( 'NONE',  ( 12.48663586349064403, 194.9999999999999716, 24.21355016816918493 ) ) ;
#16456 = EDGE_CURVE ( 'NONE', #11398, #19808, #3688, .T. ) ;
#16457 = CARTESIAN_POINT ( 'NONE',  ( 12.46528703574811558, 84.40231371789853654, -2.660918448318005503 ) ) ;
#16458 = CARTESIAN_POINT ( 'NONE',  ( 4.622313124798573369, 83.43518628210145494, 11.61527771782819940 ) ) ;
#16459 = ORIENTED_EDGE ( 'NONE', *, *, #15429, .F. ) ;
#16460 = VERTEX_POINT ( 'NONE', #12347 ) ;
#16461 = CARTESIAN_POINT ( 'NONE',  ( 27.00000000000000355, 198.9875000012290229, -3.306546357697854128E-15 ) ) ;
#16462 = CARTESIAN_POINT ( 'NONE',  ( 18.00000000000000000, 248.6312500012290343, -5.196152422706630247 ) ) ;
#16463 = CARTESIAN_POINT ( 'NONE',  ( 3.257655550456945548, 59.10231371789854649, 15.46528703574811736 ) ) ;
#16464 = CARTESIAN_POINT ( 'NONE',  ( 26.75643035624999655, -3.323476615752267715, -8.615624999385470772 ) ) ;
#16465 = CARTESIAN_POINT ( 'NONE',  ( 18.12178482187499640, 242.5843750006145285, -4.985214923628404904 ) ) ;
#16466 = CARTESIAN_POINT ( 'NONE',  ( -56.93080436395490551, 205.4999999999999716, -0.1155267958017894420 ) ) ;
#16467 = CARTESIAN_POINT ( 'NONE',  ( -1.045839947578415010E-13, 195.7250000012290343, 27.00000000000000355 ) ) ;
#16468 = CARTESIAN_POINT ( 'NONE',  ( -9.500000000000005329, 34.08981371789853654, 0.1745138560723101806 ) ) ;
#16469 = CARTESIAN_POINT ( 'NONE',  ( -66.82663769728823411, 204.3130714775002730, 3.149950860017883603 ) ) ;
#16470 = CARTESIAN_POINT ( 'NONE',  ( -8.710071997420207879, 97.91481371789856780, 3.796722387233182339 ) ) ;
#16471 = CARTESIAN_POINT ( 'NONE',  ( -27.24356964375000345, 199.4093750006145456, 0.000000000000000000 ) ) ;
#16472 = CARTESIAN_POINT ( 'NONE',  ( -8.715434833792127023, 14.53981371789855892, 8.962234695871568846 ) ) ;
#16473 = VECTOR ( 'NONE', #4534, 1000.000000000000000 ) ;
#16474 = CARTESIAN_POINT ( 'NONE',  ( -2.311890736173176641, 60.72268628210144925, -12.53471296425194836 ) ) ;
#16475 = CARTESIAN_POINT ( 'NONE',  ( 19.56230152254411792, -5.196152422706629359, -7.837499998771035870 ) ) ;
#16476 = DIRECTION ( 'NONE',  ( 1.000000000000000000, 4.130293990420971855E-17, -0.000000000000000000 ) ) ;
#16477 = CARTESIAN_POINT ( 'NONE',  ( 27.58480908411420529, 5.407089921784856479, 161.0831760960101349 ) ) ;
#16478 = CARTESIAN_POINT ( 'NONE',  ( 21.00000000000000000, -6.928203230275506996, -1.181249998770955267 ) ) ;
#16479 = CARTESIAN_POINT ( 'NONE',  ( 13.44051670066910731, 5.407089921784862696, -7.471874999385508254 ) ) ;
#16480 = PLANE ( 'NONE',  #3034 ) ;
#16481 = CARTESIAN_POINT ( 'NONE',  ( -7.234628195640313564, 199.5700961906613884, -27.00000000000000355 ) ) ;
#16482 = CARTESIAN_POINT ( 'NONE',  ( -6.594114490232312775, 96.66018628210144925, -6.840914352312096547 ) ) ;
#16483 = LINE ( 'NONE', #21987, #30395 ) ;
#16484 = CARTESIAN_POINT ( 'NONE',  ( -12.53471296425194836, 113.6226862821014407, 2.311890736173176641 ) ) ;
#16485 = LINE ( 'NONE', #9852, #29977 ) ;
#16486 = CARTESIAN_POINT ( 'NONE',  ( 26.99999999999999645, 240.4187500012290570, -3.464101615137755275 ) ) ;
#16487 = ORIENTED_EDGE ( 'NONE', *, *, #15429, .T. ) ;
#16488 = CARTESIAN_POINT ( 'NONE',  ( 37.29692136982500728, 3.604726614523238837, 164.6377359093410746 ) ) ;
#16489 = CARTESIAN_POINT ( 'NONE',  ( 26.75643035624999655, -3.323476615752267715, -6.253124999385469174 ) ) ;
#16490 = CARTESIAN_POINT ( 'NONE',  ( 27.24356964374999279, 198.7718750006145569, -15.72908226750539207 ) ) ;
#16491 = CARTESIAN_POINT ( 'NONE',  ( 37.64173127707041289, 7.646167579472024665E-16, 168.5789311836665831 ) ) ;
#16492 = CARTESIAN_POINT ( 'NONE',  ( 25.32137226386890205, 3.464101615137757051, 168.2357904697519189 ) ) ;
#16493 = DIRECTION ( 'NONE',  ( 2.057406622567553763E-16, -0.000000000000000000, -1.000000000000000000 ) ) ;
#16494 = CARTESIAN_POINT ( 'NONE',  ( 26.75643035624999655, 240.6718750006145910, -3.323476615752271712 ) ) ;
#16495 = CARTESIAN_POINT ( 'NONE',  ( 16.56230152254410370, -6.928203230275506996, -6.974999998770984533 ) ) ;
#16496 = CARTESIAN_POINT ( 'NONE',  ( 9.465287035748106703, 10.80231371789855466, -2.064181346179063237 ) ) ;
#16497 = CARTESIAN_POINT ( 'NONE',  ( 10.49813415415989581, 137.7726862821014606, 7.228626920339069173 ) ) ;
#16499 = EDGE_LOOP ( 'NONE', ( #8798, #25012, #28439, #29053 ) ) ;
#16498 = ORIENTED_EDGE ( 'NONE', *, *, #11242, .T. ) ;
#16500 = CARTESIAN_POINT ( 'NONE',  ( 26.75643035624999655, 244.5343750006144887, 3.323476615752267715 ) ) ;
#16501 = CARTESIAN_POINT ( 'NONE',  ( -12.50000000000000355, 6.489813717898557321, 0.1745138560722785670 ) ) ;
#16502 = CARTESIAN_POINT ( 'NONE',  ( 26.75643035624999655, 3.323476615752271712, -4.378124999385460292 ) ) ;
#16503 = CARTESIAN_POINT ( 'NONE',  ( -5.770363421894122880, 115.1648137178985678, 14.38691631536194393 ) ) ;
#16504 = CARTESIAN_POINT ( 'NONE',  ( 26.99999999999999645, 7.347880794884117764E-16, -2.868749998770958598 ) ) ;
#16505 = CARTESIAN_POINT ( 'NONE',  ( 26.75643035624999655, 3.323476615752271712, -1.340624999385481075 ) ) ;
#16506 = EDGE_CURVE ( 'NONE', #5916, #20921, #9882, .T. ) ;
#16507 = CARTESIAN_POINT ( 'NONE',  ( 16.56230152254411436, 7.209453229046482114, -9.309374999385525484 ) ) ;
#16508 = ORIENTED_EDGE ( 'NONE', *, *, #16559, .T. ) ;
#16509 = CARTESIAN_POINT ( 'NONE',  ( 5.727106289114498080E-15, 198.4250000012290229, 31.17691453623979214 ) ) ;
#16510 = CARTESIAN_POINT ( 'NONE',  ( 12.53471296425194836, 109.0226862821014606, -2.311890736173178418 ) ) ;
#16511 = CARTESIAN_POINT ( 'NONE',  ( 22.80587116629411071, 3.604726614523238837, -0.7781249993855585689 ) ) ;
#16512 = CARTESIAN_POINT ( 'NONE',  ( -41.88169563604517265, 210.1155267958018271, 8.500000000000003553 ) ) ;
#16513 = CARTESIAN_POINT ( 'NONE',  ( 15.24356964375000167, 244.8343750006145285, 3.323476615752272600 ) ) ;
#16514 = CARTESIAN_POINT ( 'NONE',  ( 10.56230152254411081, 0.000000000000000000, -3.037499998771009402 ) ) ;
#16515 = CARTESIAN_POINT ( 'NONE',  ( -66.22544563604516554, 214.8429017333602360, 4.673758765035156415 ) ) ;
#16516 = CARTESIAN_POINT ( 'NONE',  ( 12.50000000000000355, 127.7101862821014606, 0.1745138560725507937 ) ) ;
#16517 = CARTESIAN_POINT ( 'NONE',  ( 10.31873187879410558, -3.604726614523244610, -10.05937499938549884 ) ) ;
#16518 = CARTESIAN_POINT ( 'NONE',  ( -39.90997103062156270, 215.5714017266979852, 3.350049139982118618 ) ) ;
#16519 = DIRECTION ( 'NONE',  ( 0.000000000000000000, 0.000000000000000000, -1.000000000000000000 ) ) ;
#16520 = LINE ( 'NONE', #7614, #16597 ) ;
#16521 = CARTESIAN_POINT ( 'NONE',  ( 0.1745138560725837118, 125.4101862821014635, -15.50000000000000533 ) ) ;
#16522 = CARTESIAN_POINT ( 'NONE',  ( 26.99999999999999645, 242.5937500012290400, 3.464101615137751278 ) ) ;
#16523 = CARTESIAN_POINT ( 'NONE',  ( -12.46528703574805697, 12.99768628210143362, -2.660918448318280838 ) ) ;
#16524 = AXIS2_PLACEMENT_3D ( 'NONE', #13656, #25209, #7966 ) ;
#16525 = CARTESIAN_POINT ( 'NONE',  ( 16.56230152254411436, 6.928203230275514990, -9.562500000000060396 ) ) ;
#16526 = EDGE_LOOP ( 'NONE', ( #9159, #18884, #16148, #8689 ) ) ;
#16527 = FACE_OUTER_BOUND ( 'NONE', #7120, .T. ) ;
#16528 = CARTESIAN_POINT ( 'NONE',  ( -1.715153634034234598, 88.32268628210142936, -9.534712964251941258 ) ) ;
#16529 =( NAMED_UNIT ( * ) PLANE_ANGLE_UNIT ( ) SI_UNIT ( $, .RADIAN. ) );
#16530 = CARTESIAN_POINT ( 'NONE',  ( -8.152565276336593669, 126.9523137178985621, -5.233372021372610483 ) ) ;
#16531 = CARTESIAN_POINT ( 'NONE',  ( 27.24356964375000345, 195.0781250006145342, -3.336375036156643733E-15 ) ) ;
#16532 = CARTESIAN_POINT ( 'NONE',  ( 15.02283181144952628, 7.347880794884122694E-16, 50.52293445648592751 ) ) ;
#16533 = CARTESIAN_POINT ( 'NONE',  ( 5.778771075727756162E-15, 197.7218750006145456, 31.45816453501075927 ) ) ;
#16534 = CARTESIAN_POINT ( 'NONE',  ( 22.56230152254410370, 0.000000000000000000, -10.00000000000000000 ) ) ;
#16535 = CARTESIAN_POINT ( 'NONE',  ( 22.60769515458672885, 244.0174038105676289, -5.999999999999998224 ) ) ;
#16536 = AXIS2_PLACEMENT_3D ( 'NONE', #34366, #33817, #16758 ) ;
#16537 = CARTESIAN_POINT ( 'NONE',  ( -8.152565276336593669, 53.35231371789856780, -5.233372021372610483 ) ) ;
#16538 = FACE_OUTER_BOUND ( 'NONE', #4879, .T. ) ;
#16539 = ORIENTED_EDGE ( 'NONE', *, *, #23362, .F. ) ;
#16540 =( GEOMETRIC_REPRESENTATION_CONTEXT ( 3 ) GLOBAL_UNCERTAINTY_ASSIGNED_CONTEXT ( ( #22239 ) ) GLOBAL_UNIT_ASSIGNED_CONTEXT ( ( #8806, #8991, #34397 ) ) REPRESENTATION_CONTEXT ( 'NONE', 'WORKASPACE' ) );
#16541 = CARTESIAN_POINT ( 'NONE',  ( 24.00000000000000000, 241.2062500012290513, 5.196152422706629359 ) ) ;
#16542 = CARTESIAN_POINT ( 'NONE',  ( -10.49813415416004858, 70.02731371789855075, 7.228626920338840023 ) ) ;
#16543 = CARTESIAN_POINT ( 'NONE',  ( 22.80587116629411781, 3.604726614523243278, -6.684374999385514826 ) ) ;
#16544 = CARTESIAN_POINT ( 'NONE',  ( 27.24356964375000700, 197.2906250006145399, 15.72908226750537075 ) ) ;
#16545 = CARTESIAN_POINT ( 'NONE',  ( 15.24356964374999990, 0.000000000000000000, -7.903124999385474858 ) ) ;
#16546 = CARTESIAN_POINT ( 'NONE',  ( -7.228626920338836470, 35.52731371789855075, -10.49813415416005213 ) ) ;
#16547 = AXIS2_PLACEMENT_3D ( 'NONE', #22533, #8677, #2424 ) ;
#16548 = VERTEX_POINT ( 'NONE', #6854 ) ;
#16549 = UNCERTAINTY_MEASURE_WITH_UNIT (LENGTH_MEASURE( 1.000000000000000082E-05 ), #24444, 'distance_accuracy_value', 'NONE');
#16550 = CARTESIAN_POINT ( 'NONE',  ( 16.56230152254411792, -7.209453229046482114, -1.884374999385517446 ) ) ;
#16551 = CARTESIAN_POINT ( 'NONE',  ( -27.00000000000000355, 199.9625000000000057, -15.58845726811989429 ) ) ;
#16552 = CARTESIAN_POINT ( 'NONE',  ( 31.35328515338631306, 7.209453229046482114, 168.3385908086170559 ) ) ;
#16553 = CARTESIAN_POINT ( 'NONE',  ( -46.23586230271182984, 206.8500491399821328, 5.686928522499748340 ) ) ;
#16554 = CARTESIAN_POINT ( 'NONE',  ( 28.40800656884236730, -5.196152422706632912, 169.0950422780865097 ) ) ;
#16555 = CARTESIAN_POINT ( 'NONE',  ( -13.49999999999998401, 196.4750000000000227, 23.38268590217985476 ) ) ;
#16556 = CARTESIAN_POINT ( 'NONE',  ( 4.944772684328420986, 58.81481371789855217, 11.48171059495408208 ) ) ;
#16557 = CARTESIAN_POINT ( 'NONE',  ( -39.31622103062156981, 211.0902445701382533, 4.530955311639240257 ) ) ;
#16559 = EDGE_CURVE ( 'NONE', #6008, #2166, #32812, .T. ) ;
#16558 = CARTESIAN_POINT ( 'NONE',  ( -51.19122103062155560, 208.3738570449993404, -6.530955311639226935 ) ) ;
#16560 = CARTESIAN_POINT ( 'NONE',  ( 27.00000000000000355, 195.8375000012290457, -3.306546357697854128E-15 ) ) ;
#16561 = DIRECTION ( 'NONE',  ( 0.000000000000000000, 0.000000000000000000, 1.000000000000000000 ) ) ;
#16562 = CARTESIAN_POINT ( 'NONE',  ( 14.38691631536194393, 48.46481371789856496, 5.770363421894124656 ) ) ;
#16563 = CARTESIAN_POINT ( 'NONE',  ( -68.60788769728823411, 218.4690446883607535, 2.393094931466250408 ) ) ;
#16564 = STYLED_ITEM ( 'NONE', ( #12729 ), #3821 ) ;
#16565 = CARTESIAN_POINT ( 'NONE',  ( 10.69584247140445221, 25.64768628210143930, -6.932735513423970097 ) ) ;
#16566 = CARTESIAN_POINT ( 'NONE',  ( -11.48171059495397373, 68.48518628210145209, -4.944772684328680334 ) ) ;
#16567 = CARTESIAN_POINT ( 'NONE',  ( -8.632099005475501130, 4.947686282101431132, -13.23911966647218996 ) ) ;
#16568 = CARTESIAN_POINT ( 'NONE',  ( 19.56230152254412502, -5.196152422706635576, -2.550000000000052225 ) ) ;
#16569 = LINE ( 'NONE', #1400, #22230 ) ;
#16570 = ORIENTED_EDGE ( 'NONE', *, *, #24057, .F. ) ;
#16571 = CARTESIAN_POINT ( 'NONE',  ( -8.632099005475501130, 32.54768628210143788, -13.23911966647218996 ) ) ;
#16572 = CARTESIAN_POINT ( 'NONE',  ( 5.778771075727756162E-15, 194.9656250006145797, 31.45816453501076637 ) ) ;
#16573 = CARTESIAN_POINT ( 'NONE',  ( 27.24356964375000700, 198.2468750006145513, 15.72908226750537075 ) ) ;
#16574 = CARTESIAN_POINT ( 'NONE',  ( 22.60769515458674306, 247.4325961894323598, 5.999999999999992895 ) ) ;
#16575 = CARTESIAN_POINT ( 'NONE',  ( 13.50000000000001421, 195.3125000012290400, 23.38268590217984055 ) ) ;
#16576 = CARTESIAN_POINT ( 'NONE',  ( 20.99999999999999289, 242.6875000000000000, -5.999999999999997335 ) ) ;
#16577 = CARTESIAN_POINT ( 'NONE',  ( 0.1745138560725515708, 5.810186282101447830, -12.50000000000000355 ) ) ;
#16578 = CIRCLE ( 'NONE', #3849, 3.999999999999996447 ) ;
#16579 = CARTESIAN_POINT ( 'NONE',  ( 23.87821517812499650, 247.0093750006145399, -4.985214923628404904 ) ) ;
#16580 = CARTESIAN_POINT ( 'NONE',  ( 7.954856959092311719, 111.4273137178985422, -5.529263428287300108 ) ) ;
#16581 = CARTESIAN_POINT ( 'NONE',  ( 18.12178482187500350, 241.3843750006145115, 4.985214923628407568 ) ) ;
#16582 = EDGE_LOOP ( 'NONE', ( #15087, #33694, #10944, #19984 ) ) ;
#16583 = CARTESIAN_POINT ( 'NONE',  ( -64.45163769728823411, 215.6869285224996986, -3.149950860017881382 ) ) ;
#16584 = EDGE_CURVE ( 'NONE', #20044, #17872, #11699, .T. ) ;
#16585 = CARTESIAN_POINT ( 'NONE',  ( 15.00000000000000178, 248.7437500012290457, 3.464101615137757051 ) ) ;
#16586 = CARTESIAN_POINT ( 'NONE',  ( -4.944772684328424539, 118.6148137178985564, -11.48171059495408031 ) ) ;
#16587 = CARTESIAN_POINT ( 'NONE',  ( 10.31873187879411091, -3.604726614523240613, -8.653124999385532590 ) ) ;
#16588 = CARTESIAN_POINT ( 'NONE',  ( 33.91574363238778034, 5.407089921784857367, 161.8091613863793725 ) ) ;
#16589 =( BOUNDED_CURVE ( )  B_SPLINE_CURVE ( 2, ( #12169, #24497, #18252, #12364, #7070, #21290, #26951, #23934, #18638 ),
 .UNSPECIFIED., .F., .F. ) 
 B_SPLINE_CURVE_WITH_KNOTS ( ( 3, 2, 2, 2, 3 ),
 ( 0.3541666666666666852, 0.3611111111111111049, 0.3750000000000000000, 0.3888888888888888951, 0.3958333333333333703 ),
 .UNSPECIFIED. ) 
 CURVE ( )  GEOMETRIC_REPRESENTATION_ITEM ( )  RATIONAL_B_SPLINE_CURVE ( ( 0.9330127018922194093, 0.9330127018922196314, 1.000000000000000000, 0.8660254037844387076, 1.000000000000000000, 0.8660254037844387076, 1.000000000000000000, 0.9330127018922190762, 0.9330127018922194093 ) ) 
 REPRESENTATION_ITEM ( '' )  );
#16590 = CARTESIAN_POINT ( 'NONE',  ( 22.60769515458670753, 240.9236538117966973, -6.000000000000011546 ) ) ;
#16591 = CARTESIAN_POINT ( 'NONE',  ( -27.24356964374999990, 199.8218750006145399, -15.72908226750537786 ) ) ;
#16592 = ORIENTED_EDGE ( 'NONE', *, *, #7515, .T. ) ;
#16593 = EDGE_LOOP ( 'NONE', ( #29093, #19307, #10446, #7170 ) ) ;
#16594 = ORIENTED_EDGE ( 'NONE', *, *, #88, .F. ) ;
#16595 = CARTESIAN_POINT ( 'NONE',  ( 26.99999999999999645, -3.464101615137751278, -5.156249998770954690 ) ) ;
#16597 = VECTOR ( 'NONE', #2286, 1000.000000000000000 ) ;
#16596 = CARTESIAN_POINT ( 'NONE',  ( 23.87821517812500005, -4.985214923628404016, -2.690624999385465621 ) ) ;
#16598 = DIRECTION ( 'NONE',  ( -0.000000000000000000, -0.000000000000000000, 1.000000000000000000 ) ) ;
#16599 = CARTESIAN_POINT ( 'NONE',  ( 26.99999999999983658, 3.464101615137847645, -6.037499999999991651 ) ) ;
#16600 = LINE ( 'NONE', #20000, #22663 ) ;
#16601 = CARTESIAN_POINT ( 'NONE',  ( -0.1745138560725500443, 56.41018628210145636, 12.50000000000000355 ) ) ;
#16602 = CARTESIAN_POINT ( 'NONE',  ( -63.45461230271182274, 208.1428034533958851, -6.469044688360754414 ) ) ;
#16603 = CARTESIAN_POINT ( 'NONE',  ( 14.99999999999954170, 215.9999999999999716, -0.1308996912579681871 ) ) ;
#16604 = CARTESIAN_POINT ( 'NONE',  ( -46.43377896937850835, 208.9097554298617183, 4.530955311639234040 ) ) ;
#16605 = CARTESIAN_POINT ( 'NONE',  ( 27.00000000000001421, 197.0374999999999943, 15.58845726811988897 ) ) ;
#16606 = CARTESIAN_POINT ( 'NONE',  ( 25.10239346032254915, -3.464101615137757051, 165.7328512920207402 ) ) ;
#16607 = CARTESIAN_POINT ( 'NONE',  ( 12.50000000000000355, 121.4898137178985564, -0.1745138560722771515 ) ) ;
#16608 = CARTESIAN_POINT ( 'NONE',  ( -37.13913769728823411, 206.8500491399821044, -5.686928522499717253 ) ) ;
#16609 = CARTESIAN_POINT ( 'NONE',  ( -55.74330436395489841, 210.1155267958016850, -8.500000000000003553 ) ) ;
#16610 =( BOUNDED_CURVE ( )  B_SPLINE_CURVE ( 2, ( #36457, #22076, #30787, #16390, #13536, #25091, #16575, #17501, #14649 ),
 .UNSPECIFIED., .F., .F. ) 
 B_SPLINE_CURVE_WITH_KNOTS ( ( 3, 2, 2, 2, 3 ),
 ( 0.7708333333333333703, 0.7777777777777777901, 0.7916666666666666297, 0.8055555555555555802, 0.8125000000000000000 ),
 .UNSPECIFIED. ) 
 CURVE ( )  GEOMETRIC_REPRESENTATION_ITEM ( )  RATIONAL_B_SPLINE_CURVE ( ( 0.9330127018922192983, 0.9330127018922198534, 1.000000000000000000, 0.8660254037844387076, 1.000000000000000000, 0.8660254037844387076, 1.000000000000000000, 0.9330127018922194093, 0.9330127018922194093 ) ) 
 REPRESENTATION_ITEM ( '' )  );
#16611 = CARTESIAN_POINT ( 'NONE',  ( 20.99999999999999645, 6.646953231504538984, -0.8156249993854914893 ) ) ;
#16612 = CARTESIAN_POINT ( 'NONE',  ( 27.24356964375000700, 195.9406250006145456, 15.72908226750537075 ) ) ;
#16613 = CARTESIAN_POINT ( 'NONE',  ( -8.632099005475794229, 87.85231371789855359, 13.23911966647199812 ) ) ;
#16614 = CARTESIAN_POINT ( 'NONE',  ( -65.82961230271185116, 212.3930949314663792, 8.469044688360751749 ) ) ;
#16615 = ORIENTED_EDGE ( 'NONE', *, *, #25166, .T. ) ;
#16616 = CARTESIAN_POINT ( 'NONE',  ( 24.00000000000000000, 242.1062500012290286, 5.196152422706629359 ) ) ;
#16617 = CARTESIAN_POINT ( 'NONE',  ( 12.50000000000000355, 118.5101862821014578, 0.1745138560725507937 ) ) ;
#16618 = CARTESIAN_POINT ( 'NONE',  ( 5.770363421893814682, 65.03518628210144925, 14.38691631536207183 ) ) ;
#16619 = CARTESIAN_POINT ( 'NONE',  ( 13.56230152254411792, -5.196152422706638241, -0.8250000000000479172 ) ) ;
#16620 = CARTESIAN_POINT ( 'NONE',  ( 24.90469035240339934, 3.604726614523240613, 166.2677426758239108 ) ) ;
#16621 = AXIS2_PLACEMENT_3D ( 'NONE', #32686, #6730, #36272 ) ;
#16622 = CARTESIAN_POINT ( 'NONE',  ( -10.83675517735155047, 87.46018628210146062, -11.08355503943142750 ) ) ;
#16623 = AXIS2_PLACEMENT_3D ( 'NONE', #29310, #25916, #20804 ) ;
#16624 = CARTESIAN_POINT ( 'NONE',  ( -41.69122103062156270, 208.3738570449994256, -6.530955311639227823 ) ) ;
#16625 = AXIS2_PLACEMENT_3D ( 'NONE', #6401, #34827, #6588 ) ;
#16626 = CARTESIAN_POINT ( 'NONE',  ( 10.31873187879410736, 0.000000000000000000, -6.890624999385530636 ) ) ;
#16627 = CARTESIAN_POINT ( 'NONE',  ( -8.843639120294326972, 30.53518628210144570, 3.474262827703335166 ) ) ;
#16628 = CARTESIAN_POINT ( 'NONE',  ( 15.00000000000000178, 0.000000000000000000, -3.599999999999992095 ) ) ;
#16629 = CARTESIAN_POINT ( 'NONE',  ( -56.93080436395490551, 203.5000000000000000, -0.1155267958017335561 ) ) ;
#16630 = DIRECTION ( 'NONE',  ( 0.000000000000000000, 0.000000000000000000, -1.000000000000000000 ) ) ;
#16631 = CARTESIAN_POINT ( 'NONE',  ( 8.962234695871762469, 62.16018628210144215, -8.715434833791931624 ) ) ;
#16632 = CARTESIAN_POINT ( 'NONE',  ( -1.909035429704832693E-15, 198.5374999999999943, -31.17691453623979214 ) ) ;
#16633 = CARTESIAN_POINT ( 'NONE',  ( 15.00000000000000000, 0.000000000000000000, -2.193749998770949894 ) ) ;
#16635 = CARTESIAN_POINT ( 'NONE',  ( 13.44051670066911264, 5.407089921784862696, -0.2718749993855240632 ) ) ;
#16634 = CARTESIAN_POINT ( 'NONE',  ( -3.796722387233375073, 29.38518628210144712, 8.710071997420127943 ) ) ;
#16636 = CARTESIAN_POINT ( 'NONE',  ( 15.24356964374999990, 249.3718750006145228, -3.323476615752268604 ) ) ;
#16637 = ORIENTED_EDGE ( 'NONE', *, *, #29749, .T. ) ;
#16638 = CARTESIAN_POINT ( 'NONE',  ( 21.00000000000000000, 6.928203230275506996, -3.262499999999993516 ) ) ;
#16639 = CARTESIAN_POINT ( 'NONE',  ( 21.68347279894478774, -5.929004884096451988, -8.000000000000005329 ) ) ;
#16640 = CARTESIAN_POINT ( 'NONE',  ( 30.72576380560321851, 7.209453229046482114, 161.1659889823564811 ) ) ;
#16641 = CARTESIAN_POINT ( 'NONE',  ( 16.56230152254411436, 7.209453229046475009, -1.603124999385524108 ) ) ;
#16642 = CARTESIAN_POINT ( 'NONE',  ( 28.29077060037018043, 5.407089921784856479, 169.1523531505532674 ) ) ;
#16643 = CARTESIAN_POINT ( 'NONE',  ( 15.00000000000000178, 242.3875000000000171, 3.464101615137757051 ) ) ;
#16644 = CARTESIAN_POINT ( 'NONE',  ( 13.06157021329630474, 195.0015827616130650, 23.91706345632494646 ) ) ;
#16645 = CARTESIAN_POINT ( 'NONE',  ( 11.61527771782819940, 81.13518628210145778, -4.622313124798573369 ) ) ;
#16646 = ORIENTED_EDGE ( 'NONE', *, *, #8322, .F. ) ;
#16647 = ORIENTED_EDGE ( 'NONE', *, *, #37122, .T. ) ;
#16648 = CARTESIAN_POINT ( 'NONE',  ( 26.99999999999999645, 196.7750000012290741, -15.58845726811990495 ) ) ;
#16649 = CARTESIAN_POINT ( 'NONE',  ( 28.24132121073036927, -5.196152422706638241, 167.1898199167616781 ) ) ;
#16650 = CARTESIAN_POINT ( 'NONE',  ( 8.927990412390371944, 49.32731371789854791, 13.04141134922778811 ) ) ;
#16651 = CARTESIAN_POINT ( 'NONE',  ( 26.75643035624999655, 3.323476615752271712, -8.990624999385502747 ) ) ;
#16652 = CARTESIAN_POINT ( 'NONE',  ( 23.87821517812499650, 243.8593750006145342, -4.985214923628404904 ) ) ;
#16653 = CARTESIAN_POINT ( 'NONE',  ( -60.88913769728824121, 207.8500491399821613, -3.954877714930864485 ) ) ;
#16654 = CARTESIAN_POINT ( 'NONE',  ( 15.00000000000058620, 3.464101615138089674, -7.237500000000000711 ) ) ;
#16655 = CARTESIAN_POINT ( 'NONE',  ( -7.954856959092309943, 33.22731371789855359, 5.529263428287300108 ) ) ;
#16656 = CARTESIAN_POINT ( 'NONE',  ( 31.09590335053109555, 6.928203230275514990, 165.3967033402026914 ) ) ;
#16657 = CARTESIAN_POINT ( 'NONE',  ( 1.715153634034445762, 101.0773137178985479, -9.534712964251895073 ) ) ;
#16658 = CARTESIAN_POINT ( 'NONE',  ( 27.24356964375000700, 198.6968750006145115, 15.72908226750537075 ) ) ;
#16659 = CARTESIAN_POINT ( 'NONE',  ( 11.48171059495408208, 10.51481371789855856, -4.944772684328420986 ) ) ;
#16660 = ADVANCED_FACE ( 'NONE', ( #18624 ), #29972, .T. ) ;
#16661 = CARTESIAN_POINT ( 'NONE',  ( 12.50000000000000355, 72.51018628210145778, 0.1745138560725507937 ) ) ;
#16662 = CARTESIAN_POINT ( 'NONE',  ( 22.56230152254409660, 3.464101615137755275, -7.724999998770988086 ) ) ;
#16663 = ADVANCED_FACE ( 'NONE', ( #27319, #29781 ), #27510, .F. ) ;
#16664 = CARTESIAN_POINT ( 'NONE',  ( 33.90267027097563357, -5.407089921784855591, 161.6597321816656176 ) ) ;
#16665 = CYLINDRICAL_SURFACE ( 'NONE', #6684, 5.999999999999999112 ) ;
#16666 = CARTESIAN_POINT ( 'NONE',  ( 22.80587116629411426, 7.646167579472024665E-16, -7.621874999385519267 ) ) ;
#16667 = DIRECTION ( 'NONE',  ( 0.8083506638593009885, 0.5887012860850803220, -0.000000000000000000 ) ) ;
#16668 = CARTESIAN_POINT ( 'NONE',  ( 20.99999999999999645, 242.4625000000000057, 5.999999999999998224 ) ) ;
#16669 = CARTESIAN_POINT ( 'NONE',  ( -3.474262827703337830, 69.63518628210144357, -8.843639120294326972 ) ) ;
#16670 = CARTESIAN_POINT ( 'NONE',  ( -80.98946968704737515, 222.6276076386831733, 5.000000000000000000 ) ) ;
#16671 = EDGE_CURVE ( 'NONE', #31762, #31857, #12919, .T. ) ;
#16672 = CARTESIAN_POINT ( 'NONE',  ( 11.61527771782819940, 117.9351862821014549, -4.622313124798573369 ) ) ;
#16673 = CARTESIAN_POINT ( 'NONE',  ( 0.000000000000000000, 148.0000000000000000, 4.899999999999999467 ) ) ;
#16674 = CARTESIAN_POINT ( 'NONE',  ( 3.306546357697853733E-15, 210.0000000000000284, 27.00000000000000000 ) ) ;
#16675 = EDGE_LOOP ( 'NONE', ( #2723, #33505, #9938, #22280, #1331 ) ) ;
#16676 = CARTESIAN_POINT ( 'NONE',  ( 34.17721086063072988, -5.407089921784855591, 164.7977454806546120 ) ) ;
#16677 = CARTESIAN_POINT ( 'NONE',  ( 15.24356964375000167, -3.323476615752272600, -4.153124999385478411 ) ) ;
#16678 = CARTESIAN_POINT ( 'NONE',  ( -1.926257025242585782E-15, 197.0468750006145342, -31.45816453501076637 ) ) ;
#16679 = CARTESIAN_POINT ( 'NONE',  ( 34.36840877128340566, -5.407089921784861808, 166.9831475995933943 ) ) ;
#16680 = CARTESIAN_POINT ( 'NONE',  ( 37.18419511108482567, 3.464101615137759271, 166.1439171237837229 ) ) ;
#16681 = CARTESIAN_POINT ( 'NONE',  ( -1.045839947578415010E-13, 196.1750000012290229, 27.00000000000000355 ) ) ;
#16682 = CARTESIAN_POINT ( 'NONE',  ( 26.75643035624999655, 240.5968750006145456, 3.323476615752267715 ) ) ;
#16683 = DIRECTION ( 'NONE',  ( -1.000000000000000000, -6.123233995736766036E-17, -0.000000000000000000 ) ) ;
#16684 = VECTOR ( 'NONE', #24774, 1000.000000000000000 ) ;
#16685 = CARTESIAN_POINT ( 'NONE',  ( 7.228626920338837358, 132.1273137178986019, 10.49813415416005036 ) ) ;
#16686 = CARTESIAN_POINT ( 'NONE',  ( 4.944772684328679446, 135.1851862821014549, -11.48171059495397373 ) ) ;
#16688 = VERTEX_POINT ( 'NONE', #27131 ) ;
#16687 = ORIENTED_EDGE ( 'NONE', *, *, #19704, .F. ) ;
#16689 = CARTESIAN_POINT ( 'NONE',  ( 18.12178482187499640, 245.6218750006145228, -4.985214923628404904 ) ) ;
#16690 = CARTESIAN_POINT ( 'NONE',  ( -4.944772684328424539, 8.214813717898532985, -11.48171059495408031 ) ) ;
#16691 = CARTESIAN_POINT ( 'NONE',  ( 26.75643035624999655, 7.049594010296217766E-16, -3.965624999385464200 ) ) ;
#16692 = CARTESIAN_POINT ( 'NONE',  ( 15.53471296425188797, 112.5773137178985479, 2.908627838312457747 ) ) ;
#16693 = CARTESIAN_POINT ( 'NONE',  ( 22.56230152254411792, 7.347880794884125653E-16, -2.475000000000060485 ) ) ;
#16694 = CARTESIAN_POINT ( 'NONE',  ( 15.24356964374999990, 0.000000000000000000, -1.153124999385496396 ) ) ;
#16695 = CARTESIAN_POINT ( 'NONE',  ( 16.56230152254411436, 7.209453229046482114, -7.959374999385475213 ) ) ;
#16696 = CARTESIAN_POINT ( 'NONE',  ( 27.00000000000000355, 199.4375000012290400, -3.306546357697854128E-15 ) ) ;
#16697 = CARTESIAN_POINT ( 'NONE',  ( -8.962234695871760692, 112.7601862821014720, 8.715434833791933400 ) ) ;
#16698 = CARTESIAN_POINT ( 'NONE',  ( 19.68408634441910721, -5.407089921784855591, -2.690624999385549110 ) ) ;
#16699 = CARTESIAN_POINT ( 'NONE',  ( -41.68377896937850124, 207.8379586601372750, 8.530955311639258909 ) ) ;
#16700 = CARTESIAN_POINT ( 'NONE',  ( 23.87821517812499650, 245.0968750006145171, -4.985214923628404904 ) ) ;
#16701 = AXIS2_PLACEMENT_3D ( 'NONE', #3787, #12325, #32602 ) ;
#16702 = CARTESIAN_POINT ( 'NONE',  ( 13.56230152254410726, 5.196152422706630247, -2.662499998771022724 ) ) ;
#16703 = CARTESIAN_POINT ( 'NONE',  ( -66.81919563604517975, 216.5000000000000000, -0.1155267958017906493 ) ) ;
#16704 = CARTESIAN_POINT ( 'NONE',  ( 8.962234695871762469, 126.5601862821014691, -8.715434833791931624 ) ) ;
#16705 = CARTESIAN_POINT ( 'NONE',  ( 22.56230152254411081, 3.464101615137755275, -1.874999998771011311 ) ) ;
#16706 = AXIS2_PLACEMENT_3D ( 'NONE', #29675, #9406, #35169 ) ;
#16707 = CARTESIAN_POINT ( 'NONE',  ( -46.63913769728824121, 206.8500491399821044, -5.686928522499717253 ) ) ;
#16708 = DIRECTION ( 'NONE',  ( 0.000000000000000000, 0.000000000000000000, -1.000000000000000000 ) ) ;
#16709 = DIRECTION ( 'NONE',  ( 0.08715574274765142126, 0.000000000000000000, 0.9961946980917461003 ) ) ;
#16710 = CARTESIAN_POINT ( 'NONE',  ( -14.25334919248782306, 123.6851862821014549, -6.092822981423979378 ) ) ;
#16711 = DIRECTION ( 'NONE',  ( 0.000000000000000000, 1.000000000000000000, -2.168404344971006896E-16 ) ) ;
#16712 = CARTESIAN_POINT ( 'NONE',  ( -8.710071997420127943, 132.8851862821014436, -3.796722387233380402 ) ) ;
#16713 = CARTESIAN_POINT ( 'NONE',  ( 10.56230152254411436, -3.464101615137761048, -8.962500000000044764 ) ) ;
#16714 = CARTESIAN_POINT ( 'NONE',  ( 26.99999999999999645, 245.8187500012290627, -3.464101615137755275 ) ) ;
#16715 = ORIENTED_EDGE ( 'NONE', *, *, #27441, .F. ) ;
#16716 = FACE_OUTER_BOUND ( 'NONE', #28957, .T. ) ;
#16717 = CARTESIAN_POINT ( 'NONE',  ( -0.1745138560725182642, 74.81018628210145494, 9.500000000000005329 ) ) ;
#16718 = LINE ( 'NONE', #13872, #35718 ) ;
#16719 = CARTESIAN_POINT ( 'NONE',  ( -27.24356964374999990, 196.1656250006145399, -15.72908226750537786 ) ) ;
#16720 = CARTESIAN_POINT ( 'NONE',  ( 19.39230484541326049, 242.3138461906613657, -5.999999999999997335 ) ) ;
#16721 = CARTESIAN_POINT ( 'NONE',  ( -1.926257025242585782E-15, 197.0468750006145626, -31.45816453501075927 ) ) ;
#16722 = CARTESIAN_POINT ( 'NONE',  ( 15.00000000000000355, 7.347880794884112834E-16, -8.000000000000000000 ) ) ;
#16723 = DIRECTION ( 'NONE',  ( 1.000000000000000000, 0.000000000000000000, 0.000000000000000000 ) ) ;
#16724 = CARTESIAN_POINT ( 'NONE',  ( 5.233372021372610483, 64.85231371789855359, -8.152565276336593669 ) ) ;
#16725 = CARTESIAN_POINT ( 'NONE',  ( 26.99999999999999645, 3.464101615137755275, -8.737500000000000711 ) ) ;
#16726 = ORIENTED_EDGE ( 'NONE', *, *, #33451, .T. ) ;
#16727 = CARTESIAN_POINT ( 'NONE',  ( 15.00000000000000000, 241.9187500012290570, -3.464101615137752166 ) ) ;
#16728 = CARTESIAN_POINT ( 'NONE',  ( -7.228626920338836470, 53.92731371789854933, -10.49813415416005213 ) ) ;
#16729 = CARTESIAN_POINT ( 'NONE',  ( 10.31873187879410558, 0.000000000000000000, -6.946874999385510563 ) ) ;
#16730 = CARTESIAN_POINT ( 'NONE',  ( 23.87821517812499650, 4.985214923628404904, -7.153124999385473970 ) ) ;
#16731 = CARTESIAN_POINT ( 'NONE',  ( -10.69584247140429412, 25.75231371789854506, -6.932735513424201024 ) ) ;
#16732 = EDGE_LOOP ( 'NONE', ( #30715, #3795, #9517 ) ) ;
#16733 = CARTESIAN_POINT ( 'NONE',  ( 16.56230152254412147, -7.209453229046482114, -0.9843749993855260838 ) ) ;
#16734 = CARTESIAN_POINT ( 'NONE',  ( -4.944772684328673229, 10.98518628210143433, 11.48171059495397728 ) ) ;
#16735 = CARTESIAN_POINT ( 'NONE',  ( 25.10079077358561150, 3.604726614523240613, 168.5091807465304043 ) ) ;
#16736 = CARTESIAN_POINT ( 'NONE',  ( -39.70461230271183695, 208.1428034533959135, -6.469044688360754414 ) ) ;
#16737 = DIRECTION ( 'NONE',  ( -0.000000000000000000, 1.000000000000000000, -0.000000000000000000 ) ) ;
#16738 = AXIS2_PLACEMENT_3D ( 'NONE', #1392, #13717, #12966 ) ;
#16739 = DIRECTION ( 'NONE',  ( 0.000000000000000000, 0.000000000000000000, 1.000000000000000000 ) ) ;
#16740 = CARTESIAN_POINT ( 'NONE',  ( -34.56622103062156981, 211.0902445701382533, 4.530955311639240257 ) ) ;
#16741 = CARTESIAN_POINT ( 'NONE',  ( -49.40997103062156981, 215.5714017266979852, 3.350049139982118618 ) ) ;
#16742 = ORIENTED_EDGE ( 'NONE', *, *, #35419, .T. ) ;
#16743 = DIRECTION ( 'NONE',  ( 1.000000000000000000, 0.000000000000000000, 0.000000000000000000 ) ) ;
#16744 = CARTESIAN_POINT ( 'NONE',  ( -7.794140580174272692, 220.1661346705901678, -2.888490404254253185 ) ) ;
#16745 = CARTESIAN_POINT ( 'NONE',  ( 3.257655550456945548, 40.70231371789854791, 15.46528703574811736 ) ) ;
#16746 = CARTESIAN_POINT ( 'NONE',  ( -31.59002896937850124, 202.6965474657332038, 4.350049139982197666 ) ) ;
#16747 = CARTESIAN_POINT ( 'NONE',  ( -9.534712964251941258, 141.2226862821014493, 1.715153634034234154 ) ) ;
#16748 = CARTESIAN_POINT ( 'NONE',  ( 11.61527771782819940, 62.73518628210145209, -4.622313124798573369 ) ) ;
#16749 = CARTESIAN_POINT ( 'NONE',  ( -5.770363421893818234, 14.43518628210144072, -14.38691631536207005 ) ) ;
#16750 = CARTESIAN_POINT ( 'NONE',  ( 13.56230152254411614, -5.196152422706638241, -1.725000000000059819 ) ) ;
#16751 = CARTESIAN_POINT ( 'NONE',  ( 19.95811783012822005, 240.0005236131589754, -5.908847734042844912 ) ) ;
#16752 = ORIENTED_EDGE ( 'NONE', *, *, #7640, .F. ) ;
#16753 = CARTESIAN_POINT ( 'NONE',  ( -14.38691631536207183, 30.53518628210144570, 5.770363421893814682 ) ) ;
#16754 = CARTESIAN_POINT ( 'NONE',  ( -13.62178482187500528, 196.1281250006145171, -23.59362340125807123 ) ) ;
#16755 = CARTESIAN_POINT ( 'NONE',  ( -13.62178482187500528, 197.9843750006145626, -23.59362340125807123 ) ) ;
#16756 = DIRECTION ( 'NONE',  ( 1.000000000000000000, 0.000000000000000000, 0.000000000000000000 ) ) ;
#16757 = CARTESIAN_POINT ( 'NONE',  ( 37.23322021648719726, 3.464101615137916035, 166.7042766426847322 ) ) ;
#16758 = DIRECTION ( 'NONE',  ( 0.000000000000000000, 0.000000000000000000, -1.000000000000000000 ) ) ;
#16759 = CARTESIAN_POINT ( 'NONE',  ( 10.56230152254410903, 7.347880794884117764E-16, -10.00000000000000000 ) ) ;
#16760 = CARTESIAN_POINT ( 'NONE',  ( 23.87821517812499650, 248.8093750006145228, -4.985214923628404904 ) ) ;
#16761 = CARTESIAN_POINT ( 'NONE',  ( 3.474262827703532341, 119.7648137178985905, -8.843639120294245259 ) ) ;
#16762 = CARTESIAN_POINT ( 'NONE',  ( 23.87821517812499650, 241.1593750006145171, -4.985214923628404904 ) ) ;
#16763 = VERTEX_POINT ( 'NONE', #29593 ) ;
#16764 = CARTESIAN_POINT ( 'NONE',  ( -68.60788769728823411, 216.4690446883607535, 1.857196546604031662 ) ) ;
#16765 = DIRECTION ( 'NONE',  ( 0.000000000000000000, 0.000000000000000000, 1.000000000000000000 ) ) ;
#16766 = CIRCLE ( 'NONE', #34315, 4.899999999999999467 ) ;
#16767 = CARTESIAN_POINT ( 'NONE',  ( 21.00000000000000000, 247.9187500012290570, 6.928203230275506996 ) ) ;
#16768 = CARTESIAN_POINT ( 'NONE',  ( 0.1745138560722779009, 123.7898137178985678, 12.50000000000000355 ) ) ;
#16769 = CARTESIAN_POINT ( 'NONE',  ( 16.56230152254411081, 7.209453229046475009, -8.353124999385522997 ) ) ;
#16770 = CARTESIAN_POINT ( 'NONE',  ( 30.84832656884210067, 7.209453229046475009, 162.5668877765479863 ) ) ;
#16771 = CARTESIAN_POINT ( 'NONE',  ( 15.00000000000000355, 7.347880794884112834E-16, -8.000000000000000000 ) ) ;
#16772 = CARTESIAN_POINT ( 'NONE',  ( 5.727106289114498080E-15, 195.6125000000000398, 31.17691453623979214 ) ) ;
#16773 = EDGE_CURVE ( 'NONE', #29577, #31993, #12730, .T. ) ;
#16774 = ORIENTED_EDGE ( 'NONE', *, *, #8770, .T. ) ;
#16775 = EDGE_LOOP ( 'NONE', ( #32052, #30295, #18614, #28343 ) ) ;
#16776 = ORIENTED_EDGE ( 'NONE', *, *, #13301, .F. ) ;
#16777 = CARTESIAN_POINT ( 'NONE',  ( 18.00000000000000000, 5.196152422706630247, -4.518749998770942966 ) ) ;
#16778 = CARTESIAN_POINT ( 'NONE',  ( 15.24356964374999990, 0.000000000000000000, -1.940624999385465177 ) ) ;
#16779 = CARTESIAN_POINT ( 'NONE',  ( 22.56230152254411792, 7.347880794884125653E-16, -0.6750000000000366818 ) ) ;
#16780 = CARTESIAN_POINT ( 'NONE',  ( 20.99999999999999645, 185.0294372515228645, 0.000000000000000000 ) ) ;
#16781 = CARTESIAN_POINT ( 'NONE',  ( 15.24356964374999990, 249.7468750006145228, 0.000000000000000000 ) ) ;
#16782 = CARTESIAN_POINT ( 'NONE',  ( -6.932735513423968321, 60.14768628210144641, -10.69584247140445221 ) ) ;
#16783 = CARTESIAN_POINT ( 'NONE',  ( -57.91294563604515844, 214.6737587650350747, -4.842901733360248429 ) ) ;
#16784 = EDGE_CURVE ( 'NONE', #37177, #30702, #15586, .T. ) ;
#16785 = CARTESIAN_POINT ( 'NONE',  ( 15.04813726045348687, 225.8716339721264319, 0.7835069059938112312 ) ) ;
#16786 = CARTESIAN_POINT ( 'NONE',  ( -41.48586230271182984, 207.8500491399821613, 3.954877714930852495 ) ) ;
#16787 = CYLINDRICAL_SURFACE ( 'NONE', #32323, 5.999999999999999112 ) ;
#16788 = CARTESIAN_POINT ( 'NONE',  ( 33.96029051149804445, -5.196152422706629359, 163.7156586684033073 ) ) ;
#16789 = CARTESIAN_POINT ( 'NONE',  ( 2.660918448318002838, 123.5023137178985735, 12.46528703574811558 ) ) ;
#16790 = CARTESIAN_POINT ( 'NONE',  ( -36.74330436395489841, 210.1155267958017134, -6.500000000000000888 ) ) ;
#16791 = CARTESIAN_POINT ( 'NONE',  ( -47.23288769728824121, 201.5309553116392181, -2.393094931466246855 ) ) ;
#16792 = ADVANCED_FACE ( 'NONE', ( #4932 ), #19371, .F. ) ;
#16793 = CARTESIAN_POINT ( 'NONE',  ( 26.75643035624999655, 3.323476615752271268, -3.140624999385464022 ) ) ;
#16794 = CARTESIAN_POINT ( 'NONE',  ( 13.62178482187501416, 195.4531250006145342, 23.59362340125806767 ) ) ;
#16795 = CARTESIAN_POINT ( 'NONE',  ( -15.53471296425188442, 89.57731371789856212, -2.908627838312459080 ) ) ;
#16796 = CARTESIAN_POINT ( 'NONE',  ( -64.84002896937849414, 202.6965474657332038, 4.350049139982197666 ) ) ;
#16797 = VECTOR ( 'NONE', #7597, 1000.000000000000114 ) ;
#16798 = EDGE_CURVE ( 'NONE', #32409, #32329, #33384, .T. ) ;
#16799 = ORIENTED_EDGE ( 'NONE', *, *, #29045, .F. ) ;
#16800 = CARTESIAN_POINT ( 'NONE',  ( 15.00000000000000000, 0.000000000000000000, -7.200000000000011724 ) ) ;
#16801 = CARTESIAN_POINT ( 'NONE',  ( 10.49813415415989581, 128.5726862821014720, 7.228626920339068285 ) ) ;
#16802 = CARTESIAN_POINT ( 'NONE',  ( -8.927990412390661490, 57.27268628210143220, 13.04141134922759804 ) ) ;
#16803 = EDGE_CURVE ( 'NONE', #23009, #24665, #6616, .T. ) ;
#16804 = DIRECTION ( 'NONE',  ( 0.08715574274765150453, 0.000000000000000000, 0.9961946980917461003 ) ) ;
#16805 = CARTESIAN_POINT ( 'NONE',  ( 24.59092967851185207, 3.604726614523240613, 162.6814417626936518 ) ) ;
#16806 = CARTESIAN_POINT ( 'NONE',  ( 11.08355503943142750, 80.56018628210146915, -10.83675517735155225 ) ) ;
#16807 = CARTESIAN_POINT ( 'NONE',  ( 10.31873187879411091, -3.604726614523240613, -7.753124999385540228 ) ) ;
#16808 =( BOUNDED_CURVE ( )  B_SPLINE_CURVE ( 2, ( #36793, #10835, #13879, #33958, #36418, #25427, #16348 ),
 .UNSPECIFIED., .F., .F. ) 
 B_SPLINE_CURVE_WITH_KNOTS ( ( 3, 2, 2, 3 ),
 ( 0.6086956521739130821, 0.6159420289855073172, 0.6231884057971015523, 0.6304347826086958984 ),
 .UNSPECIFIED. ) 
 CURVE ( )  GEOMETRIC_REPRESENTATION_ITEM ( )  RATIONAL_B_SPLINE_CURVE ( ( 1.000000000000000000, 0.8660254037844387076, 1.000000000000000000, 0.8660254037844387076, 1.000000000000000000, 0.8660254037844345998, 1.000000000000003997 ) ) 
 REPRESENTATION_ITEM ( '' )  );
#16809 = CARTESIAN_POINT ( 'NONE',  ( -5.529263428287477744, 29.67268628210143788, 7.954856959092191815 ) ) ;
#16810 = CARTESIAN_POINT ( 'NONE',  ( 27.70204505258639216, -5.196152422706632912, 161.0258652235433487 ) ) ;
#16811 = CARTESIAN_POINT ( 'NONE',  ( -61.28497103062156981, 204.4285982733020148, -3.350049139982115509 ) ) ;
#16812 = CARTESIAN_POINT ( 'NONE',  ( 15.00000000000000178, 249.1375000000000171, 3.464101615137757051 ) ) ;
#16813 = CARTESIAN_POINT ( 'NONE',  ( -6.932735513423968321, 60.14768628210144641, -10.69584247140445221 ) ) ;
#16814 = CARTESIAN_POINT ( 'NONE',  ( -27.00000000000000355, 198.6125000000000398, -15.58845726811989429 ) ) ;
#16815 = CARTESIAN_POINT ( 'NONE',  ( 2.999999999999997335, 237.0000000000000000, 5.000000000000000000 ) ) ;
#16817 = CARTESIAN_POINT ( 'NONE',  ( 19.68408634441911076, 5.407089921784862696, -2.146874999385511629 ) ) ;
#16816 = CARTESIAN_POINT ( 'NONE',  ( -5.233372021372430183, 32.54768628210143788, -8.152565276336710909 ) ) ;
#16818 = DIRECTION ( 'NONE',  ( 1.000000000000000000, 0.000000000000000000, 0.000000000000000000 ) ) ;
#16819 = EDGE_LOOP ( 'NONE', ( #31409, #24861, #28522, #16272 ) ) ;
#16820 = CARTESIAN_POINT ( 'NONE',  ( 15.00000000000000000, 0.000000000000000000, -3.599999999999992095 ) ) ;
#16821 = PRODUCT ( 'Cylinder', 'Cylinder', '', ( #6962 ) ) ;
#16822 = CARTESIAN_POINT ( 'NONE',  ( 24.35560917309319251, 3.604726614523240613, 159.9917160778459220 ) ) ;
#16823 = CARTESIAN_POINT ( 'NONE',  ( 10.31873187879411091, 3.604726614523236616, -1.528124999385498173 ) ) ;
#16824 = CARTESIAN_POINT ( 'NONE',  ( 25.14491336835161306, 3.604726614523236616, 169.0135043124392951 ) ) ;
#16825 = CARTESIAN_POINT ( 'NONE',  ( 26.99999999999999645, 243.5124999999999602, -3.464101615137755275 ) ) ;
#16826 = CARTESIAN_POINT ( 'NONE',  ( -7.234628195640302017, 198.7424038105676800, 27.00000000000000711 ) ) ;
#16827 = CARTESIAN_POINT ( 'NONE',  ( -4.944772684328673229, 93.78518628210144925, 11.48171059495397728 ) ) ;
#16828 = ORIENTED_EDGE ( 'NONE', *, *, #26777, .T. ) ;
#16829 = ORIENTED_EDGE ( 'NONE', *, *, #1831, .T. ) ;
#16830 = CARTESIAN_POINT ( 'NONE',  ( 27.00000000000001066, 196.2500000012290116, 15.58845726811988897 ) ) ;
#16831 = CARTESIAN_POINT ( 'NONE',  ( 30.75272761356932705, 6.928203230275506996, 161.4741867176907988 ) ) ;
#16832 = EDGE_CURVE ( 'NONE', #18251, #9681, #24550, .T. ) ;
#16833 = CARTESIAN_POINT ( 'NONE',  ( 14.38691631536194393, 39.26481371789855501, 5.770363421894124656 ) ) ;
#16834 = CARTESIAN_POINT ( 'NONE',  ( 23.87821517812500005, -4.985214923628404016, -8.203124999385469351 ) ) ;
#16835 = CARTESIAN_POINT ( 'NONE',  ( 15.24356964374999990, 244.0093750006145399, 0.000000000000000000 ) ) ;
#16836 =( BOUNDED_CURVE ( )  B_SPLINE_CURVE ( 2, ( #26438, #28723, #5789, #37436, #29471, #470, #3507 ),
 .UNSPECIFIED., .F., .F. ) 
 B_SPLINE_CURVE_WITH_KNOTS ( ( 3, 2, 2, 3 ),
 ( 0.3913043478260864183, 0.3985507246376804869, 0.4057971014492746109, 0.4130434782608686795 ),
 .UNSPECIFIED. ) 
 CURVE ( )  GEOMETRIC_REPRESENTATION_ITEM ( )  RATIONAL_B_SPLINE_CURVE ( ( 1.000000000000010214, 0.8660254037844284936, 1.000000000000000000, 0.8660254037844387076, 1.000000000000000000, 0.8660254037844551389, 0.9999999999999835687 ) ) 
 REPRESENTATION_ITEM ( '' )  );
#16837 = AXIS2_PLACEMENT_3D ( 'NONE', #25200, #19350, #4544 ) ;
#16838 = CARTESIAN_POINT ( 'NONE',  ( -41.69122103062156270, 208.9097554298617752, -4.530955311639240257 ) ) ;
#16839 = CARTESIAN_POINT ( 'NONE',  ( 18.00000000000000000, 5.196152422706630247, -7.275000000000003908 ) ) ;
#16840 = CARTESIAN_POINT ( 'NONE',  ( 24.55170959427540822, 3.604726614523240613, 162.2331541485523587 ) ) ;
#16841 = CARTESIAN_POINT ( 'NONE',  ( -6.840914352311947333, 35.23981371789855643, -6.594114490232462877 ) ) ;
#16842 = ADVANCED_FACE ( 'NONE', ( #28061 ), #30731, .T. ) ;
#16843 = CARTESIAN_POINT ( 'NONE',  ( -67.22247103062156270, 206.6499508600178672, 5.571401726697986057 ) ) ;
#16844 = CARTESIAN_POINT ( 'NONE',  ( -1.715153634034442431, 87.27731371789855075, 9.534712964251900402 ) ) ;
#16845 = CARTESIAN_POINT ( 'NONE',  ( -27.24356964375000345, 197.6093750006145342, 0.000000000000000000 ) ) ;
#16846 = CARTESIAN_POINT ( 'NONE',  ( 11.61527771782809637, 20.86481371789854222, 4.622313124798827388 ) ) ;
#16847 = EDGE_CURVE ( 'NONE', #30367, #16244, #10480, .T. ) ;
#16848 = CARTESIAN_POINT ( 'NONE',  ( 11.48171059495397728, 73.08518628210144641, 4.944772684328674117 ) ) ;
#16849 = CARTESIAN_POINT ( 'NONE',  ( 14.47852538368266195, 5.725134515572932514, -10.32395279703524871 ) ) ;
#16850 = PLANE ( 'NONE',  #3551 ) ;
#16851 = AXIS2_PLACEMENT_3D ( 'NONE', #26426, #89, #37425 ) ;
#16852 = CARTESIAN_POINT ( 'NONE',  ( 37.56329110859752518, 7.646167579472024665E-16, 167.6823559553839971 ) ) ;
#16853 = DIRECTION ( 'NONE',  ( -0.000000000000000000, 0.000000000000000000, 1.000000000000000000 ) ) ;
#16854 = CARTESIAN_POINT ( 'NONE',  ( 10.31873187879410736, 0.000000000000000000, -6.046874999385526195 ) ) ;
#16855 = CARTESIAN_POINT ( 'NONE',  ( 10.56230152254410903, 0.000000000000000000, -0.7874999987710074034 ) ) ;
#16856 = CARTESIAN_POINT ( 'NONE',  ( 2.064181346179272847, 79.69768628210141515, -9.465287035748065847 ) ) ;
#16857 = FACE_OUTER_BOUND ( 'NONE', #1850, .T. ) ;
#16858 = CARTESIAN_POINT ( 'NONE',  ( -0.1745138560725500443, 111.6101862821014521, 12.50000000000000355 ) ) ;
#16859 = CARTESIAN_POINT ( 'NONE',  ( 26.99999999999999645, 248.9125000000000227, -3.464101615137755275 ) ) ;
#16860 = CARTESIAN_POINT ( 'NONE',  ( 3.306546357697853733E-15, 210.0000000000000284, 27.00000000000000000 ) ) ;
#16861 = VERTEX_POINT ( 'NONE', #10626 ) ;
#16862 = CARTESIAN_POINT ( 'NONE',  ( 36.94394061169700905, 3.604726614523238837, 160.6031473820695226 ) ) ;
#16863 = CARTESIAN_POINT ( 'NONE',  ( 21.00000000000000000, -6.646953231504538984, -4.528124999385448213 ) ) ;
#16864 = CARTESIAN_POINT ( 'NONE',  ( -27.24356964375000345, 195.8093750006145513, 0.000000000000000000 ) ) ;
#16865 = CARTESIAN_POINT ( 'NONE',  ( 37.59924285248093412, -3.604726614523238837, 168.0932862683468159 ) ) ;
#16866 = CARTESIAN_POINT ( 'NONE',  ( 25.16449192692313019, 3.464101615137757051, 166.4426400131867467 ) ) ;
#16867 = CARTESIAN_POINT ( 'NONE',  ( 27.00000000000013500, 3.464101615137676227, -0.1875000000000186240 ) ) ;
#16868 = CARTESIAN_POINT ( 'NONE',  ( 18.12178482187499640, 239.8843750006145115, -4.985214923628404904 ) ) ;
#16869 = CARTESIAN_POINT ( 'NONE',  ( 27.24356964374999279, 199.1656250006145399, -15.72908226750539207 ) ) ;
#16870 = CARTESIAN_POINT ( 'NONE',  ( -12.53471296425189152, 117.1773137178985564, -2.311890736173453753 ) ) ;
#16871 = CARTESIAN_POINT ( 'NONE',  ( -13.62178482187500528, 195.2843750006145456, -23.59362340125807123 ) ) ;
#16873 = VERTEX_POINT ( 'NONE', #13291 ) ;
#16872 = EDGE_LOOP ( 'NONE', ( #11541, #14134, #20226, #17540 ) ) ;
#16874 =( BOUNDED_CURVE ( )  B_SPLINE_CURVE ( 2, ( #1175, #9531, #12749, #26956, #986, #34919, #8963 ),
 .UNSPECIFIED., .F., .F. ) 
 B_SPLINE_CURVE_WITH_KNOTS ( ( 3, 2, 2, 3 ),
 ( 0.1304347826086947049, 0.1376811594202889955, 0.1449275362318833138, 0.1521739130434776044 ),
 .UNSPECIFIED. ) 
 CURVE ( )  GEOMETRIC_REPRESENTATION_ITEM ( )  RATIONAL_B_SPLINE_CURVE ( ( 1.000000000000017319, 0.8660254037844211661, 1.000000000000000000, 0.8660254037844387076, 1.000000000000000000, 0.8660254037844510311, 0.9999999999999876765 ) ) 
 REPRESENTATION_ITEM ( '' )  );
#16875 = CARTESIAN_POINT ( 'NONE',  ( 15.24356964375000167, 245.2843750006144887, 3.323476615752272600 ) ) ;
#16876 = DIRECTION ( 'NONE',  ( 1.000000000000000000, 0.000000000000000000, 0.000000000000000000 ) ) ;
#16877 = EDGE_CURVE ( 'NONE', #2209, #23009, #1297, .T. ) ;
#16878 = CARTESIAN_POINT ( 'NONE',  ( -15.50000000000000533, 107.6898137178985735, 0.1745138560722471477 ) ) ;
#16879 = LINE ( 'NONE', #19735, #16797 ) ;
#16880 = CARTESIAN_POINT ( 'NONE',  ( 26.75643035624999655, 7.049594010296217766E-16, -2.728124999385489247 ) ) ;
#16881 = CARTESIAN_POINT ( 'NONE',  ( 13.44051670066910908, 5.407089921784862696, -8.821874999385526550 ) ) ;
#16882 = CARTESIAN_POINT ( 'NONE',  ( 13.50000000000001421, 199.3625000012290513, 23.38268590217984055 ) ) ;
#16883 = CARTESIAN_POINT ( 'NONE',  ( -12.50000000000000355, 104.7101862821014606, -0.1745138560725492671 ) ) ;
#16884 = CARTESIAN_POINT ( 'NONE',  ( 13.44051670066911086, 5.407089921784856479, -2.015624999385540406 ) ) ;
#16885 = CARTESIAN_POINT ( 'NONE',  ( -40.69419563604516554, 201.5000000000000000, 0.1155267958018195706 ) ) ;
#16886 = CARTESIAN_POINT ( 'NONE',  ( 26.75643035624999655, 243.6718750006145058, -7.049594010296217766E-16 ) ) ;
#16887 = CARTESIAN_POINT ( 'NONE',  ( -3.253724281355068545E-15, 197.3000000012290229, -27.00000000000000000 ) ) ;
#16888 = CARTESIAN_POINT ( 'NONE',  ( -33.96502896937850124, 213.8393509191290889, -2.350049139982142155 ) ) ;
#16889 = CARTESIAN_POINT ( 'NONE',  ( 4.944772684328679446, 116.7851862821014635, -11.48171059495397373 ) ) ;
#16890 = CARTESIAN_POINT ( 'NONE',  ( 13.56230152254410726, 5.196152422706630247, -2.662499998771022724 ) ) ;
#16891 = CARTESIAN_POINT ( 'NONE',  ( -46.24330436395489841, 210.1155267958017134, -6.500000000000000888 ) ) ;
#16892 = CARTESIAN_POINT ( 'NONE',  ( 3.037124061885436328E-15, 148.0000000000000000, 24.80000000000000426 ) ) ;
#16893 = CARTESIAN_POINT ( 'NONE',  ( 14.25334919248782661, 109.8851862821014720, 6.092822981423971385 ) ) ;
#16894 = CARTESIAN_POINT ( 'NONE',  ( -0.1745138560725500443, 19.61018628210144144, 12.50000000000000355 ) ) ;
#16895 = CARTESIAN_POINT ( 'NONE',  ( 20.99999999999999289, 244.5437500012290570, -5.999999999999997335 ) ) ;
#16896 = CARTESIAN_POINT ( 'NONE',  ( -6.594114490232312775, 124.2601862821014578, -6.840914352312096547 ) ) ;
#16897 = CARTESIAN_POINT ( 'NONE',  ( 16.56230152254411081, 7.209453229046475009, -2.953124999385511096 ) ) ;
#16898 = CARTESIAN_POINT ( 'NONE',  ( 10.56230152254410903, 0.000000000000000000, -3.487499998771015353 ) ) ;
#16899 = ORIENTED_EDGE ( 'NONE', *, *, #12878, .T. ) ;
#16900 = CARTESIAN_POINT ( 'NONE',  ( 19.56230152254411436, -5.196152422706629359, -4.687499998771022192 ) ) ;
#16901 = CARTESIAN_POINT ( 'NONE',  ( -5.529263428287477744, 57.27268628210143220, 7.954856959092191815 ) ) ;
#16902 =( NAMED_UNIT ( * ) SI_UNIT ( $, .STERADIAN. ) SOLID_ANGLE_UNIT ( ) );
#16903 = CARTESIAN_POINT ( 'NONE',  ( -27.24356964375000345, 195.3031250006145285, 0.000000000000000000 ) ) ;
#16904 = DIRECTION ( 'NONE',  ( 0.000000000000000000, 0.000000000000000000, -1.000000000000000000 ) ) ;
#16905 = CARTESIAN_POINT ( 'NONE',  ( 13.62178482187499640, 195.6593750006145456, -23.59362340125807123 ) ) ;
#16906 = EDGE_CURVE ( 'NONE', #26157, #12608, #28250, .T. ) ;
#16907 = CARTESIAN_POINT ( 'NONE',  ( 27.97658564224149558, -5.196152422706632912, 164.1638785225323431 ) ) ;
#16908 = FACE_OUTER_BOUND ( 'NONE', #29343, .T. ) ;
#16909 = CARTESIAN_POINT ( 'NONE',  ( 7.954856959092311719, 65.42731371789857064, -5.529263428287300108 ) ) ;
#16910 = CARTESIAN_POINT ( 'NONE',  ( 26.99999999999999645, 3.464101615137755275, -9.637499999999990408 ) ) ;
#16911 = ORIENTED_EDGE ( 'NONE', *, *, #211, .T. ) ;
#16912 = EDGE_CURVE ( 'NONE', #12420, #815, #3086, .T. ) ;
#16913 = CARTESIAN_POINT ( 'NONE',  ( 18.00000000000000355, 241.1312500012290343, 5.196152422706632912 ) ) ;
#16914 = CARTESIAN_POINT ( 'NONE',  ( -6.932735513424201912, 69.45231371789856212, 10.69584247140429412 ) ) ;
#16915 = CARTESIAN_POINT ( 'NONE',  ( 13.44051670066911441, -5.407089921784865361, -6.421874999385540406 ) ) ;
#16916 = CARTESIAN_POINT ( 'NONE',  ( 26.75643035624999655, 3.323476615752271712, -7.640624999385485339 ) ) ;
#16917 = CARTESIAN_POINT ( 'NONE',  ( 12.50000000000000355, 29.48981371789854933, -0.1745138560722771515 ) ) ;
#16918 = EDGE_CURVE ( 'NONE', #16688, #8056, #28414, .T. ) ;
#16919 = VERTEX_POINT ( 'NONE', #25960 ) ;
#16920 = CARTESIAN_POINT ( 'NONE',  ( 19.68408634441911431, 5.407089921784862696, -0.7968749993855217539 ) ) ;
#16921 = CARTESIAN_POINT ( 'NONE',  ( 2.311890736173175753, 10.12268628210144428, 12.53471296425194836 ) ) ;
#16922 = CARTESIAN_POINT ( 'NONE',  ( 37.56655944895057075, 3.604726614523243278, 167.7197132565624713 ) ) ;
#16923 = CARTESIAN_POINT ( 'NONE',  ( -39.90252896937850124, 206.6499508600178387, -5.571401726697954970 ) ) ;
#16924 = DIRECTION ( 'NONE',  ( -0.000000000000000000, -0.000000000000000000, 1.000000000000000000 ) ) ;
#16925 = CARTESIAN_POINT ( 'NONE',  ( -10.06240783497716862, 195.0000000000000000, 25.33096707650729584 ) ) ;
#16926 = CARTESIAN_POINT ( 'NONE',  ( -35.35788769728823411, 214.4690446883608104, 1.321298161741840893 ) ) ;
#16927 = CARTESIAN_POINT ( 'NONE',  ( -45.05580436395489841, 216.5000000000000000, 0.1155267958017343610 ) ) ;
#16928 = CARTESIAN_POINT ( 'NONE',  ( 28.25155051613373658, 5.407089921784856479, 168.7040655364119743 ) ) ;
#16929 = EDGE_LOOP ( 'NONE', ( #27431, #19818, #11756, #19385 ) ) ;
#16930 = LINE ( 'NONE', #20145, #27013 ) ;
#16931 = CARTESIAN_POINT ( 'NONE',  ( 20.99999999999999645, 6.928203230275506996, -1.406249998770969123 ) ) ;
#16932 = CARTESIAN_POINT ( 'NONE',  ( 8.632099005475788900, 28.05231371789855643, -13.23911966647199812 ) ) ;
#16933 = CARTESIAN_POINT ( 'NONE',  ( -68.40997103062156270, 217.3034525342668815, 4.350049139982096413 ) ) ;
#16934 = CARTESIAN_POINT ( 'NONE',  ( -2.064181346179269738, 139.4976862821014549, 9.465287035748067623 ) ) ;
#16935 = CARTESIAN_POINT ( 'NONE',  ( 10.49813415415989581, 54.97268628210144925, 7.228626920339068285 ) ) ;
#16936 = CARTESIAN_POINT ( 'NONE',  ( 13.56230152254410903, 5.196152422706636465, -3.225000000000033396 ) ) ;
#16937 = DIRECTION ( 'NONE',  ( -0.000000000000000000, 0.000000000000000000, 1.000000000000000000 ) ) ;
#16938 = ORIENTED_EDGE ( 'NONE', *, *, #11477, .T. ) ;
#16939 = CARTESIAN_POINT ( 'NONE',  ( 14.38691631536207538, 7.535186282101451916, -5.770363421893813793 ) ) ;
#16940 = DIRECTION ( 'NONE',  ( -0.9933043639548644332, 0.1155267958017622554, 0.000000000000000000 ) ) ;
#16941 = CARTESIAN_POINT ( 'NONE',  ( -1.926257025242585782E-15, 198.3968750006145285, -31.45816453501075927 ) ) ;
#16942 = DIRECTION ( 'NONE',  ( 0.000000000000000000, 0.000000000000000000, -1.000000000000000000 ) ) ;
#16943 = CARTESIAN_POINT ( 'NONE',  ( -31.99330436395490196, 210.1155267958017134, -6.500000000000000888 ) ) ;
#16944 = CYLINDRICAL_SURFACE ( 'NONE', #12203, 5.999999999999999112 ) ;
#16945 = CARTESIAN_POINT ( 'NONE',  ( 19.39230484541326760, 240.2486538117967427, 5.999999999999999112 ) ) ;
#16946 = CARTESIAN_POINT ( 'NONE',  ( 26.75643035624999655, 246.9718750006145740, -3.323476615752271712 ) ) ;
#16947 = CARTESIAN_POINT ( 'NONE',  ( -0.1745138560723084320, 119.1898137178985593, -9.500000000000005329 ) ) ;
#16948 = CARTESIAN_POINT ( 'NONE',  ( 15.24356964374999990, 241.7593750006145399, 0.000000000000000000 ) ) ;
#16949 = EDGE_LOOP ( 'NONE', ( #29213, #10701, #27123 ) ) ;
#16950 = CARTESIAN_POINT ( 'NONE',  ( -66.23288769728823411, 203.5309553116391612, -1.857196546604028775 ) ) ;
#16951 = CARTESIAN_POINT ( 'NONE',  ( -27.00000000000000355, 195.9500000000000171, 0.000000000000000000 ) ) ;
#16952 = CARTESIAN_POINT ( 'NONE',  ( 21.00000000000000000, 249.2687500012290229, 6.928203230275506996 ) ) ;
#16953 = CARTESIAN_POINT ( 'NONE',  ( -7.228626920338836470, 118.3273137178985621, -10.49813415416005213 ) ) ;
#16954 = CARTESIAN_POINT ( 'NONE',  ( 10.31873187879411091, 3.604726614523236616, -10.07812499938551198 ) ) ;
#16955 = CARTESIAN_POINT ( 'NONE',  ( 36.97989235558041798, 7.646167579472015790E-16, 161.0140776950323698 ) ) ;
#16956 = DIRECTION ( 'NONE',  ( -0.000000000000000000, -0.000000000000000000, 1.000000000000000000 ) ) ;
#16957 = CARTESIAN_POINT ( 'NONE',  ( -13.49999999999998401, 195.5749999999999886, 23.38268590217985476 ) ) ;
#16958 = VERTEX_POINT ( 'NONE', #8717 ) ;
#16959 = ORIENTED_EDGE ( 'NONE', *, *, #15502, .F. ) ;
#16960 = ORIENTED_EDGE ( 'NONE', *, *, #36975, .F. ) ;
#16961 = CARTESIAN_POINT ( 'NONE',  ( 21.00000000000000000, -6.928203230275506996, -7.481249998770959309 ) ) ;
#16962 = CARTESIAN_POINT ( 'NONE',  ( 20.99999999999999645, -6.646953231504538984, -2.278124999385469529 ) ) ;
#16963 = CARTESIAN_POINT ( 'NONE',  ( 18.00000000000000000, 5.196152422706630247, -6.374999999999992006 ) ) ;
#16964 = CARTESIAN_POINT ( 'NONE',  ( 22.60769515458672885, 248.0674038105676402, -6.000000000000000000 ) ) ;
#16965 = CARTESIAN_POINT ( 'NONE',  ( 26.75643035624999655, 249.4843750006145058, 3.323476615752267715 ) ) ;
#16966 = CARTESIAN_POINT ( 'NONE',  ( -8.715434833791929847, 59.86018628210145209, -8.962234695871762469 ) ) ;
#16967 = CARTESIAN_POINT ( 'NONE',  ( -62.86086230271182984, 213.1499508600178387, -5.686928522499747451 ) ) ;
#16968 = ADVANCED_FACE ( 'NONE', ( #34858 ), #23129, .F. ) ;
#16969 = CARTESIAN_POINT ( 'NONE',  ( 15.80103094669415498, 223.8639174754799797, 3.001545256183678401 ) ) ;
#16970 = CARTESIAN_POINT ( 'NONE',  ( -37.72544563604516554, 213.3788001182224718, 3.209657149897419348 ) ) ;
#16971 = CARTESIAN_POINT ( 'NONE',  ( 25.05990503573306682, 0.000000000000000000, 165.2472063767010013 ) ) ;
#16972 = CARTESIAN_POINT ( 'NONE',  ( 12.53471296425189330, 112.5773137178985621, 2.311890736173451977 ) ) ;
#16973 = CARTESIAN_POINT ( 'NONE',  ( -68.80580436395490551, 214.5000000000000284, 0.1155267958017899832 ) ) ;
#16974 = CARTESIAN_POINT ( 'NONE',  ( -49.01413769728823411, 214.1499508600179240, 7.418979330068584233 ) ) ;
#16975 = CARTESIAN_POINT ( 'NONE',  ( 20.99999999999999645, -6.646953231504538984, -5.540624999385494576 ) ) ;
#16976 = CARTESIAN_POINT ( 'NONE',  ( 18.00000000000000000, 5.196152422706630247, -0.5249999999999976907 ) ) ;
#16977 = CARTESIAN_POINT ( 'NONE',  ( 0.1745138560722461762, 86.98981371789857064, 15.50000000000000533 ) ) ;
#16978 = CARTESIAN_POINT ( 'NONE',  ( -38.71502896937850124, 215.5714017266979567, -3.350049139982168800 ) ) ;
#16979 = VERTEX_POINT ( 'NONE', #3020 ) ;
#16980 = CARTESIAN_POINT ( 'NONE',  ( 2.999999999999997335, 244.5000000000000000, 5.000000000000000888 ) ) ;
#16981 = CARTESIAN_POINT ( 'NONE',  ( 8.962234695871762469, 108.1601862821014635, -8.715434833791931624 ) ) ;
#16982 = EDGE_CURVE ( 'NONE', #6278, #27573, #14404, .T. ) ;
#16983 = CARTESIAN_POINT ( 'NONE',  ( -6.092822981423970496, 66.18518628210145494, 14.25334919248782661 ) ) ;
#16984 = DIRECTION ( 'NONE',  ( 1.000000000000000000, 0.000000000000000000, -0.000000000000000000 ) ) ;
#16985 = CARTESIAN_POINT ( 'NONE',  ( 37.12860184164360788, -3.604726614523238837, 162.7138348986514131 ) ) ;
#16986 = AXIS2_PLACEMENT_3D ( 'NONE', #14615, #203, #34515 ) ;
#16987 = EDGE_CURVE ( 'NONE', #5563, #6369, #32286, .T. ) ;
#16988 = CARTESIAN_POINT ( 'NONE',  ( 0.1745138560725837118, 61.01018628210145067, -15.50000000000000533 ) ) ;
#16989 = CARTESIAN_POINT ( 'NONE',  ( 22.80587116629410360, -3.604726614523235284, -6.253124999385533123 ) ) ;
#16990 = CARTESIAN_POINT ( 'NONE',  ( 8.710071997420127943, 27.08518628210144996, 3.796722387233375073 ) ) ;
#16991 = CARTESIAN_POINT ( 'NONE',  ( 25.12854018303972126, 0.000000000000000000, 166.0317097002238995 ) ) ;
#16992 = CARTESIAN_POINT ( 'NONE',  ( -59.30580436395489841, 216.5000000000000000, 0.1155267958017343610 ) ) ;
#16993 = CARTESIAN_POINT ( 'NONE',  ( 0.1745138560725515708, 51.81018628210144783, -12.50000000000000355 ) ) ;
#16994 = CARTESIAN_POINT ( 'NONE',  ( -13.49999999999998401, 198.7250000000000227, 23.38268590217985476 ) ) ;
#16995 = LINE ( 'NONE', #10557, #15981 ) ;
#16997 = CARTESIAN_POINT ( 'NONE',  ( 10.31873187879410558, 3.604726614523240613, -2.484374999385500882 ) ) ;
#16996 = CARTESIAN_POINT ( 'NONE',  ( -5.529263428287477744, 29.67268628210143788, 7.954856959092191815 ) ) ;
#16998 = CARTESIAN_POINT ( 'NONE',  ( 26.75643035624999655, 249.1468750006145001, 3.323476615752267271 ) ) ;
#16999 = ORIENTED_EDGE ( 'NONE', *, *, #13446, .T. ) ;
#17000 = CARTESIAN_POINT ( 'NONE',  ( 21.00000000000000000, -6.928203230275506996, -5.287499999999990763 ) ) ;
#17001 = FACE_OUTER_BOUND ( 'NONE', #11210, .T. ) ;
#17002 = CARTESIAN_POINT ( 'NONE',  ( 36.82137784845814821, 3.604726614523243278, 159.2022485878780174 ) ) ;
#17003 = CARTESIAN_POINT ( 'NONE',  ( 10.31873187879411446, -3.604726614523240613, -2.803124999385555149 ) ) ;
#17004 = CARTESIAN_POINT ( 'NONE',  ( 36.59589384753818564, 3.464101615137759271, 159.4196029116644695 ) ) ;
#17005 = CARTESIAN_POINT ( 'NONE',  ( 18.00000000000000355, 243.3250000000000171, 5.196152422706632912 ) ) ;
#17006 = CARTESIAN_POINT ( 'NONE',  ( -13.49999999999998401, 196.5875000012290457, 23.38268590217985476 ) ) ;
#17007 = EDGE_CURVE ( 'NONE', #2700, #10334, #32118, .T. ) ;
#17008 = CARTESIAN_POINT ( 'NONE',  ( -0.1745138560725500443, 74.81018628210145494, 12.50000000000000355 ) ) ;
#17009 = EDGE_LOOP ( 'NONE', ( #34505, #5539, #5632, #7633 ) ) ;
#17010 = ORIENTED_EDGE ( 'NONE', *, *, #26495, .T. ) ;
#17011 = CARTESIAN_POINT ( 'NONE',  ( -27.00000000000000355, 196.9625000012290172, 0.000000000000000000 ) ) ;
#17012 = CARTESIAN_POINT ( 'NONE',  ( 15.00000000000021316, 3.464101615137874735, -4.931249998770944387 ) ) ;
#17013 = CARTESIAN_POINT ( 'NONE',  ( -6.092822981423666739, 35.81481371789853796, -14.25334919248795096 ) ) ;
#17014 = CARTESIAN_POINT ( 'NONE',  ( 23.87821517812499650, 4.985214923628404904, -8.953124999385497773 ) ) ;
#17015 = EDGE_CURVE ( 'NONE', #36216, #18565, #31526, .T. ) ;
#17016 = CARTESIAN_POINT ( 'NONE',  ( 23.87821517812499650, 242.0593750006145228, -4.985214923628404904 ) ) ;
#17017 = VECTOR ( 'NONE', #24252, 1000.000000000000000 ) ;
#17018 = CARTESIAN_POINT ( 'NONE',  ( -44.06622103062156270, 211.0902445701382533, 4.530955311639240257 ) ) ;
#17019 = CARTESIAN_POINT ( 'NONE',  ( 26.99999999999999645, 7.347880794884117764E-16, -6.468749998770951137 ) ) ;
#17020 = CARTESIAN_POINT ( 'NONE',  ( 24.59746635921792546, -3.604726614523244610, 162.7561563650505150 ) ) ;
#17021 = CARTESIAN_POINT ( 'NONE',  ( -1.715153634034442431, 32.07731371789855501, 9.534712964251900402 ) ) ;
#17022 = CARTESIAN_POINT ( 'NONE',  ( 22.80587116629411071, 3.604726614523238837, -9.328124999385510208 ) ) ;
#17023 = DIRECTION ( 'NONE',  ( 0.000000000000000000, 0.000000000000000000, 1.000000000000000000 ) ) ;
#17024 = CARTESIAN_POINT ( 'NONE',  ( 26.94731760015625355, 195.0000000000000284, -2.887353354705169739 ) ) ;
#17025 = CARTESIAN_POINT ( 'NONE',  ( -13.62178482187498396, 197.2343750006145626, 23.59362340125808188 ) ) ;
#17026 = CARTESIAN_POINT ( 'NONE',  ( 12.50000000000000355, 20.28981371789855004, -0.1745138560722771515 ) ) ;
#17027 = VERTEX_POINT ( 'NONE', #17821 ) ;
#17028 =( BOUNDED_CURVE ( )  B_SPLINE_CURVE ( 2, ( #1432, #18139, #1622, #33463, #13193, #12812, #24009, #24381, #12439 ),
 .UNSPECIFIED., .F., .F. ) 
 B_SPLINE_CURVE_WITH_KNOTS ( ( 3, 2, 2, 2, 3 ),
 ( 0.4791666666666666852, 0.4861111111111111049, 0.5000000000000000000, 0.5138888888888888395, 0.5208333333333333703 ),
 .UNSPECIFIED. ) 
 CURVE ( )  GEOMETRIC_REPRESENTATION_ITEM ( )  RATIONAL_B_SPLINE_CURVE ( ( 0.9330127018922194093, 0.9330127018922196314, 1.000000000000000000, 0.8660254037844387076, 1.000000000000000000, 0.8660254037844387076, 1.000000000000000000, 0.9330127018922187432, 0.9330127018922192983 ) ) 
 REPRESENTATION_ITEM ( '' )  );
#17029 = CARTESIAN_POINT ( 'NONE',  ( 10.69584247140445221, 62.44768628210145778, -6.932735513423970097 ) ) ;
#17030 = CARTESIAN_POINT ( 'NONE',  ( 10.56230152254411259, 3.464101615137752166, -10.27499999877103853 ) ) ;
#17031 = EDGE_CURVE ( 'NONE', #19996, #35202, #6391, .T. ) ;
#17032 = DIRECTION ( 'NONE',  ( -0.000000000000000000, -1.000000000000000000, -0.000000000000000000 ) ) ;
#17033 = CARTESIAN_POINT ( 'NONE',  ( 27.46714883140487373, 5.407089921784856479, 159.7383132535862842 ) ) ;
#17034 = CARTESIAN_POINT ( 'NONE',  ( 18.00000000000000355, -5.196152422706632912, -0.7687499987709400795 ) ) ;
#17035 = CARTESIAN_POINT ( 'NONE',  ( 10.31873187879410558, 0.000000000000000000, -8.746874999385534366 ) ) ;
#17036 = SURFACE_SIDE_STYLE ('',( #8318 ) ) ;
#17037 = CARTESIAN_POINT ( 'NONE',  ( -7.954856959092191815, 77.97268628210142083, -5.529263428287477744 ) ) ;
#17038 = DIRECTION ( 'NONE',  ( 0.08715574274765150453, 0.000000000000000000, 0.9961946980917461003 ) ) ;
#17039 = CARTESIAN_POINT ( 'NONE',  ( -4.622313124798576922, 106.4351862821014549, -11.61527771782819762 ) ) ;
#17040 = CARTESIAN_POINT ( 'NONE',  ( -73.23181873377778572, 221.0662276635146384, -0.4999999999999908962 ) ) ;
#17041 = CARTESIAN_POINT ( 'NONE',  ( 16.56230152254410726, 0.000000000000000000, -10.00000000000000000 ) ) ;
#17042 = VERTEX_POINT ( 'NONE', #20098 ) ;
#17043 = AXIS2_PLACEMENT_3D ( 'NONE', #30128, #4160, #553 ) ;
#17044 = CARTESIAN_POINT ( 'NONE',  ( 36.97989235558041798, 7.646167579472015790E-16, 161.0140776950323698 ) ) ;
#17045 = CARTESIAN_POINT ( 'NONE',  ( 26.75643035624999655, 3.323476615752271712, -8.878124999385482496 ) ) ;
#17046 = CARTESIAN_POINT ( 'NONE',  ( 27.24356964374999279, 195.1718750006145342, -15.72908226750539207 ) ) ;
#17047 = CARTESIAN_POINT ( 'NONE',  ( 34.38148213269554532, 5.407089921784862696, 167.1325768043071776 ) ) ;
#17048 = CARTESIAN_POINT ( 'NONE',  ( 25.17102860762920713, -3.464101615137761048, 166.5173546155436100 ) ) ;
#17049 = CARTESIAN_POINT ( 'NONE',  ( 26.99999999999999645, 7.347880794884117764E-16, -2.418749998770952647 ) ) ;
#17050 = CARTESIAN_POINT ( 'NONE',  ( 23.99999999999999645, 249.8499999999999943, -5.196152422706631135 ) ) ;
#17051 = CARTESIAN_POINT ( 'NONE',  ( -1.926257025242585782E-15, 197.4406250006145740, -31.45816453501076637 ) ) ;
#17052 =( BOUNDED_CURVE ( )  B_SPLINE_CURVE ( 2, ( #26595, #626, #3478, #23208, #5944, #3666, #9172 ),
 .UNSPECIFIED., .F., .F. ) 
 B_SPLINE_CURVE_WITH_KNOTS ( ( 3, 2, 2, 3 ),
 ( 0.9130434782608682909, 0.9202898550724624149, 0.9275362318840564280, 0.9347826086956505520 ),
 .UNSPECIFIED. ) 
 CURVE ( )  GEOMETRIC_REPRESENTATION_ITEM ( )  RATIONAL_B_SPLINE_CURVE ( ( 1.000000000000022649, 0.8660254037844161701, 1.000000000000000000, 0.8660254037844387076, 1.000000000000000000, 0.8660254037844694608, 0.9999999999999692468 ) ) 
 REPRESENTATION_ITEM ( '' )  );
#17053 = CARTESIAN_POINT ( 'NONE',  ( -8.715434833792127023, 115.7398137178985706, 8.962234695871568846 ) ) ;
#17054 = CARTESIAN_POINT ( 'NONE',  ( -12.53471296425194659, 122.8226862821014720, 2.311890736173176641 ) ) ;
#17056 = ORIENTED_EDGE ( 'NONE', *, *, #34648, .T. ) ;
#17055 = ORIENTED_EDGE ( 'NONE', *, *, #32981, .T. ) ;
#17057 = CARTESIAN_POINT ( 'NONE',  ( 21.00000000000000000, 241.3093750006145228, 6.646953231504538984 ) ) ;
#17058 = EDGE_CURVE ( 'NONE', #2107, #2079, #31647, .T. ) ;
#17059 = CARTESIAN_POINT ( 'NONE',  ( 19.56230152254412502, -5.196152422706635576, -3.000000000000058176 ) ) ;
#17060 = CARTESIAN_POINT ( 'NONE',  ( 13.23911966647199812, 94.75231371789854506, 8.632099005475788900 ) ) ;
#17061 = CARTESIAN_POINT ( 'NONE',  ( 12.46528703574805874, 100.3976862821014464, 2.660918448318279950 ) ) ;
#17062 = CARTESIAN_POINT ( 'NONE',  ( 15.24356964374999990, 3.323476615752268604, -1.640624999385488891 ) ) ;
#17063 = CARTESIAN_POINT ( 'NONE',  ( 13.50000000000001421, 198.0125000012290286, 23.38268590217984055 ) ) ;
#17064 = AXIS2_PLACEMENT_3D ( 'NONE', #8778, #28668, #2705 ) ;
#17065 = CARTESIAN_POINT ( 'NONE',  ( -10.49813415415989581, 114.7726862821014606, -7.228626920339068285 ) ) ;
#17066 = CARTESIAN_POINT ( 'NONE',  ( 10.31873187879410736, 0.000000000000000000, -4.190624999385549998 ) ) ;
#17067 = CARTESIAN_POINT ( 'NONE',  ( 18.12178482187499640, 243.8218750006145399, -4.985214923628404904 ) ) ;
#17068 = CARTESIAN_POINT ( 'NONE',  ( -55.93377896937850124, 208.3738570449995109, 6.530955311639247363 ) ) ;
#17069 = CARTESIAN_POINT ( 'NONE',  ( -12.46528703574805697, 114.1976862821014720, -2.660918448318280838 ) ) ;
#17070 = CARTESIAN_POINT ( 'NONE',  ( 10.56230152254410903, 0.000000000000000000, -3.487499998771015353 ) ) ;
#17071 = APPLICATION_CONTEXT ( 'automotive_design' ) ;
#17072 = CARTESIAN_POINT ( 'NONE',  ( -41.69122103062155560, 208.3738570449993404, -6.530955311639226935 ) ) ;
#17073 = CYLINDRICAL_SURFACE ( 'NONE', #28835, 5.999999999999998224 ) ;
#17074 = CARTESIAN_POINT ( 'NONE',  ( -3.253724281355068545E-15, 197.6374999999999602, -27.00000000000000355 ) ) ;
#17075 = CARTESIAN_POINT ( 'NONE',  ( 3.257655550457285720, 98.09768628210146346, -15.46528703574804986 ) ) ;
#17076 = CARTESIAN_POINT ( 'NONE',  ( -8.962234695871760692, 20.76018628210144001, 8.715434833791933400 ) ) ;
#17077 = FACE_OUTER_BOUND ( 'NONE', #16929, .T. ) ;
#17078 = ADVANCED_FACE ( 'NONE', ( #26326 ), #362, .F. ) ;
#17079 = CARTESIAN_POINT ( 'NONE',  ( 37.33453876732481547, -3.464101615137594514, 167.8623529779919750 ) ) ;
#17080 = CARTESIAN_POINT ( 'NONE',  ( 5.529263428287477744, 126.2726862821014464, -7.954856959092191815 ) ) ;
#17081 = CARTESIAN_POINT ( 'NONE',  ( 10.31873187879411091, -3.604726614523240613, -2.353124999385527882 ) ) ;
#17082 = CARTESIAN_POINT ( 'NONE',  ( 16.56230152254410726, 6.928203230275506996, -8.999999998771013310 ) ) ;
#17083 = VERTEX_POINT ( 'NONE', #6046 ) ;
#17084 = CARTESIAN_POINT ( 'NONE',  ( 37.64663378759995283, 7.646167579472015790E-16, 168.6349671354342092 ) ) ;
#17085 = CARTESIAN_POINT ( 'NONE',  ( 9.465287035748067623, 54.39768628210144641, 2.064181346179272847 ) ) ;
#17087 = VECTOR ( 'NONE', #513, 1000.000000000000114 ) ;
#17086 =( BOUNDED_CURVE ( )  B_SPLINE_CURVE ( 2, ( #11300, #20026, #2758, #31571, #5594, #7717, #22689, #17180, #30838 ),
 .UNSPECIFIED., .F., .T. ) 
 B_SPLINE_CURVE_WITH_KNOTS ( ( 3, 2, 2, 2, 3 ),
 ( 0.5978260869565217295, 0.6014492753623188470, 0.6086956521739130821, 0.6159420289855072062, 0.6195652173913043237 ),
 .UNSPECIFIED. ) 
 CURVE ( )  GEOMETRIC_REPRESENTATION_ITEM ( )  RATIONAL_B_SPLINE_CURVE ( ( 0.9330127018922194093, 0.9330127018922194093, 1.000000000000000000, 0.8660254037844387076, 1.000000000000000000, 0.8660254037844387076, 1.000000000000000000, 0.9330127018922194093, 0.9330127018922194093 ) ) 
 REPRESENTATION_ITEM ( '' )  );
#17088 = CARTESIAN_POINT ( 'NONE',  ( 23.87821517812500005, -4.985214923628404016, -0.4406249993854638447 ) ) ;
#17089 = CARTESIAN_POINT ( 'NONE',  ( 27.00000000000063238, 3.464101615137388013, -5.137500000000009948 ) ) ;
#17090 = CARTESIAN_POINT ( 'NONE',  ( 18.00000000000000000, 242.3312500012290513, -5.196152422706630247 ) ) ;
#17091 = CARTESIAN_POINT ( 'NONE',  ( -13.62178482187498396, 196.3343750006145285, 23.59362340125808188 ) ) ;
#17092 = CARTESIAN_POINT ( 'NONE',  ( 19.56230152254411436, -5.196152422706629359, -8.737499998771019349 ) ) ;
#17093 = FACE_OUTER_BOUND ( 'NONE', #29440, .T. ) ;
#17094 = CARTESIAN_POINT ( 'NONE',  ( 8.710071997420211432, 47.31481371789856638, -3.796722387233181895 ) ) ;
#17095 = CARTESIAN_POINT ( 'NONE',  ( 15.00000000000000000, 3.464101615137752166, -8.587500000000012790 ) ) ;
#17096 = EDGE_LOOP ( 'NONE', ( #11962, #34188, #35972, #11043 ) ) ;
#17097 = ORIENTED_EDGE ( 'NONE', *, *, #18060, .F. ) ;
#17098 = CARTESIAN_POINT ( 'NONE',  ( 18.12178482187500350, 249.3718750006145228, 4.985214923628407568 ) ) ;
#17099 = CARTESIAN_POINT ( 'NONE',  ( -4.622313124798826500, 59.96481371789855075, 11.61527771782809637 ) ) ;
#17100 = CARTESIAN_POINT ( 'NONE',  ( 22.80587116629411781, -3.604726614523238837, -9.459374999385547156 ) ) ;
#17101 = CARTESIAN_POINT ( 'NONE',  ( 26.75643035624999655, 3.323476615752271712, -8.540624999385476812 ) ) ;
#17102 = CARTESIAN_POINT ( 'NONE',  ( -13.04141134922778456, 143.6273137178985451, 8.927990412390377273 ) ) ;
#17103 = ORIENTED_EDGE ( 'NONE', *, *, #26558, .F. ) ;
#17104 = CARTESIAN_POINT ( 'NONE',  ( 10.31873187879410736, -3.604726614523244610, -0.6093749993855241964 ) ) ;
#17105 = DIRECTION ( 'NONE',  ( -1.000000000000000000, -6.123233995736766036E-17, 0.000000000000000000 ) ) ;
#17106 = CARTESIAN_POINT ( 'NONE',  ( 25.02561894546576582, 0.000000000000000000, 167.6499628194262357 ) ) ;
#17107 = CARTESIAN_POINT ( 'NONE',  ( -41.68377896937849414, 208.3738570449995109, 6.530955311639247363 ) ) ;
#17108 = CARTESIAN_POINT ( 'NONE',  ( 22.56230152254410370, 7.347880794884117764E-16, -0.5624999987710044280 ) ) ;
#17109 = SHAPE_DEFINITION_REPRESENTATION ( #15014, #201 ) ;
#17110 = DIRECTION ( 'NONE',  ( -0.000000000000000000, -0.000000000000000000, 1.000000000000000000 ) ) ;
#17111 = ADVANCED_FACE ( 'NONE', ( #17632 ), #14782, .F. ) ;
#17112 = CARTESIAN_POINT ( 'NONE',  ( -61.07961230271182984, 211.3212981617417938, 4.469044688360757966 ) ) ;
#17113 = VECTOR ( 'NONE', #23614, 1000.000000000000000 ) ;
#17114 = CARTESIAN_POINT ( 'NONE',  ( -46.83705436395489841, 205.3262412349647263, -4.842901733360204020 ) ) ;
#17115 = CARTESIAN_POINT ( 'NONE',  ( -20.74539548491456387, 194.9526013907998276, -17.40745275905709377 ) ) ;
#17116 = ORIENTED_EDGE ( 'NONE', *, *, #2844, .T. ) ;
#17117 = CARTESIAN_POINT ( 'NONE',  ( 10.49999999999999822, 222.9518338469886203, 2.500000000000000000 ) ) ;
#17118 = CARTESIAN_POINT ( 'NONE',  ( 18.00000000000000000, 5.196152422706630247, -0.4687499987709453642 ) ) ;
#17119 = CARTESIAN_POINT ( 'NONE',  ( -13.04141134922778456, 24.02731371789854364, 8.927990412390377273 ) ) ;
#17120 = CARTESIAN_POINT ( 'NONE',  ( -37.92336230271182984, 217.4189793300686233, 4.149950860017807663 ) ) ;
#17121 = CARTESIAN_POINT ( 'NONE',  ( 4.944772684328679446, 6.385186282101440014, -11.48171059495397373 ) ) ;
#17122 = EDGE_CURVE ( 'NONE', #4455, #18743, #3728, .T. ) ;
#17123 = CARTESIAN_POINT ( 'NONE',  ( 12.46528703574805874, 54.39768628210146062, 2.660918448318279950 ) ) ;
#17124 = EDGE_CURVE ( 'NONE', #10985, #31911, #18027, .T. ) ;
#17125 = CARTESIAN_POINT ( 'NONE',  ( 19.56230152254412502, -5.196152422706635576, -4.350000000000076028 ) ) ;
#17126 = VERTEX_POINT ( 'NONE', #6432 ) ;
#17127 = CARTESIAN_POINT ( 'NONE',  ( -6.092822981423970496, 10.98518628210143433, 14.25334919248782661 ) ) ;
#17128 = CARTESIAN_POINT ( 'NONE',  ( 26.99999999999999645, 195.3125000000000000, -15.58845726811990495 ) ) ;
#17129 = CARTESIAN_POINT ( 'NONE',  ( 5.778771075727756162E-15, 196.3718750006145513, 31.45816453501075927 ) ) ;
#17130 = CARTESIAN_POINT ( 'NONE',  ( 30.89980292934887629, 6.928203230275514990, 163.1552652694962546 ) ) ;
#17131 = DIRECTION ( 'NONE',  ( 0.08715574274765143514, 0.000000000000000000, 0.9961946980917462113 ) ) ;
#17132 = DIRECTION ( 'NONE',  ( 0.000000000000000000, 0.000000000000000000, 1.000000000000000000 ) ) ;
#17133 = CARTESIAN_POINT ( 'NONE',  ( 15.00000000000000178, 240.1937500012290627, 3.464101615137757051 ) ) ;
#17134 = CARTESIAN_POINT ( 'NONE',  ( 26.75643035624999655, 245.5843750006145285, -7.049594010296217766E-16 ) ) ;
#17135 = CARTESIAN_POINT ( 'NONE',  ( 1.715153634034445762, 101.0773137178985479, -9.534712964251895073 ) ) ;
#17136 = CARTESIAN_POINT ( 'NONE',  ( 26.75643035624999655, 241.9468750006145399, 3.323476615752267271 ) ) ;
#17137 = ORIENTED_EDGE ( 'NONE', *, *, #24193, .T. ) ;
#17138 = CARTESIAN_POINT ( 'NONE',  ( -62.86830436395490551, 209.8844732041982581, 6.500000000000000888 ) ) ;
#17139 = CARTESIAN_POINT ( 'NONE',  ( 31.14492845593375847, 6.928203230275506996, 165.9570628591036439 ) ) ;
#17140 = CARTESIAN_POINT ( 'NONE',  ( 15.00000000000000000, 249.1562500012290400, 0.000000000000000000 ) ) ;
#17141 = ORIENTED_EDGE ( 'NONE', *, *, #6346, .T. ) ;
#17142 = CARTESIAN_POINT ( 'NONE',  ( 11.48171059495408208, 120.9148137178985536, -4.944772684328420986 ) ) ;
#17143 = CARTESIAN_POINT ( 'NONE',  ( 22.80587116629411781, 7.646167579472024665E-16, -0.4218749993855352987 ) ) ;
#17144 = CARTESIAN_POINT ( 'NONE',  ( 27.59788244552635206, -5.407089921784859143, 161.2326053007238897 ) ) ;
#17145 = CARTESIAN_POINT ( 'NONE',  ( 26.75643035624999655, 3.323476615752271712, -2.690624999385500260 ) ) ;
#17146 = CARTESIAN_POINT ( 'NONE',  ( -12.50000000000000355, 80.08981371789855075, 0.1745138560722786503 ) ) ;
#17147 = CARTESIAN_POINT ( 'NONE',  ( 5.727106289114498080E-15, 196.0625000000000000, 31.17691453623979214 ) ) ;
#17148 = ORIENTED_EDGE ( 'NONE', *, *, #1109, .F. ) ;
#17149 = EDGE_LOOP ( 'NONE', ( #13930, #14481 ) ) ;
#17150 = VERTEX_POINT ( 'NONE', #21042 ) ;
#17151 = CARTESIAN_POINT ( 'NONE',  ( 26.99999999999999645, -3.464101615137751278, -6.056249998770946164 ) ) ;
#17152 = CARTESIAN_POINT ( 'NONE',  ( 20.99999999999999645, 6.646953231504538984, -3.853124999385470595 ) ) ;
#17153 = DIRECTION ( 'NONE',  ( 0.000000000000000000, 0.000000000000000000, -1.000000000000000000 ) ) ;
#17154 = CARTESIAN_POINT ( 'NONE',  ( 20.00041297495057080, 5.668978411116884608, -10.14010147226209035 ) ) ;
#17155 = CARTESIAN_POINT ( 'NONE',  ( -2.660918448318275509, 65.89768628210146062, 12.46528703574805874 ) ) ;
#17156 = CARTESIAN_POINT ( 'NONE',  ( -54.74627896937849414, 203.4690446883607535, -1.626142955000504209 ) ) ;
#17157 = CARTESIAN_POINT ( 'NONE',  ( 21.00000000000005329, 209.9999999999999716, -5.999999999999996447 ) ) ;
#17158 = CARTESIAN_POINT ( 'NONE',  ( -42.27752896937850835, 212.3500491399821613, 3.839350919129088435 ) ) ;
#17159 = SURFACE_STYLE_FILL_AREA ( #31367 ) ;
#17160 = PRESENTATION_LAYER_ASSIGNMENT (  '', '', ( #33498 ) ) ;
#17161 = CARTESIAN_POINT ( 'NONE',  ( 24.94224478302373527, 0.000000000000000000, 163.9023435342771506 ) ) ;
#17162 = CARTESIAN_POINT ( 'NONE',  ( 12.50000000000000355, 103.0898137178985650, -0.1745138560722771515 ) ) ;
#17163 = CARTESIAN_POINT ( 'NONE',  ( -38.12872103062154849, 203.4690446883607535, 1.626142955000567936 ) ) ;
#17164 = CARTESIAN_POINT ( 'NONE',  ( -43.07663769728824121, 202.5810206699313767, 4.149950860017909804 ) ) ;
#17165 = CARTESIAN_POINT ( 'NONE',  ( 23.87821517812500005, -4.985214923628404016, -4.603124999385476812 ) ) ;
#17166 = CARTESIAN_POINT ( 'NONE',  ( 1.069080835302379631E-14, 196.6250000012290400, 27.00000000000000000 ) ) ;
#17167 = CARTESIAN_POINT ( 'NONE',  ( 2.908627838312458636, 73.47731371789855359, -15.53471296425188442 ) ) ;
#17168 = CARTESIAN_POINT ( 'NONE',  ( -38.91294563604516554, 214.6737587650350747, -4.842901733360249317 ) ) ;
#17169 = ORIENTED_EDGE ( 'NONE', *, *, #16559, .F. ) ;
#17170 = CARTESIAN_POINT ( 'NONE',  ( 33.92107042726159705, -5.196152422706629359, 163.2673710542620427 ) ) ;
#17171 = CARTESIAN_POINT ( 'NONE',  ( -11.61527771782819940, 104.1351862821014578, 4.622313124798574258 ) ) ;
#17172 = CARTESIAN_POINT ( 'NONE',  ( 2.908627838312118019, 46.92268628210143788, 15.53471296425195369 ) ) ;
#17173 = CARTESIAN_POINT ( 'NONE',  ( 21.00000000000016342, -4.000000000000002665, 50.00000000000000000 ) ) ;
#17174 = VECTOR ( 'NONE', #33993, 1000.000000000000000 ) ;
#17175 = CARTESIAN_POINT ( 'NONE',  ( 33.85854767620964623, -5.407089921784861808, 161.1554086157566985 ) ) ;
#17176 = CARTESIAN_POINT ( 'NONE',  ( -15.50000000000000533, 58.71018628210145351, -0.1745138560725808530 ) ) ;
#17177 = CARTESIAN_POINT ( 'NONE',  ( 16.56230152254411081, 7.209453229046475009, -6.103124999385545202 ) ) ;
#17178 = CARTESIAN_POINT ( 'NONE',  ( 15.00000000000000355, 7.347880794884112834E-16, -8.000000000000000000 ) ) ;
#17179 = CARTESIAN_POINT ( 'NONE',  ( -52.77455436395490551, 205.1570982666397356, 4.673758765035198159 ) ) ;
#17180 = CARTESIAN_POINT ( 'NONE',  ( 19.39230484541326049, 243.2138461906613713, -5.999999999999997335 ) ) ;
#17181 = CARTESIAN_POINT ( 'NONE',  ( -0.1745138560725500443, 38.01018628210144357, 12.50000000000000355 ) ) ;
#17182 = CARTESIAN_POINT ( 'NONE',  ( 27.00000000000000355, 198.4250000000000114, -3.306546357697854128E-15 ) ) ;
#17183 = CARTESIAN_POINT ( 'NONE',  ( 14.99999999999936229, 3.464101615137384904, -3.581249998770946075 ) ) ;
#17184 = CARTESIAN_POINT ( 'NONE',  ( 2.064181346179272847, 15.29768628210142722, -9.465287035748065847 ) ) ;
#17185 = CARTESIAN_POINT ( 'NONE',  ( 23.87821517812499650, 249.2593750006145399, -4.985214923628404904 ) ) ;
#17186 = EDGE_LOOP ( 'NONE', ( #2764, #37170, #8575, #32249 ) ) ;
#17187 = CARTESIAN_POINT ( 'NONE',  ( 24.00000000000000000, -5.196152422706629359, -4.799999999999998934 ) ) ;
#17188 = CARTESIAN_POINT ( 'NONE',  ( 37.17765843037913953, -3.464101615137540779, 166.0692025214268313 ) ) ;
#17189 = CARTESIAN_POINT ( 'NONE',  ( 36.85732959234155004, 7.646167579472024665E-16, 159.6131789008408646 ) ) ;
#17190 = CARTESIAN_POINT ( 'NONE',  ( 13.44051670066911086, 5.407089921784856479, -4.715624999385548577 ) ) ;
#17191 = CARTESIAN_POINT ( 'NONE',  ( 27.60072650153512441, 5.196152422706636465, 159.8677888857873768 ) ) ;
#17192 = CARTESIAN_POINT ( 'NONE',  ( 15.00000000000000178, 243.2874999999999943, 3.464101615137757051 ) ) ;
#17193 = DIRECTION ( 'NONE',  ( 0.000000000000000000, 1.000000000000000000, 0.000000000000000000 ) ) ;
#17194 = AXIS2_PLACEMENT_3D ( 'NONE', #34236, #36703, #19110 ) ;
#17195 = CARTESIAN_POINT ( 'NONE',  ( 2.311890736173175753, 74.52268628210146062, 12.53471296425194659 ) ) ;
#17196 = ORIENTED_EDGE ( 'NONE', *, *, #27094, .T. ) ;
#17197 = ORIENTED_EDGE ( 'NONE', *, *, #36630, .F. ) ;
#17198 = DIRECTION ( 'NONE',  ( 1.000000000000000000, 0.000000000000000000, 0.000000000000000000 ) ) ;
#17199 = CARTESIAN_POINT ( 'NONE',  ( 13.50000000000001421, 196.2125000012290172, 23.38268590217984055 ) ) ;
#17200 = CARTESIAN_POINT ( 'NONE',  ( 33.73804336749152810, 5.196152422706631135, 161.1753621882693892 ) ) ;
#17201 = CARTESIAN_POINT ( 'NONE',  ( 15.53471296425188797, 48.17731371789854222, 2.908627838312457747 ) ) ;
#17202 = CARTESIAN_POINT ( 'NONE',  ( 26.75643035624999655, 7.049594010296217766E-16, -9.478124999385496352 ) ) ;
#17203 = CARTESIAN_POINT ( 'NONE',  ( 21.00000000000000000, 243.4468750006145683, -6.646953231504538984 ) ) ;
#17204 = CARTESIAN_POINT ( 'NONE',  ( -48.22247103062156981, 207.6499508600178387, 3.839350919129076445 ) ) ;
#17205 = DIRECTION ( 'NONE',  ( 1.000000000000000000, 0.000000000000000000, 0.000000000000000000 ) ) ;
#17206 = CARTESIAN_POINT ( 'NONE',  ( 33.87162103762178589, 5.407089921784862696, 161.3048378204704534 ) ) ;
#17207 = CARTESIAN_POINT ( 'NONE',  ( 9.534712964251900402, 29.77731371789854364, 1.715153634034445540 ) ) ;
#17208 = CARTESIAN_POINT ( 'NONE',  ( -69.99330436395490551, 210.1155267958017134, -6.500000000000000888 ) ) ;
#17209 = DIRECTION ( 'NONE',  ( 1.000000000000000000, 0.000000000000000000, 0.000000000000000000 ) ) ;
#17210 = CARTESIAN_POINT ( 'NONE',  ( 23.54001937024031577, 195.0000000000001421, 13.61873700199885029 ) ) ;
#17211 = CARTESIAN_POINT ( 'NONE',  ( 13.62178482187501416, 196.8593750006145342, 23.59362340125806767 ) ) ;
#17212 = AXIS2_PLACEMENT_3D ( 'NONE', #26208, #31715, #25472 ) ;
#17213 = CARTESIAN_POINT ( 'NONE',  ( 15.50000000000000533, 130.6898137178985451, -0.1745138560722452326 ) ) ;
#17214 = PRODUCT_DEFINITION_FORMATION_WITH_SPECIFIED_SOURCE ( 'ANY', '', #28601, .NOT_KNOWN. ) ;
#17215 = AXIS2_PLACEMENT_3D ( 'NONE', #16047, #4651, #19645 ) ;
#17216 = VERTEX_POINT ( 'NONE', #12304 ) ;
#17217 = CARTESIAN_POINT ( 'NONE',  ( -2.660918448318275509, 38.29768628210145920, 12.46528703574805874 ) ) ;
#17218 = CYLINDRICAL_SURFACE ( 'NONE', #9878, 27.00000000000000000 ) ;
#17219 = CIRCLE ( 'NONE', #858, 2.649999999999992806 ) ;
#17220 = CARTESIAN_POINT ( 'NONE',  ( 21.27583786793474019, 5.761682509828531806, -8.000000000000005329 ) ) ;
#17221 = CARTESIAN_POINT ( 'NONE',  ( 28.32508817407707014, 5.407089921784862696, 169.5446048129269059 ) ) ;
#17222 = CARTESIAN_POINT ( 'NONE',  ( 18.00000000000000000, 5.196152422706630247, -1.368749998770957266 ) ) ;
#17223 = CARTESIAN_POINT ( 'NONE',  ( 13.44051670066911441, -5.407089921784865361, -9.121874999385520155 ) ) ;
#17224 = DIRECTION ( 'NONE',  ( 0.000000000000000000, 1.000000000000000000, 0.000000000000000000 ) ) ;
#17225 = CARTESIAN_POINT ( 'NONE',  ( -5.529263428287477744, 75.67268628210143788, 7.954856959092191815 ) ) ;
#17226 = FACE_OUTER_BOUND ( 'NONE', #12720, .T. ) ;
#17227 = CARTESIAN_POINT ( 'NONE',  ( -6.932735513423968321, 87.74768628210145494, -10.69584247140445221 ) ) ;
#17228 = CARTESIAN_POINT ( 'NONE',  ( -13.49999999999998401, 197.3750000000000284, 23.38268590217985476 ) ) ;
#17229 = CARTESIAN_POINT ( 'NONE',  ( 20.99999999999999645, 0.000000000000000000, 50.00000000000000000 ) ) ;
#17230 = ORIENTED_EDGE ( 'NONE', *, *, #8492, .T. ) ;
#17231 = CARTESIAN_POINT ( 'NONE',  ( 37.05506418370028143, -3.604726614523235284, 161.8732956221364816 ) ) ;
#17232 = CARTESIAN_POINT ( 'NONE',  ( 15.24356964375000167, -3.323476615752272600, -7.303124999385448568 ) ) ;
#17233 = CYLINDRICAL_SURFACE ( 'NONE', #16258, 5.999999999999999112 ) ;
#17234 = CARTESIAN_POINT ( 'NONE',  ( 25.14654753852813229, -3.604726614523244610, 169.0321829630285322 ) ) ;
#17235 = CARTESIAN_POINT ( 'NONE',  ( 34.26424616422337266, -5.196152422706635576, 167.1898876767739353 ) ) ;
#17236 = CARTESIAN_POINT ( 'NONE',  ( 23.87821517812500005, 240.5593750006145228, 4.985214923628404016 ) ) ;
#17237 = CARTESIAN_POINT ( 'NONE',  ( -27.24356964374999279, 198.0406250006145399, 15.72908226750539384 ) ) ;
#17238 = CARTESIAN_POINT ( 'NONE',  ( -8.962234695871565293, 127.2398137178985564, -8.715434833792128799 ) ) ;
#17239 = CARTESIAN_POINT ( 'NONE',  ( 12.53471296425194659, 118.2226862821014635, -2.311890736173178418 ) ) ;
#17241 = ORIENTED_EDGE ( 'NONE', *, *, #31285, .T. ) ;
#17240 = EDGE_LOOP ( 'NONE', ( #19261, #19317, #24451, #35782 ) ) ;
#17242 = CARTESIAN_POINT ( 'NONE',  ( -27.24356964374999990, 197.5156250006145626, -15.72908226750537786 ) ) ;
#17243 = CARTESIAN_POINT ( 'NONE',  ( 23.87821517812499650, 242.3968750006145285, -4.985214923628404904 ) ) ;
#17244 = DIRECTION ( 'NONE',  ( 0.000000000000000000, -1.000000000000000000, 0.000000000000000000 ) ) ;
#17245 = CARTESIAN_POINT ( 'NONE',  ( 8.927990412390371944, 95.32731371789854791, 13.04141134922778811 ) ) ;
#17246 = EDGE_CURVE ( 'NONE', #17383, #35216, #23551, .T. ) ;
#17247 = CARTESIAN_POINT ( 'NONE',  ( 15.24356964374999990, 3.323476615752268604, -1.190624999385493377 ) ) ;
#17248 = CARTESIAN_POINT ( 'NONE',  ( 13.50000000000001421, 196.6625000012290343, 23.38268590217984055 ) ) ;
#17249 = CARTESIAN_POINT ( 'NONE',  ( -8.710071997420207879, 79.51481371789856212, 3.796722387233182339 ) ) ;
#17250 = CARTESIAN_POINT ( 'NONE',  ( 10.31873187879411091, -3.604726614523240613, -1.903124999385531924 ) ) ;
#17251 =( BOUNDED_CURVE ( )  B_SPLINE_CURVE ( 2, ( #22492, #11106, #37244, #22680, #16619, #28526, #19841 ),
 .UNSPECIFIED., .F., .F. ) 
 B_SPLINE_CURVE_WITH_KNOTS ( ( 3, 2, 2, 3 ),
 ( 0.06521739130434593690, 0.07246376811594026912, 0.07971014492753460134, 0.08695652173912893357 ),
 .UNSPECIFIED. ) 
 CURVE ( )  GEOMETRIC_REPRESENTATION_ITEM ( )  RATIONAL_B_SPLINE_CURVE ( ( 1.000000000000034861, 0.8660254037844038466, 1.000000000000000000, 0.8660254037844387076, 1.000000000000000000, 0.8660254037844664632, 0.9999999999999722444 ) ) 
 REPRESENTATION_ITEM ( '' )  );
#17252 = EDGE_CURVE ( 'NONE', #31128, #7808, #21230, .T. ) ;
#17253 = CARTESIAN_POINT ( 'NONE',  ( 15.24356964375000167, 240.7843750006145171, 3.323476615752272600 ) ) ;
#17254 = CARTESIAN_POINT ( 'NONE',  ( 2.311890736173452865, 73.47731371789856780, -12.53471296425189152 ) ) ;
#17255 = CARTESIAN_POINT ( 'NONE',  ( 26.99999999999999289, 0.000000000000000000, -8.000000000000000000 ) ) ;
#17256 = CARTESIAN_POINT ( 'NONE',  ( -4.944772684328673229, 112.1851862821014549, 11.48171059495397728 ) ) ;
#17257 = CARTESIAN_POINT ( 'NONE',  ( 13.56230152254410548, 5.196152422706630247, -4.462499998771018994 ) ) ;
#17258 = CARTESIAN_POINT ( 'NONE',  ( -41.49330436395490551, 210.1155267958017134, -6.500000000000000888 ) ) ;
#17259 = CARTESIAN_POINT ( 'NONE',  ( 26.99999999999999645, 239.9687500012290116, -3.464101615137755275 ) ) ;
#17260 = CARTESIAN_POINT ( 'NONE',  ( 2.999999999999997335, 244.5000000000000000, -11.00000000000000000 ) ) ;
#17261 = CARTESIAN_POINT ( 'NONE',  ( 14.38691631536207538, 99.53518628210146346, -5.770363421893813793 ) ) ;
#17262 = ADVANCED_FACE ( 'NONE', ( #927, #6620 ), #12110, .T. ) ;
#17263 = CARTESIAN_POINT ( 'NONE',  ( -10.49813415415989404, 13.57268628210145422, -7.228626920339069173 ) ) ;
#17264 = DIRECTION ( 'NONE',  ( 0.9961946980917462113, 0.000000000000000000, -0.08715574274765118534 ) ) ;
#17265 = CARTESIAN_POINT ( 'NONE',  ( 23.99999999999999645, 244.5062500012290627, -5.196152422706631135 ) ) ;
#17266 = CARTESIAN_POINT ( 'NONE',  ( -6.840914352312096547, 140.3601862821014663, 6.594114490232313663 ) ) ;
#17267 = VECTOR ( 'NONE', #35348, 1000.000000000000000 ) ;
#17268 =( BOUNDED_CURVE ( )  B_SPLINE_CURVE ( 2, ( #31358, #5383, #16963, #22657, #34203, #2914, #14303 ),
 .UNSPECIFIED., .F., .F. ) 
 B_SPLINE_CURVE_WITH_KNOTS ( ( 3, 2, 2, 3 ),
 ( 0.6086956521739130821, 0.6159420289855073172, 0.6231884057971016633, 0.6304347826086960094 ),
 .UNSPECIFIED. ) 
 CURVE ( )  GEOMETRIC_REPRESENTATION_ITEM ( )  RATIONAL_B_SPLINE_CURVE ( ( 1.000000000000000000, 0.8660254037844387076, 1.000000000000000000, 0.8660254037844387076, 1.000000000000000000, 0.8660254037844326014, 1.000000000000006217 ) ) 
 REPRESENTATION_ITEM ( '' )  );
#17269 = CARTESIAN_POINT ( 'NONE',  ( -79.74198084750221938, 216.3821266856691921, 3.000000000000000000 ) ) ;
#17270 = ORIENTED_EDGE ( 'NONE', *, *, #2452, .F. ) ;
#17271 = CARTESIAN_POINT ( 'NONE',  ( 28.26462387754589045, -5.407089921784859143, 168.8534947411257576 ) ) ;
#17272 = CARTESIAN_POINT ( 'NONE',  ( -1.715153634034234598, 60.72268628210144925, -9.534712964251941258 ) ) ;
#17273 = CARTESIAN_POINT ( 'NONE',  ( 26.99999999999999645, 243.9437500012290911, 3.464101615137751278 ) ) ;
#17274 = CARTESIAN_POINT ( 'NONE',  ( 20.99999999999999645, 185.0294372515228645, 5.999999999999999112 ) ) ;
#17275 = CARTESIAN_POINT ( 'NONE',  ( 27.24356964374999635, 196.5218750006145569, -15.72908226750539029 ) ) ;
#17276 = CARTESIAN_POINT ( 'NONE',  ( 23.99999999999999645, 246.2500000000000000, -5.196152422706631135 ) ) ;
#17277 = DIRECTION ( 'NONE',  ( -0.000000000000000000, 1.000000000000000000, -0.000000000000000000 ) ) ;
#17278 = CARTESIAN_POINT ( 'NONE',  ( -3.474262827703527901, 41.56481371789855217, 8.843639120294245259 ) ) ;
#17279 = CARTESIAN_POINT ( 'NONE',  ( -27.24356964375000345, 198.5093750006145399, 0.000000000000000000 ) ) ;
#17280 = ORIENTED_EDGE ( 'NONE', *, *, #17592, .T. ) ;
#17281 = ORIENTED_EDGE ( 'NONE', *, *, #3854, .F. ) ;
#17282 = CARTESIAN_POINT ( 'NONE',  ( 18.12178482187500350, 248.4718750006145171, 4.985214923628407568 ) ) ;
#17283 = CARTESIAN_POINT ( 'NONE',  ( 0.1745138560722779009, 40.98981371789854933, 12.50000000000000355 ) ) ;
#17284 = CARTESIAN_POINT ( 'NONE',  ( 10.31873187879410736, 3.604726614523240613, -8.334374999385541827 ) ) ;
#17285 = CARTESIAN_POINT ( 'NONE',  ( 15.24356964374999990, 3.323476615752268604, -9.740624999385508076 ) ) ;
#17286 = CARTESIAN_POINT ( 'NONE',  ( -10.69584247140429412, 16.55231371789855999, -6.932735513424201024 ) ) ;
#17287 = ORIENTED_EDGE ( 'NONE', *, *, #33340, .F. ) ;
#17288 = CARTESIAN_POINT ( 'NONE',  ( 22.80587116629412492, 3.604726614523243278, -3.534374999385544669 ) ) ;
#17289 = AXIS2_PLACEMENT_3D ( 'NONE', #8371, #19569, #14059 ) ;
#17290 = CARTESIAN_POINT ( 'NONE',  ( -1.926257025242585782E-15, 199.6906250006145456, -31.45816453501075927 ) ) ;
#17291 = EDGE_CURVE ( 'NONE', #20196, #27300, #36369, .T. ) ;
#17292 = CARTESIAN_POINT ( 'NONE',  ( 28.10284103007056089, -5.407089921784865361, 167.0043083327929878 ) ) ;
#17293 = CARTESIAN_POINT ( 'NONE',  ( -36.34002896937850124, 204.4285982733020433, 3.350049139982171020 ) ) ;
#17294 = CYLINDRICAL_SURFACE ( 'NONE', #19220, 27.00000000000000355 ) ;
#17295 = CARTESIAN_POINT ( 'NONE',  ( -23.86618284116000410, 194.9999999999999147, 12.98668072022443987 ) ) ;
#17296 = EDGE_CURVE ( 'NONE', #22116, #18605, #12762, .T. ) ;
#17297 = CARTESIAN_POINT ( 'NONE',  ( -52.76711230271184405, 214.4690446883608104, -1.321298161741814914 ) ) ;
#17298 = CARTESIAN_POINT ( 'NONE',  ( -44.06622103062156981, 211.6261429550005744, 6.530955311639227823 ) ) ;
#17299 = CARTESIAN_POINT ( 'NONE',  ( 25.10569328411516921, 3.604726614523236616, 168.5652166982980305 ) ) ;
#17300 = ORIENTED_EDGE ( 'NONE', *, *, #19209, .F. ) ;
#17301 = CARTESIAN_POINT ( 'NONE',  ( 5.438367727407757144E-14, 197.7500000012290400, -27.00000000000000000 ) ) ;
#17302 = CARTESIAN_POINT ( 'NONE',  ( 22.56230152254377330, 3.464101615137958667, -1.537500000000063816 ) ) ;
#17303 = CARTESIAN_POINT ( 'NONE',  ( -8.632099005475794229, 23.45231371789854435, 13.23911966647199812 ) ) ;
#17304 = CARTESIAN_POINT ( 'NONE',  ( -63.26413769728823411, 214.1499508600179240, 7.418979330068584233 ) ) ;
#17305 =( BOUNDED_CURVE ( )  B_SPLINE_CURVE ( 2, ( #1258, #12827, #27606, #18910, #9983, #24395, #36688, #15871, #10726 ),
 .UNSPECIFIED., .F., .F. ) 
 B_SPLINE_CURVE_WITH_KNOTS ( ( 3, 2, 2, 2, 3 ),
 ( 0.6458333333333333703, 0.6527777777777777901, 0.6666666666666666297, 0.6805555555555555802, 0.6875000000000000000 ),
 .UNSPECIFIED. ) 
 CURVE ( )  GEOMETRIC_REPRESENTATION_ITEM ( )  RATIONAL_B_SPLINE_CURVE ( ( 0.9330127018922192983, 0.9330127018922198534, 1.000000000000000000, 0.8660254037844387076, 1.000000000000000000, 0.8660254037844387076, 1.000000000000000000, 0.9330127018922194093, 0.9330127018922194093 ) ) 
 REPRESENTATION_ITEM ( '' )  );
#17306 = CARTESIAN_POINT ( 'NONE',  ( -2.311890736173176641, 14.72268628210143859, -12.53471296425194836 ) ) ;
#17307 = CARTESIAN_POINT ( 'NONE',  ( 2.660918448318279950, 52.09768628210144215, -12.46528703574805697 ) ) ;
#17308 = CARTESIAN_POINT ( 'NONE',  ( 19.56230152254412502, 5.196152422706637353, -5.100000000000049383 ) ) ;
#17309 = VERTEX_POINT ( 'NONE', #6806 ) ;
#17310 = CARTESIAN_POINT ( 'NONE',  ( -39.11830436395489841, 209.8844732041982581, 6.500000000000000888 ) ) ;
#17311 = CARTESIAN_POINT ( 'NONE',  ( 27.24356964375000345, 196.4843750006145626, -3.336375036156643733E-15 ) ) ;
#17312 = CARTESIAN_POINT ( 'NONE',  ( 22.56230152254426358, -3.464101615137659351, -6.449999998771025922 ) ) ;
#17313 = CARTESIAN_POINT ( 'NONE',  ( 15.00000000000000000, 250.0000000000000000, 0.000000000000000000 ) ) ;
#17314 = CARTESIAN_POINT ( 'NONE',  ( 16.56230152254410726, 0.000000000000000000, -10.00000000000000000 ) ) ;
#17315 = DIRECTION ( 'NONE',  ( 0.9961946980917462113, 0.000000000000000000, -0.08715574274765118534 ) ) ;
#17316 = AXIS2_PLACEMENT_3D ( 'NONE', #30368, #7621, #27523 ) ;
#17317 = CARTESIAN_POINT ( 'NONE',  ( 21.00000000000000000, 246.1468750006145285, -6.646953231504538984 ) ) ;
#17318 = CARTESIAN_POINT ( 'NONE',  ( 6.840914352311949109, 95.03981371789855359, 6.594114490232462877 ) ) ;
#17319 = CARTESIAN_POINT ( 'NONE',  ( 23.87821517812499650, 240.7093750006145285, -4.985214923628404904 ) ) ;
#17320 = ORIENTED_EDGE ( 'NONE', *, *, #27448, .F. ) ;
#17321 = CARTESIAN_POINT ( 'NONE',  ( -50.79538769728821990, 211.8571965466039444, -6.469044688360768625 ) ) ;
#17322 = CARTESIAN_POINT ( 'NONE',  ( 7.234628195640309123, 197.2799038117966859, -27.00000000000000711 ) ) ;
#17323 = CARTESIAN_POINT ( 'NONE',  ( 24.00000000000000000, 247.0562500012290457, 5.196152422706629359 ) ) ;
#17324 = EDGE_LOOP ( 'NONE', ( #349, #33414, #20551, #36663 ) ) ;
#17325 = CARTESIAN_POINT ( 'NONE',  ( 2.660918448318003282, 105.1023137178985678, 12.46528703574811558 ) ) ;
#17326 = CARTESIAN_POINT ( 'NONE',  ( 10.31873187879410736, 0.000000000000000000, -1.096874999385516469 ) ) ;
#17327 = CARTESIAN_POINT ( 'NONE',  ( 36.90145218710753738, 7.646167579472015790E-16, 160.1175024667497837 ) ) ;
#17328 = CARTESIAN_POINT ( 'NONE',  ( 15.24356964374999990, 0.000000000000000000, -1.603124999385474592 ) ) ;
#17329 = CARTESIAN_POINT ( 'NONE',  ( -11.61527771782809282, 71.46481371789856496, -4.622313124798832717 ) ) ;
#17330 = CARTESIAN_POINT ( 'NONE',  ( -13.49999999999998401, 196.0250000000000057, 23.38268590217985476 ) ) ;
#17331 = ORIENTED_EDGE ( 'NONE', *, *, #11394, .F. ) ;
#17332 = ORIENTED_EDGE ( 'NONE', *, *, #19875, .T. ) ;
#17333 = ORIENTED_EDGE ( 'NONE', *, *, #4833, .F. ) ;
#17334 = CARTESIAN_POINT ( 'NONE',  ( 26.99999999999999645, 3.464101615137755275, -6.431249998770947940 ) ) ;
#17335 = CARTESIAN_POINT ( 'NONE',  ( 23.87821517812500005, -4.985214923628404016, -2.240624999385460114 ) ) ;
#17336 = CARTESIAN_POINT ( 'NONE',  ( 1.069080835302379631E-14, 196.9624999999999773, 27.00000000000000000 ) ) ;
#17337 = CARTESIAN_POINT ( 'NONE',  ( 26.75643035624999655, 246.8218750006145115, -7.049594010296217766E-16 ) ) ;
#17338 = VECTOR ( 'NONE', #23268, 1000.000000000000000 ) ;
#17339 = CARTESIAN_POINT ( 'NONE',  ( -7.228626920339069173, 48.07268628210143646, 10.49813415415989581 ) ) ;
#17340 = EDGE_CURVE ( 'NONE', #8607, #27046, #732, .T. ) ;
#17341 = CARTESIAN_POINT ( 'NONE',  ( -48.41294563604515844, 214.6737587650350747, -4.842901733360248429 ) ) ;
#17342 = CARTESIAN_POINT ( 'NONE',  ( 18.18132103106268715, 212.8186789689449654, -5.491377079880368939 ) ) ;
#17343 = CARTESIAN_POINT ( 'NONE',  ( -37.32961230271184405, 211.3212981617417938, 4.469044688360757966 ) ) ;
#17344 = PRESENTATION_STYLE_ASSIGNMENT (( #23215 ) ) ;
#17345 = CARTESIAN_POINT ( 'NONE',  ( 24.82785287066744573, -3.464101615137757051, 162.5948379930317458 ) ) ;
#17346 = CARTESIAN_POINT ( 'NONE',  ( -10.49813415416004858, 106.8273137178985479, 7.228626920338839135 ) ) ;
#17347 = CARTESIAN_POINT ( 'NONE',  ( -56.93080436395490551, 205.4999999999999716, -0.1155267958017894420 ) ) ;
#17348 = CARTESIAN_POINT ( 'NONE',  ( -41.29538769728824121, 212.3930949314662371, -8.469044688360781947 ) ) ;
#17349 = AXIS2_PLACEMENT_3D ( 'NONE', #1465, #10560, #7541 ) ;
#17350 = CARTESIAN_POINT ( 'NONE',  ( 23.87821517812499650, 4.985214923628404904, -4.903124999385472194 ) ) ;
#17351 = CARTESIAN_POINT ( 'NONE',  ( 16.56230152254411081, -6.928203230275514990, -5.287500000000021849 ) ) ;
#17352 = CARTESIAN_POINT ( 'NONE',  ( -8.632099005475794229, 78.65231371789856496, 13.23911966647199812 ) ) ;
#17353 = CARTESIAN_POINT ( 'NONE',  ( -30.40252896937849769, 206.6499508600178387, -5.571401726697954970 ) ) ;
#17354 = VERTEX_POINT ( 'NONE', #32392 ) ;
#17355 = CARTESIAN_POINT ( 'NONE',  ( 26.99999999999999645, 242.1812500012290457, -7.347880794884117764E-16 ) ) ;
#17356 = CARTESIAN_POINT ( 'NONE',  ( 7.228626920339068285, 107.8726862821014549, -10.49813415415989581 ) ) ;
#17357 = CARTESIAN_POINT ( 'NONE',  ( -3.257655550457281723, 38.29768628210144499, 15.46528703574804986 ) ) ;
#17358 = DIRECTION ( 'NONE',  ( 0.000000000000000000, 0.000000000000000000, 1.000000000000000000 ) ) ;
#17359 = CARTESIAN_POINT ( 'NONE',  ( 24.51248951003896437, 3.604726614523240613, 161.7848665344110657 ) ) ;
#17360 = CARTESIAN_POINT ( 'NONE',  ( -5.770363421893818234, 69.63518628210144357, -14.38691631536207005 ) ) ;
#17361 = CIRCLE ( 'NONE', #30073, 4.899999999999999467 ) ;
#17362 = CARTESIAN_POINT ( 'NONE',  ( -27.24356964374999279, 199.3906250006145342, 15.72908226750539384 ) ) ;
#17363 = CARTESIAN_POINT ( 'NONE',  ( 13.44051670066911619, -5.407089921784859143, -9.965624999385552130 ) ) ;
#17364 = DIRECTION ( 'NONE',  ( 0.000000000000000000, 0.000000000000000000, 1.000000000000000000 ) ) ;
#17365 = CARTESIAN_POINT ( 'NONE',  ( -51.78497103062156981, 204.4285982733020148, -3.350049139982115509 ) ) ;
#17366 = CARTESIAN_POINT ( 'NONE',  ( 1.069080835302379631E-14, 195.6124999999999829, 27.00000000000000000 ) ) ;
#17367 = CARTESIAN_POINT ( 'NONE',  ( 8.962234695871762469, 43.76018628210144357, -8.715434833791931624 ) ) ;
#17368 = CARTESIAN_POINT ( 'NONE',  ( 13.62178482187499640, 199.7093750006145285, -23.59362340125807123 ) ) ;
#17369 = CARTESIAN_POINT ( 'NONE',  ( -27.00000000000000355, 197.8250000012290570, -15.58845726811989429 ) ) ;
#17370 = CARTESIAN_POINT ( 'NONE',  ( -9.465287035748065847, 12.99768628210143362, -2.064181346179273735 ) ) ;
#17371 = LINE ( 'NONE', #13789, #28828 ) ;
#17372 = VERTEX_POINT ( 'NONE', #3589 ) ;
#17373 = CARTESIAN_POINT ( 'NONE',  ( 18.00000000000000355, -5.196152422706632912, -4.425000000000012257 ) ) ;
#17374 = CARTESIAN_POINT ( 'NONE',  ( -14.50000000000000533, 237.0000000000000000, 2.500000000000000000 ) ) ;
#17375 = CARTESIAN_POINT ( 'NONE',  ( 24.36214585379926234, -3.604726614523244610, 160.0664306802028136 ) ) ;
#17376 = CARTESIAN_POINT ( 'NONE',  ( 22.80587116629410716, 7.646167579472015790E-16, -3.515624999385541294 ) ) ;
#17377 = CARTESIAN_POINT ( 'NONE',  ( 25.22335353682449721, 3.604726614523236616, 169.9100795407218811 ) ) ;
#17378 = CARTESIAN_POINT ( 'NONE',  ( 21.00000000000000000, 241.5625000000000000, 6.928203230275506996 ) ) ;
#17379 = ADVANCED_FACE ( 'NONE', ( #15151 ), #3769, .F. ) ;
#17380 = CARTESIAN_POINT ( 'NONE',  ( -26.99999999999999645, 196.5500000012290513, 15.58845726811991561 ) ) ;
#17381 =( BOUNDED_CURVE ( )  B_SPLINE_CURVE ( 2, ( #24238, #7185, #35784, #3385, #14954, #26502, #9267 ),
 .UNSPECIFIED., .F., .F. ) 
 B_SPLINE_CURVE_WITH_KNOTS ( ( 3, 2, 2, 3 ),
 ( 0.5217391304347817060, 0.5289855072463759411, 0.5362318840579700652, 0.5434782608695641892 ),
 .UNSPECIFIED. ) 
 CURVE ( )  GEOMETRIC_REPRESENTATION_ITEM ( )  RATIONAL_B_SPLINE_CURVE ( ( 1.000000000000016431, 0.8660254037844222763, 1.000000000000000000, 0.8660254037844387076, 1.000000000000000000, 0.8660254037844571373, 0.9999999999999815703 ) ) 
 REPRESENTATION_ITEM ( '' )  );
#17382 = CARTESIAN_POINT ( 'NONE',  ( -2.311890736173176641, 69.92268628210145209, -12.53471296425194659 ) ) ;
#17383 = VERTEX_POINT ( 'NONE', #27091 ) ;
#17384 = ORIENTED_EDGE ( 'NONE', *, *, #28096, .F. ) ;
#17385 = CARTESIAN_POINT ( 'NONE',  ( 24.99999999999998934, -2.343145750507539926, 49.65004534589634488 ) ) ;
#17386 = CARTESIAN_POINT ( 'NONE',  ( -26.99999999999998934, 195.6500000012290457, 15.58845726811991561 ) ) ;
#17387 = DIRECTION ( 'NONE',  ( 0.000000000000000000, 0.000000000000000000, 1.000000000000000000 ) ) ;
#17388 = CARTESIAN_POINT ( 'NONE',  ( 23.87821517812499650, 4.985214923628404904, -5.240624999385462779 ) ) ;
#17389 = CARTESIAN_POINT ( 'NONE',  ( 15.53471296425188797, 38.97731371789853938, 2.908627838312457747 ) ) ;
#17390 = EDGE_CURVE ( 'NONE', #35535, #12708, #1116, .T. ) ;
#17391 = CYLINDRICAL_SURFACE ( 'NONE', #21231, 5.999999999999998224 ) ;
#17392 = CARTESIAN_POINT ( 'NONE',  ( 15.24356964374999990, 240.8593750006145342, 0.000000000000000000 ) ) ;
#17393 = CARTESIAN_POINT ( 'NONE',  ( -49.21205436395490551, 213.2096571498974242, 3.378800118222489601 ) ) ;
#17394 = VECTOR ( 'NONE', #5958, 999.9999999999998863 ) ;
#17395 = DIRECTION ( 'NONE',  ( -0.000000000000000000, -0.000000000000000000, 1.000000000000000000 ) ) ;
#17396 = CARTESIAN_POINT ( 'NONE',  ( 25.37366570962461054, 0.000000000000000000, 168.8335072898312887 ) ) ;
#17397 = CARTESIAN_POINT ( 'NONE',  ( -2.064181346179062349, 17.70231371789854435, -9.465287035748106703 ) ) ;
#17398 = CARTESIAN_POINT ( 'NONE',  ( -63.85788769728821279, 216.4690446883607535, 1.857196546604031662 ) ) ;
#17399 = DIRECTION ( 'NONE',  ( 1.000000000000000000, 0.000000000000000000, 0.000000000000000000 ) ) ;
#17400 = CYLINDRICAL_SURFACE ( 'NONE', #1574, 6.000000000000001776 ) ;
#17401 = CARTESIAN_POINT ( 'NONE',  ( -13.62178482187500528, 197.0843750006145285, -23.59362340125807123 ) ) ;
#17402 = CARTESIAN_POINT ( 'NONE',  ( 11.08355503943118769, 122.6398137178985479, 10.83675517735179028 ) ) ;
#17403 = ORIENTED_EDGE ( 'NONE', *, *, #37465, .F. ) ;
#17404 = CARTESIAN_POINT ( 'NONE',  ( 11.48171059495397728, 45.48518628210145209, 4.944772684328674117 ) ) ;
#17405 = CARTESIAN_POINT ( 'NONE',  ( 13.56230152254411436, -5.196152422706632912, -10.16249999877102894 ) ) ;
#17406 = CARTESIAN_POINT ( 'NONE',  ( 25.90932369323456541, 3.028670999275696829, -8.000000000000000000 ) ) ;
#17407 = CARTESIAN_POINT ( 'NONE',  ( 33.74578993402985816, -5.407089921784855591, 159.8665817251004739 ) ) ;
#17408 = CARTESIAN_POINT ( 'NONE',  ( 26.99999999999999645, 7.347880794884117764E-16, -3.318749998770964549 ) ) ;
#17409 = CARTESIAN_POINT ( 'NONE',  ( 16.56230152254411436, -7.209453229046482114, -8.634374999385517668 ) ) ;
#17410 = CARTESIAN_POINT ( 'NONE',  ( -27.00000000000000355, 196.9250000012290229, -15.58845726811989429 ) ) ;
#17411 = CARTESIAN_POINT ( 'NONE',  ( 9.465287035748067623, 81.99768628210142651, 2.064181346179272847 ) ) ;
#17412 = FACE_OUTER_BOUND ( 'NONE', #18513, .T. ) ;
#17413 = CARTESIAN_POINT ( 'NONE',  ( 0.000000000000000000, 210.0000000000000284, 0.000000000000000000 ) ) ;
#17414 = CARTESIAN_POINT ( 'NONE',  ( 4.944772684328679446, 89.18518628210145494, -11.48171059495397373 ) ) ;
#17415 = CARTESIAN_POINT ( 'NONE',  ( 26.99999999999999645, 249.7375000000000114, 3.464101615137751278 ) ) ;
#17416 = DIRECTION ( 'NONE',  ( 0.000000000000000000, 0.000000000000000000, -1.000000000000000000 ) ) ;
#17417 = ORIENTED_EDGE ( 'NONE', *, *, #33554, .F. ) ;
#17418 = CARTESIAN_POINT ( 'NONE',  ( 30.75027635825099281, -7.209453229046475009, 161.4461687411947821 ) ) ;
#17419 = CARTESIAN_POINT ( 'NONE',  ( 21.00000000000000000, -6.646953231504538984, -8.128124999385477167 ) ) ;
#17420 = CARTESIAN_POINT ( 'NONE',  ( 13.62178482187499640, 195.6593750006145456, -23.59362340125807123 ) ) ;
#17421 = CARTESIAN_POINT ( 'NONE',  ( 28.24664800560418243, 5.407089921784862696, 168.6480295846443482 ) ) ;
#17422 = CARTESIAN_POINT ( 'NONE',  ( 37.17765843037876294, -3.464101615137755275, 166.0692025214268597 ) ) ;
#17423 = CARTESIAN_POINT ( 'NONE',  ( 10.56230152254410548, 0.000000000000000000, -9.000000000000035527 ) ) ;
#17424 = CARTESIAN_POINT ( 'NONE',  ( 18.00000000000000000, 249.4749999999999943, -5.196152422706630247 ) ) ;
#17425 = CARTESIAN_POINT ( 'NONE',  ( 27.24356964375000700, 197.7406250006145285, 15.72908226750537075 ) ) ;
#17426 = CARTESIAN_POINT ( 'NONE',  ( -2.311890736173448424, 114.8773137178985735, 12.53471296425189330 ) ) ;
#17427 = CARTESIAN_POINT ( 'NONE',  ( 2.660918448318279950, 125.6976862821014578, -12.46528703574805874 ) ) ;
#17429 = VERTEX_POINT ( 'NONE', #35416 ) ;
#17428 = EDGE_LOOP ( 'NONE', ( #4360, #33315, #8221, #10746 ) ) ;
#17430 = CARTESIAN_POINT ( 'NONE',  ( 27.24356964375000345, 197.7781250006145228, -3.336375036156643733E-15 ) ) ;
#17431 = CARTESIAN_POINT ( 'NONE',  ( 18.12178482187499640, 243.3718750006145228, -4.985214923628404904 ) ) ;
#17432 = CARTESIAN_POINT ( 'NONE',  ( 8.632099005475788900, 92.45231371789854791, -13.23911966647199812 ) ) ;
#17433 = CARTESIAN_POINT ( 'NONE',  ( 21.00000000000000000, 6.646953231504538984, -3.965624999385493510 ) ) ;
#17434 = CARTESIAN_POINT ( 'NONE',  ( 23.87821517812500005, 246.8593750006145342, 4.985214923628404016 ) ) ;
#17435 = PRODUCT ( 'pusher spring', 'pusher spring', '', ( #17768 ) ) ;
#17436 = CARTESIAN_POINT ( 'NONE',  ( -27.00000000000000355, 195.6125000012290513, 0.000000000000000000 ) ) ;
#17437 = CARTESIAN_POINT ( 'NONE',  ( -1.715153634034442431, 68.87731371789855928, 9.534712964251900402 ) ) ;
#17438 = CARTESIAN_POINT ( 'NONE',  ( 16.56230152254411436, 7.209453229046475009, -3.853124999385534544 ) ) ;
#17439 = CARTESIAN_POINT ( 'NONE',  ( 20.99999999999999645, 240.8593750006145342, 6.646953231504538984 ) ) ;
#17440 = CARTESIAN_POINT ( 'NONE',  ( -6.932735513424201912, 51.05231371789854933, 10.69584247140429412 ) ) ;
#17441 = CARTESIAN_POINT ( 'NONE',  ( 30.88999790839687876, -6.928203230275506996, 163.0431933671852676 ) ) ;
#17442 = CARTESIAN_POINT ( 'NONE',  ( -7.228626920339069173, 94.07268628210145778, 10.49813415415989581 ) ) ;
#17443 = CARTESIAN_POINT ( 'NONE',  ( 13.56230152254411614, -5.196152422706632912, -4.762499998771041021 ) ) ;
#17444 = CARTESIAN_POINT ( 'NONE',  ( -34.17038769728823411, 208.1428034533959703, 6.469044688360770401 ) ) ;
#17445 = DIRECTION ( 'NONE',  ( 2.335191374515007749E-05, 0.9999999997188656620, -4.117873977262775813E-06 ) ) ;
#17446 = CARTESIAN_POINT ( 'NONE',  ( 10.49999999999999467, 222.9518338469886203, 12.50000000000000000 ) ) ;
#17447 = AXIS2_PLACEMENT_3D ( 'NONE', #19392, #30935, #33957 ) ;
#17448 = CARTESIAN_POINT ( 'NONE',  ( 13.04141134922759804, 110.1726862821014663, 8.927990412390657937 ) ) ;
#17449 = CARTESIAN_POINT ( 'NONE',  ( 11.61527771782819940, 7.535186282101452804, -4.622313124798573369 ) ) ;
#17450 = DIRECTION ( 'NONE',  ( 0.000000000000000000, 0.000000000000000000, 1.000000000000000000 ) ) ;
#17451 = CARTESIAN_POINT ( 'NONE',  ( 7.234628195640322446, 196.6450961906613770, 26.99999999999999645 ) ) ;
#17452 = CARTESIAN_POINT ( 'NONE',  ( -9.465287035748065847, 132.5976862821014493, -2.064181346179273735 ) ) ;
#17453 = EDGE_CURVE ( 'NONE', #11581, #4178, #9467, .T. ) ;
#17454 = CARTESIAN_POINT ( 'NONE',  ( 37.34761212884377812, 7.347880794884117764E-16, 168.0117821839301087 ) ) ;
#17455 = CARTESIAN_POINT ( 'NONE',  ( 26.75643035624999655, 242.7718750006145001, -7.049594010296217766E-16 ) ) ;
#17456 = ORIENTED_EDGE ( 'NONE', *, *, #5436, .F. ) ;
#17457 = CARTESIAN_POINT ( 'NONE',  ( 25.11222996482124259, -3.604726614523240613, 168.6399313006548937 ) ) ;
#17458 = CARTESIAN_POINT ( 'NONE',  ( -9.465287035748065847, 58.99768628210144783, -2.064181346179273735 ) ) ;
#17459 = CYLINDRICAL_SURFACE ( 'NONE', #7300, 4.000000000000000888 ) ;
#17460 = CARTESIAN_POINT ( 'NONE',  ( -29.00000000000002487, 210.0000000000000000, -8.000000000000000000 ) ) ;
#17461 = FACE_OUTER_BOUND ( 'NONE', #27391, .T. ) ;
#17462 = CARTESIAN_POINT ( 'NONE',  ( 13.62178482187499640, 195.2093750006145569, -23.59362340125807123 ) ) ;
#17463 = CARTESIAN_POINT ( 'NONE',  ( 33.96029051149804445, -5.196152422706629359, 163.7156586684033073 ) ) ;
#17464 = CARTESIAN_POINT ( 'NONE',  ( 37.22014685496823461, 7.347880794884125653E-16, 166.5548474367465985 ) ) ;
#17465 = CARTESIAN_POINT ( 'NONE',  ( 5.233372021372610483, 46.45231371789854791, -8.152565276336593669 ) ) ;
#17466 = CARTESIAN_POINT ( 'NONE',  ( 27.24356964375000345, 199.6343750006145399, -3.336375036156643733E-15 ) ) ;
#17467 = VECTOR ( 'NONE', #31201, 1000.000000000000000 ) ;
#17468 = EDGE_LOOP ( 'NONE', ( #27260, #8815, #18701, #35872 ) ) ;
#17469 = VERTEX_POINT ( 'NONE', #20787 ) ;
#17470 = CARTESIAN_POINT ( 'NONE',  ( 15.24356964375000167, 248.4343750006145228, 3.323476615752272600 ) ) ;
#17471 = CARTESIAN_POINT ( 'NONE',  ( 6.932735513424201024, 46.45231371789855501, -10.69584247140429412 ) ) ;
#17472 = CARTESIAN_POINT ( 'NONE',  ( 19.68408634441910721, 5.407089921784862696, -8.896874999385516958 ) ) ;
#17473 = CARTESIAN_POINT ( 'NONE',  ( 21.00000000000000000, 6.646953231504538984, -9.815624999385470062 ) ) ;
#17474 = CARTESIAN_POINT ( 'NONE',  ( 12.46528703574811558, 10.80231371789855466, -2.660918448318005503 ) ) ;
#17475 =( BOUNDED_CURVE ( )  B_SPLINE_CURVE ( 2, ( #21251, #29570, #14984, #3978, #12889, #9674, #27291 ),
 .UNSPECIFIED., .F., .F. ) 
 B_SPLINE_CURVE_WITH_KNOTS ( ( 3, 2, 2, 3 ),
 ( 0.4565217391304354777, 0.4637681159420298238, 0.4710144927536240589, 0.4782608695652184050 ),
 .UNSPECIFIED. ) 
 CURVE ( )  GEOMETRIC_REPRESENTATION_ITEM ( )  RATIONAL_B_SPLINE_CURVE ( ( 0.9999999999999866773, 0.8660254037844520303, 1.000000000000000000, 0.8660254037844387076, 1.000000000000000000, 0.8660254037844202779, 1.000000000000018430 ) ) 
 REPRESENTATION_ITEM ( '' )  );
#17476 = ADVANCED_FACE ( 'NONE', ( #28926 ), #8844, .T. ) ;
#17477 = ORIENTED_EDGE ( 'NONE', *, *, #19700, .F. ) ;
#17478 = CARTESIAN_POINT ( 'NONE',  ( 10.31873187879410736, 0.000000000000000000, -3.796874999385524418 ) ) ;
#17479 = CARTESIAN_POINT ( 'NONE',  ( -27.24356964374999990, 198.4156250006145399, -15.72908226750537786 ) ) ;
#17480 = CARTESIAN_POINT ( 'NONE',  ( 34.32918868704696536, -5.407089921784861808, 166.5348599854521296 ) ) ;
#17481 = EDGE_CURVE ( 'NONE', #9915, #17895, #26639, .T. ) ;
#17482 = CARTESIAN_POINT ( 'NONE',  ( -66.81919563604516554, 218.5000000000000000, -0.1155267958018185298 ) ) ;
#17483 = CARTESIAN_POINT ( 'NONE',  ( 18.12178482187499640, 249.6718750006145342, -4.985214923628404904 ) ) ;
#17484 = CARTESIAN_POINT ( 'NONE',  ( -25.79889966451204586, 194.9999999999999147, 8.394779565232020957 ) ) ;
#17485 = CARTESIAN_POINT ( 'NONE',  ( -57.12127896937850124, 214.5309553116392749, 1.090244570138288127 ) ) ;
#17486 = CARTESIAN_POINT ( 'NONE',  ( -35.75372103062156981, 216.5309553116391612, -1.626142955000564383 ) ) ;
#17487 = CARTESIAN_POINT ( 'NONE',  ( 37.52897353489062482, 7.646167579472015790E-16, 167.2901042930103586 ) ) ;
#17488 = ORIENTED_EDGE ( 'NONE', *, *, #1909, .T. ) ;
#17489 = CARTESIAN_POINT ( 'NONE',  ( -26.99999999999999645, 197.9000000012290457, 15.58845726811991561 ) ) ;
#17490 = CARTESIAN_POINT ( 'NONE',  ( 13.23911966647199812, 21.15231371789855430, 8.632099005475788900 ) ) ;
#17491 = CARTESIAN_POINT ( 'NONE',  ( -58.51413769728822700, 214.1499508600179240, 7.418979330068584233 ) ) ;
#17492 = CARTESIAN_POINT ( 'NONE',  ( -6.932735513423968321, 14.14768628210144463, -10.69584247140445221 ) ) ;
#17493 = CARTESIAN_POINT ( 'NONE',  ( 6.932735513423970097, 46.34768628210145636, 10.69584247140445044 ) ) ;
#17494 = CARTESIAN_POINT ( 'NONE',  ( 22.56230152254412147, -3.464101615137755275, -5.212500000000060751 ) ) ;
#17495 = VERTEX_POINT ( 'NONE', #115 ) ;
#17496 = CARTESIAN_POINT ( 'NONE',  ( -37.33705436395490551, 205.3262412349647548, -4.842901733360204908 ) ) ;
#17497 = CARTESIAN_POINT ( 'NONE',  ( 2.999999999999997335, 244.5000000000000000, 0.000000000000000000 ) ) ;
#17498 = EDGE_CURVE ( 'NONE', #21163, #29577, #21900, .T. ) ;
#17499 = CARTESIAN_POINT ( 'NONE',  ( 27.24356964375000345, 196.0343750006145456, -3.336375036156643733E-15 ) ) ;
#17500 = CARTESIAN_POINT ( 'NONE',  ( 20.99999999999999645, 0.000000000000000000, -8.000000000000000000 ) ) ;
#17501 = CARTESIAN_POINT ( 'NONE',  ( 7.234628195640322446, 195.2950961906613827, 26.99999999999999645 ) ) ;
#17502 = CARTESIAN_POINT ( 'NONE',  ( 16.56230152254410726, 0.000000000000000000, 10.00000000000000000 ) ) ;
#17503 = DIRECTION ( 'NONE',  ( 1.000000000000000000, 0.000000000000000000, 0.000000000000000000 ) ) ;
#17504 = CARTESIAN_POINT ( 'NONE',  ( 23.87821517812500005, 246.4093750006145171, 4.985214923628404016 ) ) ;
#17505 = CARTESIAN_POINT ( 'NONE',  ( -2.064181346179062349, 91.30231371789854222, -9.465287035748106703 ) ) ;
#17506 = FACE_OUTER_BOUND ( 'NONE', #31717, .T. ) ;
#17507 = ORIENTED_EDGE ( 'NONE', *, *, #24306, .F. ) ;
#17508 = CARTESIAN_POINT ( 'NONE',  ( -56.33705436395489841, 205.3262412349647263, -4.842901733360204020 ) ) ;
#17509 = CARTESIAN_POINT ( 'NONE',  ( 26.99999999999999645, 197.2250000012290343, -15.58845726811990495 ) ) ;
#17510 = CARTESIAN_POINT ( 'NONE',  ( 21.00000000000000000, 247.4687500012290684, 6.928203230275506996 ) ) ;
#17511 = ORIENTED_EDGE ( 'NONE', *, *, #27441, .T. ) ;
#17512 = CARTESIAN_POINT ( 'NONE',  ( -10.69584247140429412, 99.35231371789855359, -6.932735513424201024 ) ) ;
#17513 = EDGE_CURVE ( 'NONE', #5564, #22630, #6181, .T. ) ;
#17514 = CARTESIAN_POINT ( 'NONE',  ( 22.80587116629411781, 7.646167579472024665E-16, -0.8718749993855412495 ) ) ;
#17515 = CARTESIAN_POINT ( 'NONE',  ( 30.59339602130522096, -7.209453229046475009, 159.6530182846296384 ) ) ;
#17516 = CARTESIAN_POINT ( 'NONE',  ( 18.12178482187499640, 4.985214923628404904, -2.578124999385478233 ) ) ;
#17517 = CARTESIAN_POINT ( 'NONE',  ( -7.228626920338836470, 72.32731371789854791, -10.49813415416005213 ) ) ;
#17518 = CARTESIAN_POINT ( 'NONE',  ( -13.62178482187500528, 197.0843750006145285, -23.59362340125807123 ) ) ;
#17519 = ORIENTED_EDGE ( 'NONE', *, *, #7007, .F. ) ;
#17520 = ORIENTED_EDGE ( 'NONE', *, *, #20778, .F. ) ;
#17521 = ORIENTED_EDGE ( 'NONE', *, *, #16798, .F. ) ;
#17522 = CARTESIAN_POINT ( 'NONE',  ( 18.12178482187499640, 4.985214923628404904, -4.715624999385465088 ) ) ;
#17523 = DIRECTION ( 'NONE',  ( 1.000000000000000000, 0.000000000000000000, 0.000000000000000000 ) ) ;
#17524 = CARTESIAN_POINT ( 'NONE',  ( 26.75643035624999655, 246.4093750006145171, -3.323476615752271712 ) ) ;
#17525 = EDGE_CURVE ( 'NONE', #6022, #25349, #22126, .T. ) ;
#17526 = CARTESIAN_POINT ( 'NONE',  ( 8.962234695871762469, 34.56018628210144783, -8.715434833791931624 ) ) ;
#17527 = CARTESIAN_POINT ( 'NONE',  ( -48.80877896937850835, 211.6261429550004891, -6.530955311639245586 ) ) ;
#17528 = CARTESIAN_POINT ( 'NONE',  ( 18.90563079128943968, 210.7853884532671884, -5.961323472697883652 ) ) ;
#17529 = CARTESIAN_POINT ( 'NONE',  ( -30.60044563604516199, 206.6211998817775566, -3.209657149897419348 ) ) ;
#17530 =( BOUNDED_CURVE ( )  B_SPLINE_CURVE ( 2, ( #12651, #27424, #35197, #21384, #1081, #18162, #32737, #9433, #9621 ),
 .UNSPECIFIED., .F., .F. ) 
 B_SPLINE_CURVE_WITH_KNOTS ( ( 3, 2, 2, 2, 3 ),
 ( 0.8586956521739130821, 0.8623188405797101996, 0.8695652173913043237, 0.8768115942028985588, 0.8804347826086956763 ),
 .UNSPECIFIED. ) 
 CURVE ( )  GEOMETRIC_REPRESENTATION_ITEM ( )  RATIONAL_B_SPLINE_CURVE ( ( 0.9330127018922194093, 0.9330127018922194093, 1.000000000000000000, 0.8660254037844387076, 1.000000000000000000, 0.8660254037844387076, 1.000000000000000000, 0.9330127018922194093, 0.9330127018922194093 ) ) 
 REPRESENTATION_ITEM ( '' )  );
#17531 = CARTESIAN_POINT ( 'NONE',  ( 36.87370277765342763, -3.464101615137751278, 162.5949735130562317 ) ) ;
#17532 = CARTESIAN_POINT ( 'NONE',  ( 7.228626920338837358, 95.32731371789856212, 10.49813415416005036 ) ) ;
#17533 = CARTESIAN_POINT ( 'NONE',  ( -53.56622103062157692, 211.0902445701382533, 4.530955311639240257 ) ) ;
#17534 = CARTESIAN_POINT ( 'NONE',  ( -48.42038769728824832, 207.6069050685337913, 8.469044688360781947 ) ) ;
#17535 = EDGE_CURVE ( 'NONE', #30240, #6822, #20227, .T. ) ;
#17536 = CARTESIAN_POINT ( 'NONE',  ( 26.75643035624999655, -3.323476615752267271, -3.215624999385489957 ) ) ;
#17537 = CARTESIAN_POINT ( 'NONE',  ( 15.00000000000000000, 0.000000000000000000, -0.4500000000000059508 ) ) ;
#17538 = CARTESIAN_POINT ( 'NONE',  ( 6.092822981423662299, 77.21481371789855075, 14.25334919248795096 ) ) ;
#17539 = CARTESIAN_POINT ( 'NONE',  ( -62.06919563604516554, 218.5000000000000000, -0.1155267958018185298 ) ) ;
#17540 = ORIENTED_EDGE ( 'NONE', *, *, #21328, .T. ) ;
#17541 = CARTESIAN_POINT ( 'NONE',  ( 16.56230152254410726, 0.000000000000000000, -10.00000000000000000 ) ) ;
#17542 = CARTESIAN_POINT ( 'NONE',  ( -12.53471296425194836, 104.4226862821014379, 2.311890736173176641 ) ) ;
#17543 = CARTESIAN_POINT ( 'NONE',  ( -15.50000000000000533, 40.31018628210145494, -0.1745138560725808530 ) ) ;
#17544 = DIRECTION ( 'NONE',  ( 0.000000000000000000, 0.000000000000000000, 1.000000000000000000 ) ) ;
#17545 = CARTESIAN_POINT ( 'NONE',  ( 30.90225418466721408, -7.209453229046482114, 163.1832832459922713 ) ) ;
#17546 = CARTESIAN_POINT ( 'NONE',  ( 13.23911966647218996, 71.64768628210146062, -8.632099005475504683 ) ) ;
#17547 = CARTESIAN_POINT ( 'NONE',  ( -20.68320086892770604, 194.6619763917542798, -17.35526438333879540 ) ) ;
#17548 = EDGE_CURVE ( 'NONE', #29003, #26829, #3148, .T. ) ;
#17549 = CARTESIAN_POINT ( 'NONE',  ( 15.47812198514404258, 6.148716665048038266, -10.14010144556222315 ) ) ;
#17550 = DIRECTION ( 'NONE',  ( -0.000000000000000000, -1.000000000000000000, -0.000000000000000000 ) ) ;
#17551 = CARTESIAN_POINT ( 'NONE',  ( -48.02455436395488420, 205.1570982666397356, 4.673758765035198159 ) ) ;
#17552 = CARTESIAN_POINT ( 'NONE',  ( 10.39871248152193672, 0.5029693937725558950, -9.999999999999998224 ) ) ;
#17553 = CARTESIAN_POINT ( 'NONE',  ( 10.69584247140445221, 44.04768628210144499, -6.932735513423970097 ) ) ;
#17554 = CARTESIAN_POINT ( 'NONE',  ( 26.99999999999999645, 195.7625000000000171, -15.58845726811990495 ) ) ;
#17555 = CARTESIAN_POINT ( 'NONE',  ( 15.00000000000058620, 3.464101615138089674, -7.631249998770955223 ) ) ;
#17556 = CARTESIAN_POINT ( 'NONE',  ( 8.152565276336714462, 16.44768628210144001, -5.233372021372432847 ) ) ;
#17557 = CARTESIAN_POINT ( 'NONE',  ( 18.12178482187499640, 246.6343750006145115, -4.985214923628404904 ) ) ;
#17558 = CIRCLE ( 'NONE', #3635, 2.499999999999996891 ) ;
#17559 = ORIENTED_EDGE ( 'NONE', *, *, #28353, .T. ) ;
#17560 = CARTESIAN_POINT ( 'NONE',  ( 21.00000000000000000, -6.928203230275506996, -5.737500000000017586 ) ) ;
#17561 = CARTESIAN_POINT ( 'NONE',  ( 21.00000000000000355, 0.000000000000000000, 50.00000000000001421 ) ) ;
#17562 = CARTESIAN_POINT ( 'NONE',  ( 7.234628195640309123, 197.6174038105676516, -27.00000000000000711 ) ) ;
#17563 = CARTESIAN_POINT ( 'NONE',  ( 19.68408634441910365, 5.407089921784857367, -4.340624999385561900 ) ) ;
#17564 = CARTESIAN_POINT ( 'NONE',  ( 34.29487111334006499, -5.407089921784855591, 166.1426083230784911 ) ) ;
#17565 = CARTESIAN_POINT ( 'NONE',  ( 15.00000000000000000, 241.9000000000000057, 0.000000000000000000 ) ) ;
#17566 = CYLINDRICAL_SURFACE ( 'NONE', #313, 5.999999999999998224 ) ;
#17567 = CARTESIAN_POINT ( 'NONE',  ( 6.932735513423970097, 73.94768628210145778, 10.69584247140445044 ) ) ;
#17568 = ORIENTED_EDGE ( 'NONE', *, *, #37039, .T. ) ;
#17569 = ORIENTED_EDGE ( 'NONE', *, *, #8615, .F. ) ;
#17570 = DIRECTION ( 'NONE',  ( 0.000000000000000000, 0.000000000000000000, 1.000000000000000000 ) ) ;
#17571 = EDGE_CURVE ( 'NONE', #2674, #14431, #12052, .T. ) ;
#17572 = DIRECTION ( 'NONE',  ( 1.000000000000000000, 0.000000000000000000, 0.000000000000000000 ) ) ;
#17573 = CARTESIAN_POINT ( 'NONE',  ( -27.00000000000000355, 196.5125000012290570, 0.000000000000000000 ) ) ;
#17574 = CARTESIAN_POINT ( 'NONE',  ( 21.00000000000000000, 6.646953231504538984, -7.453124999385469351 ) ) ;
#17575 = VECTOR ( 'NONE', #22642, 1000.000000000000000 ) ;
#17576 = CARTESIAN_POINT ( 'NONE',  ( 3.257655550456945548, 31.50231371789854862, 15.46528703574811736 ) ) ;
#17577 = CARTESIAN_POINT ( 'NONE',  ( 22.60769515458673595, 249.4174038105677198, -5.999999999999999112 ) ) ;
#17578 = CARTESIAN_POINT ( 'NONE',  ( 26.75643035624999655, 240.1468750006145285, 3.323476615752267715 ) ) ;
#17579 = CARTESIAN_POINT ( 'NONE',  ( -38.32663769728823411, 206.0451222850691408, 2.149950860017832532 ) ) ;
#17580 = CARTESIAN_POINT ( 'NONE',  ( 22.56230152254410370, 7.347880794884117764E-16, -5.062499998771007981 ) ) ;
#17581 = CARTESIAN_POINT ( 'NONE',  ( 24.39482925732963281, 3.604726614523240613, 160.4400036919872150 ) ) ;
#17582 = CARTESIAN_POINT ( 'NONE',  ( 9.465287035748106703, 29.20231371789855501, -2.064181346179063237 ) ) ;
#17583 = CARTESIAN_POINT ( 'NONE',  ( -65.24330436395489130, 210.1155267958017134, -6.500000000000000888 ) ) ;
#17584 =( BOUNDED_CURVE ( )  B_SPLINE_CURVE ( 2, ( #34085, #14189, #20254, #14373, #5453, #22913, #14002 ),
 .UNSPECIFIED., .F., .F. ) 
 B_SPLINE_CURVE_WITH_KNOTS ( ( 3, 2, 2, 3 ),
 ( 0.000000000000000000, 0.007246376811594273243, 0.01449275362318854649, 0.02173913043478281973 ),
 .UNSPECIFIED. ) 
 CURVE ( )  GEOMETRIC_REPRESENTATION_ITEM ( )  RATIONAL_B_SPLINE_CURVE ( ( 1.000000000000000000, 0.8660254037844387076, 1.000000000000000000, 0.8660254037844387076, 1.000000000000000000, 0.8660254037844348218, 1.000000000000003997 ) ) 
 REPRESENTATION_ITEM ( '' )  );
#17585 = CARTESIAN_POINT ( 'NONE',  ( -38.12127896937850835, 218.5309553116392465, 2.162041339862725842 ) ) ;
#17586 = PRODUCT_CONTEXT ( 'NONE', #13203, 'mechanical' ) ;
#17587 = DIRECTION ( 'NONE',  ( -0.000000000000000000, -1.000000000000000000, -0.000000000000000000 ) ) ;
#17588 = CARTESIAN_POINT ( 'NONE',  ( 27.24356964375000345, 195.5843750006145285, -3.336375036156643733E-15 ) ) ;
#17589 = CARTESIAN_POINT ( 'NONE',  ( -14.38691631536193860, 135.8648137178985849, -5.770363421894132649 ) ) ;
#17590 = EDGE_CURVE ( 'NONE', #3817, #10799, #19699, .T. ) ;
#17591 = ORIENTED_EDGE ( 'NONE', *, *, #34228, .F. ) ;
#17592 = EDGE_CURVE ( 'NONE', #7912, #28136, #25763, .T. ) ;
#17593 = CARTESIAN_POINT ( 'NONE',  ( 7.228626920339068285, 52.67268628210144499, -10.49813415415989581 ) ) ;
#17594 = CARTESIAN_POINT ( 'NONE',  ( 20.99999999999997868, 210.0000000000000000, 5.999999999999999112 ) ) ;
#17595 = CARTESIAN_POINT ( 'NONE',  ( 23.77150201299510712, 5.059023344826917068, -8.000000000000028422 ) ) ;
#17596 = CARTESIAN_POINT ( 'NONE',  ( 28.41593846164884241, 5.957544813848095089, 159.6438083957854133 ) ) ;
#17597 = CARTESIAN_POINT ( 'NONE',  ( 18.00000000000000000, 5.196152422706630247, -2.268749998770941190 ) ) ;
#17598 = CARTESIAN_POINT ( 'NONE',  ( 10.31873187879410381, -3.604726614523244610, -7.809374999385488181 ) ) ;
#17599 = VECTOR ( 'NONE', #35738, 1000.000000000000000 ) ;
#17600 = CARTESIAN_POINT ( 'NONE',  ( -5.233372021372430183, 60.14768628210144641, -8.152565276336710909 ) ) ;
#17601 = CARTESIAN_POINT ( 'NONE',  ( 21.00000000000000000, 249.4375000000000568, -5.999999999999998224 ) ) ;
#17602 = CARTESIAN_POINT ( 'NONE',  ( 1.069080835302379631E-14, 198.4250000012290229, 27.00000000000000000 ) ) ;
#17603 = EDGE_CURVE ( 'NONE', #33644, #1610, #20601, .T. ) ;
#17604 =( BOUNDED_CURVE ( )  B_SPLINE_CURVE ( 2, ( #21996, #21808, #33361, #10421, #7397, #4730, #16305 ),
 .UNSPECIFIED., .F., .F. ) 
 B_SPLINE_CURVE_WITH_KNOTS ( ( 3, 2, 2, 3 ),
 ( 0.8478260869565201752, 0.8550724637681145213, 0.8623188405797089784, 0.8695652173913032135 ),
 .UNSPECIFIED. ) 
 CURVE ( )  GEOMETRIC_REPRESENTATION_ITEM ( )  RATIONAL_B_SPLINE_CURVE ( ( 1.000000000000028644, 0.8660254037844099528, 1.000000000000000000, 0.8660254037844387076, 1.000000000000000000, 0.8660254037844592467, 0.9999999999999794609 ) ) 
 REPRESENTATION_ITEM ( '' )  );
#17605 = CARTESIAN_POINT ( 'NONE',  ( 11.61527771782819940, 99.53518628210144925, -4.622313124798573369 ) ) ;
#17606 = CARTESIAN_POINT ( 'NONE',  ( 5.438367727407757775E-14, 198.5374999999999943, -27.00000000000000355 ) ) ;
#17607 = CARTESIAN_POINT ( 'NONE',  ( 15.00000000000000000, 0.000000000000000000, -1.349999999999990097 ) ) ;
#17608 = ORIENTED_EDGE ( 'NONE', *, *, #32700, .T. ) ;
#17609 = CARTESIAN_POINT ( 'NONE',  ( 24.67754069786733240, 0.000000000000000000, 163.6714102439223097 ) ) ;
#17610 = CARTESIAN_POINT ( 'NONE',  ( 26.75643035624999655, 3.323476615752271712, -8.428124999385486760 ) ) ;
#17611 = CARTESIAN_POINT ( 'NONE',  ( -1.926257025242585782E-15, 195.2468750006145513, -31.45816453501076637 ) ) ;
#17612 = CARTESIAN_POINT ( 'NONE',  ( 34.13308826586474254, -5.407089921784861808, 164.2934219147456929 ) ) ;
#17613 = CARTESIAN_POINT ( 'NONE',  ( 25.08932009880328096, 0.000000000000000000, 165.5834220860826349 ) ) ;
#17614 = CARTESIAN_POINT ( 'NONE',  ( 22.56230152254412147, 7.347880794884125653E-16, -9.225000000000010303 ) ) ;
#17615 = CARTESIAN_POINT ( 'NONE',  ( 24.00000000000000000, 248.3499999999999943, 5.196152422706629359 ) ) ;
#17616 = CARTESIAN_POINT ( 'NONE',  ( 13.62178482187499640, 199.2031250006145342, -23.59362340125807123 ) ) ;
#17617 = CARTESIAN_POINT ( 'NONE',  ( -8.962234695871565293, 118.0398137178985678, -8.715434833792128799 ) ) ;
#17618 = CARTESIAN_POINT ( 'NONE',  ( 7.228626920339069173, 117.0726862821014578, -10.49813415415989404 ) ) ;
#17619 = VECTOR ( 'NONE', #9839, 1000.000000000000000 ) ;
#17621 = ORIENTED_EDGE ( 'NONE', *, *, #29538, .T. ) ;
#17620 = ORIENTED_EDGE ( 'NONE', *, *, #4155, .T. ) ;
#17622 = CARTESIAN_POINT ( 'NONE',  ( -1.926257025242585782E-15, 196.9906250006145569, -31.45816453501075927 ) ) ;
#17623 = CARTESIAN_POINT ( 'NONE',  ( 15.24356964374999990, 242.0968750006145171, 0.000000000000000000 ) ) ;
#17624 = CARTESIAN_POINT ( 'NONE',  ( -5.770363421894122880, 87.56481371789857349, 14.38691631536194393 ) ) ;
#17625 = CARTESIAN_POINT ( 'NONE',  ( 18.12178482187499640, 4.985214923628404904, -5.278124999385486404 ) ) ;
#17626 = CARTESIAN_POINT ( 'NONE',  ( 21.00000000000000000, 246.5968750006145456, -6.646953231504538984 ) ) ;
#17627 = CARTESIAN_POINT ( 'NONE',  ( 27.00000000000000355, 196.2875000012290343, -3.306546357697854128E-15 ) ) ;
#17628 = CARTESIAN_POINT ( 'NONE',  ( -6.840914352311947333, 81.23981371789855643, -6.594114490232462877 ) ) ;
#17629 = CARTESIAN_POINT ( 'NONE',  ( 19.68408634441910721, 5.407089921784857367, -6.140624999385558169 ) ) ;
#17630 = CARTESIAN_POINT ( 'NONE',  ( 26.75643035624999655, 241.8343750006145285, 3.323476615752267271 ) ) ;
#17631 = CARTESIAN_POINT ( 'NONE',  ( -12.53471296425189152, 43.57731371789855501, -2.311890736173453753 ) ) ;
#17632 = FACE_OUTER_BOUND ( 'NONE', #1727, .T. ) ;
#17633 = CARTESIAN_POINT ( 'NONE',  ( 2.311890736173175753, 92.92268628210145209, 12.53471296425194836 ) ) ;
#17634 = CARTESIAN_POINT ( 'NONE',  ( 19.56230152254410370, 5.196152422706631135, -3.187499998770992882 ) ) ;
#17635 = CARTESIAN_POINT ( 'NONE',  ( -36.14955436395490551, 214.8429017333601792, -4.673758765035196383 ) ) ;
#17636 = CARTESIAN_POINT ( 'NONE',  ( 21.00000000000000355, 0.000000000000000000, 50.00000000000001421 ) ) ;
#17637 = VECTOR ( 'NONE', #1167, 1000.000000000000000 ) ;
#17638 = CARTESIAN_POINT ( 'NONE',  ( 20.99999999999995381, 241.1687500012290570, 5.999999999999998224 ) ) ;
#17639 = CARTESIAN_POINT ( 'NONE',  ( 2.908627838312118019, 92.92268628210145209, 15.53471296425195369 ) ) ;
#17640 = CARTESIAN_POINT ( 'NONE',  ( -4.622313124798576922, 14.43518628210144250, -11.61527771782819762 ) ) ;
#17641 = CARTESIAN_POINT ( 'NONE',  ( -76.95115755716804529, 229.4913094451872553, 7.500000000000000000 ) ) ;
#17642 = DIRECTION ( 'NONE',  ( 0.000000000000000000, 1.000000000000000000, 0.000000000000000000 ) ) ;
#17643 = CARTESIAN_POINT ( 'NONE',  ( 5.529263428287477744, 117.0726862821014294, -7.954856959092191815 ) ) ;
#17644 = CARTESIAN_POINT ( 'NONE',  ( 27.00000000000000355, 194.9375000012290400, -3.306546357697854128E-15 ) ) ;
#17645 = DIRECTION ( 'NONE',  ( 0.000000000000000000, 0.000000000000000000, 1.000000000000000000 ) ) ;
#17646 = CARTESIAN_POINT ( 'NONE',  ( 18.12178482187499640, 242.0218750006145001, -4.985214923628404904 ) ) ;
#17647 = EDGE_LOOP ( 'NONE', ( #31408, #27635, #30583 ) ) ;
#17648 = DIRECTION ( 'NONE',  ( 0.000000000000000000, 0.000000000000000000, -1.000000000000000000 ) ) ;
#17649 = CARTESIAN_POINT ( 'NONE',  ( 9.534712964251941258, 53.82268628210144357, -1.715153634034235708 ) ) ;
#17650 = FACE_OUTER_BOUND ( 'NONE', #15010, .T. ) ;
#17651 = DIRECTION ( 'NONE',  ( -0.000000000000000000, 1.000000000000000000, -0.000000000000000000 ) ) ;
#17652 = CARTESIAN_POINT ( 'NONE',  ( -27.24356964375000345, 194.9093750006145456, 0.000000000000000000 ) ) ;
#17653 = CARTESIAN_POINT ( 'NONE',  ( 16.56230152254411081, -6.928203230275506996, -8.774999998770997678 ) ) ;
#17654 = DIRECTION ( 'NONE',  ( -0.000000000000000000, -1.000000000000000000, -0.000000000000000000 ) ) ;
#17655 = CARTESIAN_POINT ( 'NONE',  ( 3.474262827703532341, 36.96481371789853654, -8.843639120294245259 ) ) ;
#17656 = LINE ( 'NONE', #35070, #5472 ) ;
#17657 = VERTEX_POINT ( 'NONE', #29105 ) ;
#17658 = ORIENTED_EDGE ( 'NONE', *, *, #25713, .T. ) ;
#17659 = CARTESIAN_POINT ( 'NONE',  ( 23.99999999999999645, 240.0062500012290627, -5.196152422706631135 ) ) ;
#17660 = CARTESIAN_POINT ( 'NONE',  ( -7.228626920338836470, 35.52731371789855075, -10.49813415416005213 ) ) ;
#17661 = CARTESIAN_POINT ( 'NONE',  ( 10.31873187879410558, -3.604726614523244610, -9.159374999385507365 ) ) ;
#17662 = CARTESIAN_POINT ( 'NONE',  ( 15.24356964374999990, 3.323476615752268604, -8.390624999385488891 ) ) ;
#17663 = CARTESIAN_POINT ( 'NONE',  ( -12.46528703574811558, 15.40231371789854542, 2.660918448318003726 ) ) ;
#17664 = CARTESIAN_POINT ( 'NONE',  ( 26.99999999999999645, 247.9749999999999943, -7.347880794884117764E-16 ) ) ;
#17665 = ORIENTED_EDGE ( 'NONE', *, *, #17590, .F. ) ;
#17666 = CARTESIAN_POINT ( 'NONE',  ( 10.31873187879410381, -3.604726614523244610, -4.209374999385490312 ) ) ;
#17667 = ORIENTED_EDGE ( 'NONE', *, *, #18504, .T. ) ;
#17668 = CARTESIAN_POINT ( 'NONE',  ( 27.24356964375000345, 199.1281250006145171, -3.336375036156643733E-15 ) ) ;
#17669 = CARTESIAN_POINT ( 'NONE',  ( 37.40314243129871841, -3.604726614523238837, 165.8518481976404360 ) ) ;
#17670 = CARTESIAN_POINT ( 'NONE',  ( -67.61086230271183695, 214.1499508600178387, -7.418979330068641964 ) ) ;
#17671 = CARTESIAN_POINT ( 'NONE',  ( 26.75643035624999655, 248.6593750006145171, -3.323476615752271268 ) ) ;
#17672 = PLANE ( 'NONE',  #20050 ) ;
#17673 = CARTESIAN_POINT ( 'NONE',  ( -52.37127896937850835, 214.5309553116392749, 1.090244570138288127 ) ) ;
#17674 = CARTESIAN_POINT ( 'NONE',  ( -32.38913769728823411, 206.8500491399821044, -5.686928522499717253 ) ) ;
#17675 = CARTESIAN_POINT ( 'NONE',  ( 25.22662187717753568, 0.000000000000000000, 169.9474368419002985 ) ) ;
#17676 = VERTEX_POINT ( 'NONE', #5803 ) ;
#17677 = CARTESIAN_POINT ( 'NONE',  ( 21.00000000000000000, 241.6187500012290457, 5.999999999999998224 ) ) ;
#17678 = CARTESIAN_POINT ( 'NONE',  ( 13.04141134922778988, 28.62731371789854506, -8.927990412390371944 ) ) ;
#17679 = CARTESIAN_POINT ( 'NONE',  ( -55.14955436395491262, 216.3070033484980002, -6.137860380172975638 ) ) ;
#17680 = VECTOR ( 'NONE', #30698, 1000.000000000000000 ) ;
#17681 = CARTESIAN_POINT ( 'NONE',  ( 9.465287035748067623, 137.1976862821014436, 2.064181346179272847 ) ) ;
#17682 = CARTESIAN_POINT ( 'NONE',  ( -10.49813415415989581, 41.17268628210144499, -7.228626920339068285 ) ) ;
#17683 = CARTESIAN_POINT ( 'NONE',  ( 22.56230152254412147, 7.347880794884125653E-16, -4.275000000000028777 ) ) ;
#17684 = EDGE_LOOP ( 'NONE', ( #37031, #13275, #27813, #14023 ) ) ;
#17685 = CARTESIAN_POINT ( 'NONE',  ( -49.01413769728823411, 213.1499508600178672, 5.686928522499718142 ) ) ;
#17686 = CARTESIAN_POINT ( 'NONE',  ( 19.39230484541326049, 242.2575961894323200, -5.999999999999997335 ) ) ;
#17687 = CARTESIAN_POINT ( 'NONE',  ( 6.840914352312096547, 16.16018628210144570, -6.594114490232313663 ) ) ;
#17688 = CARTESIAN_POINT ( 'NONE',  ( -27.24356964374999990, 195.7718750006145569, -15.72908226750537786 ) ) ;
#17689 = CARTESIAN_POINT ( 'NONE',  ( 26.99999999999999645, 198.1250000012290400, -15.58845726811990495 ) ) ;
#17690 = CARTESIAN_POINT ( 'NONE',  ( -13.50000000000000533, 198.5749999999999886, -23.38268590217984411 ) ) ;
#17691 = CARTESIAN_POINT ( 'NONE',  ( 25.25600545691528254, 0.000000000000000000, 167.4886444474074381 ) ) ;
#17692 = CARTESIAN_POINT ( 'NONE',  ( 28.32956640036948315, -5.196152422706632912, 168.1984670498039236 ) ) ;
#17693 = CARTESIAN_POINT ( 'NONE',  ( 15.24356964374999990, 246.2218750006145456, -3.323476615752268604 ) ) ;
#17694 = CARTESIAN_POINT ( 'NONE',  ( -9.500000000000005329, 98.48981371789855643, 0.1745138560723101806 ) ) ;
#17695 = VERTEX_POINT ( 'NONE', #2961 ) ;
#17696 = CARTESIAN_POINT ( 'NONE',  ( -53.36830436395489841, 209.8844732041982581, 6.500000000000000888 ) ) ;
#17697 = CARTESIAN_POINT ( 'NONE',  ( 15.00000000000000000, 247.3562500012290570, 0.000000000000000000 ) ) ;
#17698 = CARTESIAN_POINT ( 'NONE',  ( 12.50000000000000355, 93.88981371789856212, -0.1745138560722771515 ) ) ;
#17699 = CARTESIAN_POINT ( 'NONE',  ( 19.68408634441912142, -5.407089921784861808, -2.296874999385551064 ) ) ;
#17700 = CARTESIAN_POINT ( 'NONE',  ( 7.234628195640337545, 198.1799038117967200, -26.99999999999999289 ) ) ;
#17701 = CARTESIAN_POINT ( 'NONE',  ( 21.00000000000000000, 6.646953231504538984, -2.165624999385510563 ) ) ;
#17702 = CARTESIAN_POINT ( 'NONE',  ( 12.46528703574811558, 75.20231371789856212, -2.660918448318005503 ) ) ;
#17703 = CARTESIAN_POINT ( 'NONE',  ( -27.24356964374999635, 198.5468750006145626, 15.72908226750539384 ) ) ;
#17704 = ORIENTED_EDGE ( 'NONE', *, *, #7983, .F. ) ;
#17705 = ORIENTED_EDGE ( 'NONE', *, *, #175, .T. ) ;
#17706 = CARTESIAN_POINT ( 'NONE',  ( 26.75643035624999655, 3.323476615752271268, -6.178124999385475213 ) ) ;
#17707 = CARTESIAN_POINT ( 'NONE',  ( -56.70466238434235606, 244.2363183625454894, 7.500000000000000000 ) ) ;
#17708 = CARTESIAN_POINT ( 'NONE',  ( 23.87821517812500005, 247.1968750006145115, 4.985214923628404016 ) ) ;
#17709 = CARTESIAN_POINT ( 'NONE',  ( -12.50000000000000355, 31.11018628210143788, -0.1745138560725492671 ) ) ;
#17710 = ADVANCED_FACE ( 'NONE', ( #34800, #20416 ), #31959, .F. ) ;
#17711 = CARTESIAN_POINT ( 'NONE',  ( -49.99627896937850124, 203.4690446883607535, -1.626142955000504209 ) ) ;
#17712 = LINE ( 'NONE', #20377, #2669 ) ;
#17713 = CARTESIAN_POINT ( 'NONE',  ( -32.97544563604516554, 213.3788001182224718, 3.209657149897419348 ) ) ;
#17714 = SHAPE_REPRESENTATION_RELATIONSHIP ( 'NONE' , 'NONE' ,  #8404, #35907 ) ;
#17715 = CARTESIAN_POINT ( 'NONE',  ( 33.84263025878871645, -5.196152422706629359, 162.3707958259794566 ) ) ;
#17716 = CARTESIAN_POINT ( 'NONE',  ( -6.932735513424201912, 106.2523137178985735, 10.69584247140429412 ) ) ;
#17717 = CARTESIAN_POINT ( 'NONE',  ( -63.46205436395489841, 213.2096571498974242, 3.378800118222489601 ) ) ;
#17718 = CARTESIAN_POINT ( 'NONE',  ( -68.40997103062156270, 215.5714017266979852, 3.350049139982118618 ) ) ;
#17719 = CARTESIAN_POINT ( 'NONE',  ( 20.99999999999999645, -6.646953231504538984, -4.190624999385508254 ) ) ;
#17720 = FACE_OUTER_BOUND ( 'NONE', #27952, .T. ) ;
#17721 = CARTESIAN_POINT ( 'NONE',  ( -3.257655550456946880, 72.90231371789855075, -15.46528703574811736 ) ) ;
#17722 = CARTESIAN_POINT ( 'NONE',  ( -59.69419563604517265, 201.5000000000000000, 0.1155267958018195706 ) ) ;
#17723 = ORIENTED_EDGE ( 'NONE', *, *, #27451, .F. ) ;
#17724 = CARTESIAN_POINT ( 'NONE',  ( 14.47852626837769563, 5.725135026351853007, -9.986452809322953428 ) ) ;
#17725 = CARTESIAN_POINT ( 'NONE',  ( 11.61527771782819940, 108.7351862821014663, -4.622313124798573369 ) ) ;
#17726 = CARTESIAN_POINT ( 'NONE',  ( 15.46528703574804986, 54.39768628210144641, 3.257655550457285720 ) ) ;
#17727 = PLANE ( 'NONE',  #2306 ) ;
#17728 = CARTESIAN_POINT ( 'NONE',  ( 36.85406125198851157, -3.604726614523238837, 159.5758215996624187 ) ) ;
#17729 = CARTESIAN_POINT ( 'NONE',  ( -10.83675517735155047, 69.06018628210144072, -11.08355503943142750 ) ) ;
#17730 = CARTESIAN_POINT ( 'NONE',  ( 13.62178482187501416, 199.5031250006145456, 23.59362340125806767 ) ) ;
#17731 = EDGE_CURVE ( 'NONE', #7355, #23955, #29633, .T. ) ;
#17732 = CARTESIAN_POINT ( 'NONE',  ( 22.80587116629410716, 7.646167579472015790E-16, -8.465624999385523708 ) ) ;
#17733 = DIRECTION ( 'NONE',  ( 0.000000000000000000, 0.000000000000000000, 1.000000000000000000 ) ) ;
#17734 = CARTESIAN_POINT ( 'NONE',  ( -43.86830436395490551, 209.8844732041982581, 6.500000000000000888 ) ) ;
#17735 = AXIS2_PLACEMENT_3D ( 'NONE', #21606, #21979, #24805 ) ;
#17736 = CARTESIAN_POINT ( 'NONE',  ( 0.000000000000000000, 200.0000000000000000, 0.000000000000000000 ) ) ;
#17737 = CARTESIAN_POINT ( 'NONE',  ( 12.46528703574805874, 35.99768628210144072, 2.660918448318279950 ) ) ;
#17738 = CARTESIAN_POINT ( 'NONE',  ( 27.00000000000001066, 196.5875000000000341, 15.58845726811988897 ) ) ;
#17739 = CARTESIAN_POINT ( 'NONE',  ( 18.91622499444735439, 240.0135471875693725, -5.725135169889072451 ) ) ;
#17740 = CARTESIAN_POINT ( 'NONE',  ( 8.843639120294328748, 7.535186282101451916, -3.474262827703334722 ) ) ;
#17741 = CARTESIAN_POINT ( 'NONE',  ( 23.87821517812499650, 247.0093750006145399, -4.985214923628404904 ) ) ;
#17742 = ORIENTED_EDGE ( 'NONE', *, *, #9927, .T. ) ;
#17743 = CARTESIAN_POINT ( 'NONE',  ( 24.00000000000000000, -5.196152422706629359, -7.950000000000012612 ) ) ;
#17744 = PRODUCT_DEFINITION_SHAPE ( 'NONE', 'NONE',  #15289 ) ;
#17745 = CARTESIAN_POINT ( 'NONE',  ( 20.99999999999999645, 0.000000000000000000, -8.000000000000000000 ) ) ;
#17746 = CARTESIAN_POINT ( 'NONE',  ( 22.80587116629410360, -3.604726614523235284, -4.003124999385554439 ) ) ;
#17747 = CARTESIAN_POINT ( 'NONE',  ( 31.26013745332475224, -7.209453229046475009, 167.2739077250314779 ) ) ;
#17748 = CARTESIAN_POINT ( 'NONE',  ( 15.00000000000000000, 241.0000000000000000, 0.000000000000000000 ) ) ;
#17749 = CARTESIAN_POINT ( 'NONE',  ( 27.00000000000000355, 199.7750000000000057, -3.306546357697854128E-15 ) ) ;
#17750 = CARTESIAN_POINT ( 'NONE',  ( 4.622313124798573369, 74.23518628210145209, 11.61527771782819940 ) ) ;
#17751 = ORIENTED_EDGE ( 'NONE', *, *, #3391, .F. ) ;
#17752 = ORIENTED_EDGE ( 'NONE', *, *, #16103, .F. ) ;
#17753 = CARTESIAN_POINT ( 'NONE',  ( 26.97716818855048260, 0.000000000000000000, 49.47706554351410801 ) ) ;
#17754 = CARTESIAN_POINT ( 'NONE',  ( 27.58438479987706415, -5.196152422706632912, 159.6810023811194981 ) ) ;
#17756 = CARTESIAN_POINT ( 'NONE',  ( 7.234628195640363302, 195.3674038105676800, -26.99999999999996803 ) ) ;
#17755 =( GEOMETRIC_REPRESENTATION_CONTEXT ( 3 ) GLOBAL_UNCERTAINTY_ASSIGNED_CONTEXT ( ( #36618 ) ) GLOBAL_UNIT_ASSIGNED_CONTEXT ( ( #6136, #34764, #5574 ) ) REPRESENTATION_CONTEXT ( 'NONE', 'WORKASPACE' ) );
#17757 = CARTESIAN_POINT ( 'NONE',  ( 21.00000000000000000, -6.646953231504538984, -5.428124999385471661 ) ) ;
#17758 = CARTESIAN_POINT ( 'NONE',  ( 10.69584247140445221, 90.04768628210145209, -6.932735513423970097 ) ) ;
#17759 = CARTESIAN_POINT ( 'NONE',  ( 8.632099005475788900, 28.05231371789855643, -13.23911966647199812 ) ) ;
#17760 = LINE ( 'NONE', #2781, #6074 ) ;
#17761 = CARTESIAN_POINT ( 'NONE',  ( 26.75643035624999655, 240.1843750006145513, -7.049594010296217766E-16 ) ) ;
#17762 = CARTESIAN_POINT ( 'NONE',  ( -36.94122103062156981, 208.9097554298617752, -4.530955311639240257 ) ) ;
#17763 = CARTESIAN_POINT ( 'NONE',  ( 26.99999999999983658, 3.464101615137847645, -6.431249998770946164 ) ) ;
#17764 = CARTESIAN_POINT ( 'NONE',  ( 36.81810950810510974, 7.646167579472024665E-16, 159.1648912866995715 ) ) ;
#17765 = CARTESIAN_POINT ( 'NONE',  ( -0.1745138560723084320, 17.98981371789853867, -9.500000000000005329 ) ) ;
#17766 = CARTESIAN_POINT ( 'NONE',  ( -54.55580436395489841, 216.5000000000000000, 0.1155267958017343610 ) ) ;
#17767 = CARTESIAN_POINT ( 'NONE',  ( -32.97544563604516554, 216.3070033484980854, 6.137860380172893926 ) ) ;
#17768 = PRODUCT_CONTEXT ( 'NONE', #35935, 'mechanical' ) ;
#17769 = CARTESIAN_POINT ( 'NONE',  ( 26.81003669216458718, 195.0000000000000000, 4.277059241843740978 ) ) ;
#17770 = CARTESIAN_POINT ( 'NONE',  ( -13.62178482187498396, 195.4343750006145228, 23.59362340125808188 ) ) ;
#17771 = CARTESIAN_POINT ( 'NONE',  ( -8.927990412390371944, 136.7273137178985110, -13.04141134922778988 ) ) ;
#17772 = CARTESIAN_POINT ( 'NONE',  ( -53.36086230271183695, 213.1499508600178387, -5.686928522499747451 ) ) ;
#17773 = VERTEX_POINT ( 'NONE', #30053 ) ;
#17774 = CARTESIAN_POINT ( 'NONE',  ( -4.944772684328673229, 47.78518628210144925, 11.48171059495397728 ) ) ;
#17775 = CARTESIAN_POINT ( 'NONE',  ( -4.500000000000001776, 227.8255434699758837, -2.500000000000000000 ) ) ;
#17776 = CARTESIAN_POINT ( 'NONE',  ( 7.234628195640322446, 198.7825961894323257, 26.99999999999999645 ) ) ;
#17777 = CARTESIAN_POINT ( 'NONE',  ( 31.15718473220409379, 7.209453229046482114, 166.0971527379105908 ) ) ;
#17778 = CARTESIAN_POINT ( 'NONE',  ( 26.99999999999999645, -3.464101615137751278, -2.906249998770944032 ) ) ;
#17779 = EDGE_LOOP ( 'NONE', ( #6700, #15970, #12331, #4138 ) ) ;
#17780 = CARTESIAN_POINT ( 'NONE',  ( -63.46205436395489841, 214.6737587650351884, 4.842901733360205796 ) ) ;
#17781 = CARTESIAN_POINT ( 'NONE',  ( 19.68408634441910365, 5.407089921784857367, -2.990624999385543603 ) ) ;
#17782 = CARTESIAN_POINT ( 'NONE',  ( 6.594114490232313663, 55.26018628210144357, 6.840914352312096547 ) ) ;
#17783 = CARTESIAN_POINT ( 'NONE',  ( 16.56230152254410726, 0.000000000000000000, 10.00000000000000000 ) ) ;
#17784 = CARTESIAN_POINT ( 'NONE',  ( 23.99999999999999645, 245.7999999999999829, -5.196152422706631135 ) ) ;
#17785 = AXIS2_PLACEMENT_3D ( 'NONE', #17229, #35388, #31800 ) ;
#17786 = CARTESIAN_POINT ( 'NONE',  ( 8.962234695871762469, 98.96018628210146062, -8.715434833791931624 ) ) ;
#17787 = CARTESIAN_POINT ( 'NONE',  ( 36.63511393177383013, 3.464101615138219348, 159.8678905258058194 ) ) ;
#17788 = CARTESIAN_POINT ( 'NONE',  ( -27.00000000000000355, 195.0500000000000114, 0.000000000000000000 ) ) ;
#17789 = ORIENTED_EDGE ( 'NONE', *, *, #28427, .T. ) ;
#17790 = CARTESIAN_POINT ( 'NONE',  ( -20.86978606573367045, 194.8588513912095266, -17.51182790300216752 ) ) ;
#17791 = CARTESIAN_POINT ( 'NONE',  ( 15.00000000000000000, 3.464101615137752166, -0.03749999999999697325 ) ) ;
#17792 = CARTESIAN_POINT ( 'NONE',  ( 34.19887935716262461, 5.196152422706637353, 166.4427416532051609 ) ) ;
#17793 = CARTESIAN_POINT ( 'NONE',  ( 37.40641077165175687, 7.646167579472024665E-16, 165.8892054988188534 ) ) ;
#17794 = CARTESIAN_POINT ( 'NONE',  ( 36.90638618107669799, 7.347880794884125653E-16, 162.9685465236163111 ) ) ;
#17795 = CARTESIAN_POINT ( 'NONE',  ( 1.120210788295102201E-13, 196.7375000000000398, -27.00000000000000711 ) ) ;
#17796 = CARTESIAN_POINT ( 'NONE',  ( 18.00000000000000000, 248.5749999999999886, -5.196152422706630247 ) ) ;
#17797 = CARTESIAN_POINT ( 'NONE',  ( 27.24356964375000700, 195.0406250006145399, 15.72908226750537075 ) ) ;
#17798 = CARTESIAN_POINT ( 'NONE',  ( 12.46528703574811558, 112.0023137178985735, -2.660918448318005503 ) ) ;
#17799 =( REPRESENTATION_RELATIONSHIP ('NONE','NONE', #4304, #10397 ) REPRESENTATION_RELATIONSHIP_WITH_TRANSFORMATION ( #19833 )SHAPE_REPRESENTATION_RELATIONSHIP( ) );
#17800 = CARTESIAN_POINT ( 'NONE',  ( 12.46528703574805874, 118.7976862821014663, 2.660918448318279950 ) ) ;
#17802 = VERTEX_POINT ( 'NONE', #7313 ) ;
#17801 = ORIENTED_EDGE ( 'NONE', *, *, #15976, .F. ) ;
#17803 = CARTESIAN_POINT ( 'NONE',  ( -27.24356964374999635, 195.3406250006145513, 15.72908226750539384 ) ) ;
#17804 = CARTESIAN_POINT ( 'NONE',  ( 23.87821517812499650, 241.4968750006144944, -4.985214923628404904 ) ) ;
#17805 = CARTESIAN_POINT ( 'NONE',  ( 14.38691631536194393, 94.46481371789855075, 5.770363421894124656 ) ) ;
#17806 =( BOUNDED_CURVE ( )  B_SPLINE_CURVE ( 2, ( #15351, #9846, #26905, #32778, #15540, #7017, #14788 ),
 .UNSPECIFIED., .F., .F. ) 
 B_SPLINE_CURVE_WITH_KNOTS ( ( 3, 2, 2, 3 ),
 ( 0.2608695652173921298, 0.2681159420289864204, 0.2753623188405806554, 0.2826086956521748905 ),
 .UNSPECIFIED. ) 
 CURVE ( )  GEOMETRIC_REPRESENTATION_ITEM ( )  RATIONAL_B_SPLINE_CURVE ( ( 0.9999999999999845679, 0.8660254037844541397, 1.000000000000000000, 0.8660254037844387076, 1.000000000000000000, 0.8660254037844202779, 1.000000000000018430 ) ) 
 REPRESENTATION_ITEM ( '' )  );
#17807 = CARTESIAN_POINT ( 'NONE',  ( 26.75643035624999655, -3.323476615752267715, -4.115624999385481431 ) ) ;
#17808 = CARTESIAN_POINT ( 'NONE',  ( 26.75643035624999655, 248.7343750006145342, -7.049594010296217766E-16 ) ) ;
#17809 = CARTESIAN_POINT ( 'NONE',  ( -8.710071997420127943, 105.2851862821014777, -3.796722387233380402 ) ) ;
#17810 = CIRCLE ( 'NONE', #13558, 10.00000000000000888 ) ;
#17811 = AXIS2_PLACEMENT_3D ( 'NONE', #500, #9229, #130 ) ;
#17812 = CARTESIAN_POINT ( 'NONE',  ( 13.49999999999999645, 195.4625000012290172, -23.38268590217984766 ) ) ;
#17813 = ADVANCED_FACE ( 'NONE', ( #21165 ), #24001, .F. ) ;
#17814 = CARTESIAN_POINT ( 'NONE',  ( 1.715153634034445762, 73.47731371789855359, -9.534712964251895073 ) ) ;
#17815 = VECTOR ( 'NONE', #30247, 1000.000000000000000 ) ;
#17816 = CARTESIAN_POINT ( 'NONE',  ( 13.44051670066911086, 5.407089921784856479, -6.515624999385543958 ) ) ;
#17817 = COLOUR_RGB ( '',0.8941176470588234615, 0.8941176470588234615, 0.8941176470588234615 ) ;
#17818 = EDGE_CURVE ( 'NONE', #17469, #26583, #27210, .T. ) ;
#17819 = CARTESIAN_POINT ( 'NONE',  ( 15.24356964375000167, 241.6843750006145513, 3.323476615752272600 ) ) ;
#17820 = CARTESIAN_POINT ( 'NONE',  ( -12.50000000000000355, 43.28981371789855359, 0.1745138560722786503 ) ) ;
#17821 = CARTESIAN_POINT ( 'NONE',  ( 1.120210788295102201E-13, 197.1875000000000568, -27.00000000000000711 ) ) ;
#17822 = CARTESIAN_POINT ( 'NONE',  ( 12.53471296425194836, 109.0226862821014606, -2.311890736173178418 ) ) ;
#17823 = CARTESIAN_POINT ( 'NONE',  ( 19.56230152254410726, 5.196152422706631135, -5.887499998771001053 ) ) ;
#17824 = EDGE_CURVE ( 'NONE', #3383, #29774, #7616, .T. ) ;
#17825 =( BOUNDED_CURVE ( )  B_SPLINE_CURVE ( 2, ( #18924, #35767, #13226, #29902, #9811, #32930, #27622, #21761, #10184 ),
 .UNSPECIFIED., .F., .F. ) 
 B_SPLINE_CURVE_WITH_KNOTS ( ( 3, 2, 2, 2, 3 ),
 ( 0.1041666666666666713, 0.1111111111111111049, 0.1250000000000000000, 0.1388888888888888951, 0.1458333333333333426 ),
 .UNSPECIFIED. ) 
 CURVE ( )  GEOMETRIC_REPRESENTATION_ITEM ( )  RATIONAL_B_SPLINE_CURVE ( ( 0.9330127018922194093, 0.9330127018922194093, 1.000000000000000000, 0.8660254037844387076, 1.000000000000000000, 0.8660254037844387076, 1.000000000000000000, 0.9330127018922194093, 0.9330127018922194093 ) ) 
 REPRESENTATION_ITEM ( '' )  );
#17826 = CARTESIAN_POINT ( 'NONE',  ( -63.06622103062156270, 211.0902445701382533, 4.530955311639240257 ) ) ;
#17827 = CARTESIAN_POINT ( 'NONE',  ( 10.69584247140445221, 136.0476862821014379, -6.932735513423970097 ) ) ;
#17828 = CARTESIAN_POINT ( 'NONE',  ( 19.39230484541323918, 240.9638461906613998, -5.999999999999987566 ) ) ;
#17829 = CARTESIAN_POINT ( 'NONE',  ( 13.23911966647218996, 80.84768628210143504, -8.632099005475504683 ) ) ;
#17830 = CARTESIAN_POINT ( 'NONE',  ( 26.99999999999958078, -3.464101615137992862, -0.7125000000000120126 ) ) ;
#17831 = LINE ( 'NONE', #3259, #6115 ) ;
#17832 = CARTESIAN_POINT ( 'NONE',  ( 1.069080835302379631E-14, 199.2125000000000057, 27.00000000000000000 ) ) ;
#17833 = CARTESIAN_POINT ( 'NONE',  ( 3.796722387233379514, 107.5851862821014748, -8.710071997420127943 ) ) ;
#17834 = CARTESIAN_POINT ( 'NONE',  ( 15.00000000000000000, 247.7687500012291082, -3.464101615137752610 ) ) ;
#17835 = CARTESIAN_POINT ( 'NONE',  ( 15.53471296425195369, 17.02268628210144996, -2.908627838312120684 ) ) ;
#17836 = CARTESIAN_POINT ( 'NONE',  ( -27.24356964375000345, 195.8093750006145513, 0.000000000000000000 ) ) ;
#17837 = CARTESIAN_POINT ( 'NONE',  ( 23.87821517812500005, 241.3468750006145171, 4.985214923628404016 ) ) ;
#17838 = EDGE_LOOP ( 'NONE', ( #12911, #6967, #22932, #5351, #27310, #15646, #17116, #18398, #4478, #25665, #15783, #4599, #10322, #27867, #28492, #27261, #32787, #8884, #12886, #2496, #3662, #34384, #16726, #26500, #26359 ) ) ;
#17839 = CARTESIAN_POINT ( 'NONE',  ( 24.90959286293295705, 3.604726614523236616, 166.3237786275915937 ) ) ;
#17840 = AXIS2_PLACEMENT_3D ( 'NONE', #2390, #16630, #2202 ) ;
#17841 = CARTESIAN_POINT ( 'NONE',  ( 21.00000000000000000, 6.646953231504538984, -1.603124999385459937 ) ) ;
#17842 = DIRECTION ( 'NONE',  ( 1.000000000000000000, 0.000000000000000000, 0.000000000000000000 ) ) ;
#17843 = FACE_OUTER_BOUND ( 'NONE', #30000, .T. ) ;
#17844 = FACE_BOUND ( 'NONE', #6577, .T. ) ;
#17845 = CARTESIAN_POINT ( 'NONE',  ( 13.44051670066911441, 5.407089921784856479, -0.6656249993855500868 ) ) ;
#17846 = CARTESIAN_POINT ( 'NONE',  ( 8.843639120294245259, 11.66481371789854293, 3.474262827703527901 ) ) ;
#17847 = CARTESIAN_POINT ( 'NONE',  ( 13.62178482187499640, 199.2593750006145399, -23.59362340125807123 ) ) ;
#17848 = VERTEX_POINT ( 'NONE', #9405 ) ;
#17849 = CARTESIAN_POINT ( 'NONE',  ( 15.00000000000000178, 239.7437500012290457, 3.464101615137757051 ) ) ;
#17850 = CARTESIAN_POINT ( 'NONE',  ( -6.932735513424201912, 51.05231371789854933, 10.69584247140429412 ) ) ;
#17851 = CARTESIAN_POINT ( 'NONE',  ( 18.12178482187500350, -4.985214923628407568, -9.628124999385478944 ) ) ;
#17852 = CARTESIAN_POINT ( 'NONE',  ( 12.46528703574811558, 20.00231371789855217, -2.660918448318005503 ) ) ;
#17853 = CARTESIAN_POINT ( 'NONE',  ( 37.37702719191401002, 7.347880794884125653E-16, 168.3479978933117422 ) ) ;
#17854 = ORIENTED_EDGE ( 'NONE', *, *, #36911, .F. ) ;
#17855 = CARTESIAN_POINT ( 'NONE',  ( 16.56230152254411436, -7.209453229046482114, -3.234374999385536409 ) ) ;
#17856 = CARTESIAN_POINT ( 'NONE',  ( 5.778771075727756162E-15, 199.0156250006145342, 31.45816453501075927 ) ) ;
#17857 = CARTESIAN_POINT ( 'NONE',  ( 31.13757469008587719, -7.209453229046482114, 165.8730089308399442 ) ) ;
#17858 = ADVANCED_FACE ( 'NONE', ( #35730 ), #32893, .T. ) ;
#17859 = CARTESIAN_POINT ( 'NONE',  ( -32.57961230271183695, 211.8571965466040297, 6.469044688360755302 ) ) ;
#17860 = CARTESIAN_POINT ( 'NONE',  ( 26.75643035624999655, 249.0343750006144887, 3.323476615752267271 ) ) ;
#17861 = CARTESIAN_POINT ( 'NONE',  ( -15.87381995262718704, 194.9999999999999716, 22.12161802415705480 ) ) ;
#17862 = CARTESIAN_POINT ( 'NONE',  ( -60.28794563604517975, 206.7903428501025758, 3.378800118222471838 ) ) ;
#17863 = CARTESIAN_POINT ( 'NONE',  ( -38.12872103062154849, 203.4690446883607535, 1.626142955000567936 ) ) ;
#17864 = CARTESIAN_POINT ( 'NONE',  ( 28.02930337212723089, -5.407089921784859143, 166.1637690562780278 ) ) ;
#17865 = ORIENTED_EDGE ( 'NONE', *, *, #29381, .F. ) ;
#17866 = CARTESIAN_POINT ( 'NONE',  ( -28.69006028236768913, 203.2074086957352108, 4.234161556416165872 ) ) ;
#17867 = CARTESIAN_POINT ( 'NONE',  ( 10.83675517735179206, 9.939813717898537959, -11.08355503943118769 ) ) ;
#17868 = CARTESIAN_POINT ( 'NONE',  ( -58.90997103062156981, 217.3034525342668815, 4.350049139982096413 ) ) ;
#17869 = CARTESIAN_POINT ( 'NONE',  ( -9.500000000000005329, 132.3101862821014549, -0.1745138560725176813 ) ) ;
#17870 = CARTESIAN_POINT ( 'NONE',  ( -0.1745138560725500443, 28.81018628210144072, 12.50000000000000355 ) ) ;
#17871 = CARTESIAN_POINT ( 'NONE',  ( 10.56230152254411259, -3.464101615137761048, -7.612500000000058442 ) ) ;
#17872 = VERTEX_POINT ( 'NONE', #18514 ) ;
#17873 = CARTESIAN_POINT ( 'NONE',  ( -48.61830436395490551, 209.8844732041982581, 6.500000000000000888 ) ) ;
#17874 = CARTESIAN_POINT ( 'NONE',  ( 0.1745138560725837118, 125.4101862821014635, -15.50000000000000533 ) ) ;
#17875 = CARTESIAN_POINT ( 'NONE',  ( -7.234628195640302017, 198.8549038117967029, 27.00000000000000711 ) ) ;
#17876 = CARTESIAN_POINT ( 'NONE',  ( 7.954856959092191815, 8.972686282101431487, 5.529263428287477744 ) ) ;
#17877 = CARTESIAN_POINT ( 'NONE',  ( -13.62178482187498396, 196.7843750006145456, 23.59362340125808188 ) ) ;
#17878 = LINE ( 'NONE', #6497, #10501 ) ;
#17879 = CARTESIAN_POINT ( 'NONE',  ( 15.00000000000000000, 249.9296875003072387, 0.000000000000000000 ) ) ;
#17880 = LINE ( 'NONE', #32265, #37006 ) ;
#17881 = FACE_OUTER_BOUND ( 'NONE', #14113, .T. ) ;
#17882 = CARTESIAN_POINT ( 'NONE',  ( 23.87821517812500005, 242.8093750006145228, 4.985214923628404016 ) ) ;
#17883 = CARTESIAN_POINT ( 'NONE',  ( 9.534712964251900402, 84.97731371789856780, 1.715153634034445540 ) ) ;
#17884 = DIRECTION ( 'NONE',  ( 0.000000000000000000, 0.000000000000000000, 1.000000000000000000 ) ) ;
#17885 = ORIENTED_EDGE ( 'NONE', *, *, #36247, .F. ) ;
#17886 = CARTESIAN_POINT ( 'NONE',  ( -57.12872103062157692, 203.4690446883607535, 1.626142955000567936 ) ) ;
#17887 = CARTESIAN_POINT ( 'NONE',  ( 23.99999999999999645, 247.2062500012290229, -5.196152422706631135 ) ) ;
#17888 = CARTESIAN_POINT ( 'NONE',  ( -12.50000000000000355, 107.6898137178985735, 0.1745138560722786503 ) ) ;
#17889 = CARTESIAN_POINT ( 'NONE',  ( 22.80587116629411781, 3.604726614523243278, -0.8343749993855380520 ) ) ;
#17890 = CARTESIAN_POINT ( 'NONE',  ( 33.70656984979341786, -5.407089921784855591, 159.4182941109592093 ) ) ;
#17891 = CARTESIAN_POINT ( 'NONE',  ( 26.75643035624999655, -3.323476615752267715, -1.415624999385507232 ) ) ;
#17892 = CARTESIAN_POINT ( 'NONE',  ( -10.49813415416004858, 60.82731371789855501, 7.228626920338839135 ) ) ;
#17893 = CARTESIAN_POINT ( 'NONE',  ( -1.926257025242585782E-15, 197.9468750006145399, -31.45816453501075927 ) ) ;
#17894 = AXIS2_PLACEMENT_3D ( 'NONE', #5696, #31666, #28815 ) ;
#17895 = VERTEX_POINT ( 'NONE', #27393 ) ;
#17896 = VERTEX_POINT ( 'NONE', #24374 ) ;
#17897 = CARTESIAN_POINT ( 'NONE',  ( 23.87821517812500005, -4.985214923628404016, -5.840624999385479299 ) ) ;
#17898 = CARTESIAN_POINT ( 'NONE',  ( 19.56230152254410726, 5.196152422706631135, -6.337499998771006560 ) ) ;
#17899 = CARTESIAN_POINT ( 'NONE',  ( 15.24356964374999990, 246.5968750006145171, 0.000000000000000000 ) ) ;
#17900 = CARTESIAN_POINT ( 'NONE',  ( 10.49813415415989581, 36.57268628210145067, 7.228626920339068285 ) ) ;
#17901 = CARTESIAN_POINT ( 'NONE',  ( -45.24627896937849414, 203.4690446883607535, -1.626142955000504209 ) ) ;
#17902 =( LENGTH_UNIT ( ) NAMED_UNIT ( * ) SI_UNIT ( .MILLI., .METRE. ) );
#17903 = CARTESIAN_POINT ( 'NONE',  ( -31.98586230271182984, 207.8500491399821613, 3.954877714930852495 ) ) ;
#17904 = SURFACE_STYLE_USAGE ( .BOTH. , #12200 ) ;
#17905 = CARTESIAN_POINT ( 'NONE',  ( 30.79194769780577445, 6.928203230275506996, 161.9224743318320634 ) ) ;
#17906 = CARTESIAN_POINT ( 'NONE',  ( 8.962234695871567070, 85.83981371789856496, 8.715434833792127023 ) ) ;
#17907 = CARTESIAN_POINT ( 'NONE',  ( -63.65997103062157692, 213.8393509191290889, 2.350049139982164359 ) ) ;
#17908 = CARTESIAN_POINT ( 'NONE',  ( -64.84747103062156270, 213.3500491399821328, -5.571401726697985168 ) ) ;
#17909 = CARTESIAN_POINT ( 'NONE',  ( 23.87821517812499650, 4.985214923628404904, -7.153124999385473970 ) ) ;
#17910 = CARTESIAN_POINT ( 'NONE',  ( -8.632099005475794229, 69.45231371789853370, 13.23911966647199812 ) ) ;
#17911 = CARTESIAN_POINT ( 'NONE',  ( -58.90252896937851546, 205.6499508600178103, -7.303452534266820173 ) ) ;
#17912 = VECTOR ( 'NONE', #34325, 1000.000000000000000 ) ;
#17913 = ORIENTED_EDGE ( 'NONE', *, *, #19662, .T. ) ;
#17914 = DIRECTION ( 'NONE',  ( 0.000000000000000000, 0.000000000000000000, 1.000000000000000000 ) ) ;
#17915 = CARTESIAN_POINT ( 'NONE',  ( 10.69584247140445221, 90.04768628210145209, -6.932735513423970097 ) ) ;
#17916 = CARTESIAN_POINT ( 'NONE',  ( 5.770363421893814682, 46.63518628210144357, 14.38691631536207183 ) ) ;
#17917 = CARTESIAN_POINT ( 'NONE',  ( 19.39230484541326760, 243.3424038105676743, 5.999999999999999112 ) ) ;
#17918 = CARTESIAN_POINT ( 'NONE',  ( 33.78010750773675852, -5.407089921784861808, 160.2588333874741124 ) ) ;
#17919 = CARTESIAN_POINT ( 'NONE',  ( 13.04141134922759804, 54.97268628210144215, 8.927990412390657937 ) ) ;
#17920 = CARTESIAN_POINT ( 'NONE',  ( 27.24356964375000700, 199.5406250006145967, 15.72908226750537075 ) ) ;
#17921 = CARTESIAN_POINT ( 'NONE',  ( 16.56230152254410726, 7.209453229046475009, -9.253124999385514471 ) ) ;
#17922 = CARTESIAN_POINT ( 'NONE',  ( 15.00000000000017408, -3.464101615137856083, -2.156249998770938703 ) ) ;
#17923 = CARTESIAN_POINT ( 'NONE',  ( -55.14955436395487709, 214.8429017333601792, -4.673758765035196383 ) ) ;
#17924 = EDGE_CURVE ( 'NONE', #12908, #21187, #11479, .T. ) ;
#17925 = CARTESIAN_POINT ( 'NONE',  ( 20.99999999999999289, 241.3937500012289945, -5.999999999999997335 ) ) ;
#17926 = CARTESIAN_POINT ( 'NONE',  ( -6.932735513423968321, 32.54768628210144499, -10.69584247140445221 ) ) ;
#17927 = CARTESIAN_POINT ( 'NONE',  ( 6.000000000000000000, -20.00000000000000000, 20.00000000000000000 ) ) ;
#17928 = CARTESIAN_POINT ( 'NONE',  ( -7.954856959092309943, 143.6273137178985451, 5.529263428287300108 ) ) ;
#17929 = CARTESIAN_POINT ( 'NONE',  ( 18.12178482187499640, 247.5343750006145456, -4.985214923628404904 ) ) ;
#17930 = ORIENTED_EDGE ( 'NONE', *, *, #18990, .F. ) ;
#17931 = CARTESIAN_POINT ( 'NONE',  ( 23.99999999999999645, 5.196152422706631135, -6.000000000000005329 ) ) ;
#17932 = CARTESIAN_POINT ( 'NONE',  ( 20.99999999999997513, 244.9937500012290457, -5.999999999999999112 ) ) ;
#17933 = CYLINDRICAL_SURFACE ( 'NONE', #31637, 5.999999999999994671 ) ;
#17934 = CARTESIAN_POINT ( 'NONE',  ( 16.56230152254410726, 7.209453229046475009, -5.203124999385489780 ) ) ;
#17935 = CARTESIAN_POINT ( 'NONE',  ( 34.38638464322509947, 5.407089921784857367, 167.1886127560748321 ) ) ;
#17936 = CARTESIAN_POINT ( 'NONE',  ( 26.99999999999999645, 240.3250000000000171, -7.347880794884117764E-16 ) ) ;
#17937 = CARTESIAN_POINT ( 'NONE',  ( 27.64975160693779443, 5.196152422706630247, 160.4281484046883293 ) ) ;
#17938 = CARTESIAN_POINT ( 'NONE',  ( 7.228626920339069173, 43.47268628210144925, -10.49813415415989404 ) ) ;
#17939 = ORIENTED_EDGE ( 'NONE', *, *, #14057, .T. ) ;
#17940 = EDGE_LOOP ( 'NONE', ( #11449, #32754, #36567, #2219 ) ) ;
#17941 = CARTESIAN_POINT ( 'NONE',  ( 24.97165984609394940, 0.000000000000000000, 164.2385592436587558 ) ) ;
#17942 = CARTESIAN_POINT ( 'NONE',  ( 22.56230152254361698, -3.464101615138046597, -2.962500000000023892 ) ) ;
#17943 = CARTESIAN_POINT ( 'NONE',  ( 22.60769515458672529, 246.7174038105676743, -6.000000000000004441 ) ) ;
#17944 = CARTESIAN_POINT ( 'NONE',  ( 33.75438506914960612, -5.196152422706635576, 161.3621486929372111 ) ) ;
#17945 = CARTESIAN_POINT ( 'NONE',  ( 15.24356964375000167, -3.323476615752272600, -6.853124999385484806 ) ) ;
#17946 = CARTESIAN_POINT ( 'NONE',  ( -8.962234695871760692, 103.5601862821014549, 8.715434833791933400 ) ) ;
#17947 = CARTESIAN_POINT ( 'NONE',  ( -13.23911966647199812, 25.75231371789854506, -8.632099005475788900 ) ) ;
#17948 = CARTESIAN_POINT ( 'NONE',  ( 24.82458453031440726, 0.000000000000000000, 162.5574806918533000 ) ) ;
#17949 = EDGE_CURVE ( 'NONE', #7130, #32512, #18132, .T. ) ;
#17950 = VECTOR ( 'NONE', #13304, 1000.000000000000000 ) ;
#17951 = CARTESIAN_POINT ( 'NONE',  ( 21.00000000000000000, 240.0718750006145399, 6.646953231504538984 ) ) ;
#17952 = CARTESIAN_POINT ( 'NONE',  ( -66.22544563604516554, 213.3788001182224718, 3.209657149897419348 ) ) ;
#17953 = CARTESIAN_POINT ( 'NONE',  ( -4.499999999999999112, 226.9729365756407731, 2.499999999999999112 ) ) ;
#17954 = CARTESIAN_POINT ( 'NONE',  ( 27.54068648934820729, 5.407089921784862696, 160.5788525301012157 ) ) ;
#17955 = CARTESIAN_POINT ( 'NONE',  ( 6.594114490232462877, 19.13981371789855146, -6.840914352311949109 ) ) ;
#17956 = CARTESIAN_POINT ( 'NONE',  ( -57.12872103062157692, 203.4690446883607535, 1.626142955000567936 ) ) ;
#17957 = CARTESIAN_POINT ( 'NONE',  ( -67.02455436395489130, 203.6929966515020283, 6.137860380172978303 ) ) ;
#17958 = EDGE_CURVE ( 'NONE', #762, #33635, #30244, .T. ) ;
#17959 = DIRECTION ( 'NONE',  ( 1.000000000000000000, 0.000000000000000000, 0.000000000000000000 ) ) ;
#17960 = CARTESIAN_POINT ( 'NONE',  ( 26.99999999999999645, 247.1125000000000114, -3.464101615137755275 ) ) ;
#17961 = CARTESIAN_POINT ( 'NONE',  ( 27.24356964374999635, 196.5218750006145569, -15.72908226750539029 ) ) ;
#17962 = CARTESIAN_POINT ( 'NONE',  ( -8.632099005475794229, 133.8523137178985394, 13.23911966647199812 ) ) ;
#17963 = CARTESIAN_POINT ( 'NONE',  ( -60.88169563604516554, 210.1155267958017703, 6.500000000000000888 ) ) ;
#17964 = ORIENTED_EDGE ( 'NONE', *, *, #12440, .F. ) ;
#17965 = CARTESIAN_POINT ( 'NONE',  ( -10.49813415415989581, 41.17268628210144499, -7.228626920339068285 ) ) ;
#17966 = CARTESIAN_POINT ( 'NONE',  ( 26.99999999999999645, 245.3687500012290457, -3.464101615137755275 ) ) ;
#17967 = DIRECTION ( 'NONE',  ( 0.000000000000000000, 0.000000000000000000, 1.000000000000000000 ) ) ;
#17968 = CARTESIAN_POINT ( 'NONE',  ( 24.98966720158236043, -3.604726614523244610, 167.2390325064633885 ) ) ;
#17969 = CARTESIAN_POINT ( 'NONE',  ( 21.00000000000000000, -6.928203230275506996, -3.431249998770965703 ) ) ;
#17970 = DIRECTION ( 'NONE',  ( 0.000000000000000000, 0.000000000000000000, -1.000000000000000000 ) ) ;
#17971 = CARTESIAN_POINT ( 'NONE',  ( 16.56230152254411436, 7.209453229046475009, -1.153124999385528371 ) ) ;
#17972 = CARTESIAN_POINT ( 'NONE',  ( 0.1745138560725194299, 51.81018628210144783, -9.500000000000005329 ) ) ;
#17973 = LINE ( 'NONE', #29516, #22518 ) ;
#17974 = DIRECTION ( 'NONE',  ( 0.000000000000000000, 0.000000000000000000, 1.000000000000000000 ) ) ;
#17975 = CARTESIAN_POINT ( 'NONE',  ( -4.622313124798576922, 88.03518628210144925, -11.61527771782819762 ) ) ;
#17976 = CARTESIAN_POINT ( 'NONE',  ( 26.99999999999999645, 7.347880794884117764E-16, -0.2250000000000029754 ) ) ;
#17977 = DIRECTION ( 'NONE',  ( -0.000000000000000000, -1.000000000000000000, -0.000000000000000000 ) ) ;
#17978 = ORIENTED_EDGE ( 'NONE', *, *, #29163, .F. ) ;
#17979 = CARTESIAN_POINT ( 'NONE',  ( 27.50636891564131759, 5.407089921784856479, 160.1866008677275772 ) ) ;
#17980 = CARTESIAN_POINT ( 'NONE',  ( 15.24356964375000167, -3.323476615752272600, -10.00312499938545407 ) ) ;
#17982 = EDGE_CURVE ( 'NONE', #36330, #31630, #4271, .T. ) ;
#17981 = CARTESIAN_POINT ( 'NONE',  ( -13.50000000000000533, 195.5375000012290343, -23.38268590217984411 ) ) ;
#17983 = CARTESIAN_POINT ( 'NONE',  ( 37.21357869082257253, 3.604726614523243278, 163.6851247292908624 ) ) ;
#17984 = PRODUCT_DEFINITION_CONTEXT ( 'detailed design', #29401, 'design' ) ;
#17985 = CARTESIAN_POINT ( 'NONE',  ( 36.87043443719328195, 3.464101615137759271, 162.5576162106534639 ) ) ;
#17986 = CARTESIAN_POINT ( 'NONE',  ( 15.00000000000000000, 0.000000000000000000, -7.143749998770959841 ) ) ;
#17987 = CARTESIAN_POINT ( 'NONE',  ( 21.00000000000000000, 248.3124999999999716, 6.928203230275506996 ) ) ;
#17988 = CARTESIAN_POINT ( 'NONE',  ( 13.62178482187501416, 195.4531250006145342, 23.59362340125806767 ) ) ;
#17989 = CARTESIAN_POINT ( 'NONE',  ( -11.48171059495408208, 107.1148137178985564, 4.944772684328421875 ) ) ;
#17990 = CARTESIAN_POINT ( 'NONE',  ( -10.49813415415989404, 96.37268628210145494, -7.228626920339069173 ) ) ;
#17991 = VERTEX_POINT ( 'NONE', #24557 ) ;
#17992 = CARTESIAN_POINT ( 'NONE',  ( -13.62178482187498396, 194.9281250006145569, 23.59362340125808188 ) ) ;
#17993 = CARTESIAN_POINT ( 'NONE',  ( 20.00041244883536606, 239.7473985345926053, -5.668978318349186196 ) ) ;
#17994 = AXIS2_PLACEMENT_3D ( 'NONE', #23443, #5437, #34996 ) ;
#17995 = EDGE_CURVE ( 'NONE', #24114, #26868, #26832, .T. ) ;
#17996 = CARTESIAN_POINT ( 'NONE',  ( -15.50000000000000533, 70.88981371789854791, 0.1745138560722471477 ) ) ;
#17997 = CARTESIAN_POINT ( 'NONE',  ( 23.87821517812500005, -4.985214923628404016, -3.253124999385486937 ) ) ;
#17998 = CARTESIAN_POINT ( 'NONE',  ( 26.75643035624999655, 247.8343750006145285, -7.049594010296217766E-16 ) ) ;
#17999 = CARTESIAN_POINT ( 'NONE',  ( -3.796722387233375073, 102.9851862821014805, 8.710071997420127943 ) ) ;
#18000 = EDGE_CURVE ( 'NONE', #8445, #36238, #7950, .T. ) ;
#18001 = CARTESIAN_POINT ( 'NONE',  ( 26.99999999999999645, 194.9750000012290343, -15.58845726811990495 ) ) ;
#18002 = CARTESIAN_POINT ( 'NONE',  ( 5.233372021372610483, 74.05231371789854222, -8.152565276336593669 ) ) ;
#18003 = CARTESIAN_POINT ( 'NONE',  ( 16.56230152254411081, -7.209453229046475009, -5.428124999385503635 ) ) ;
#18004 = CARTESIAN_POINT ( 'NONE',  ( 23.87821517812499650, 242.3968750006145285, -4.985214923628404904 ) ) ;
#18005 = CARTESIAN_POINT ( 'NONE',  ( -12.50000000000000355, 52.48981371789855643, 0.1745138560722786503 ) ) ;
#18006 = DIRECTION ( 'NONE',  ( -1.000000000000000000, 0.000000000000000000, 0.000000000000000000 ) ) ;
#18007 = CARTESIAN_POINT ( 'NONE',  ( -4.622313124798576922, 106.4351862821014549, -11.61527771782819762 ) ) ;
#18008 = CARTESIAN_POINT ( 'NONE',  ( 10.56230152254410903, 0.000000000000000000, -6.187499998771023080 ) ) ;
#18009 = CARTESIAN_POINT ( 'NONE',  ( -68.80580436395490551, 214.5000000000000284, 0.1155267958017899832 ) ) ;
#18010 = CARTESIAN_POINT ( 'NONE',  ( 11.48171059495397728, 137.4851862821014663, 4.944772684328674117 ) ) ;
#18011 = CARTESIAN_POINT ( 'NONE',  ( 37.13350435217316203, -3.604726614523235284, 162.7698708504190677 ) ) ;
#18012 = CARTESIAN_POINT ( 'NONE',  ( 5.770363421893814682, 74.23518628210142367, 14.38691631536207183 ) ) ;
#18013 = CARTESIAN_POINT ( 'NONE',  ( 10.31873187879410736, 0.000000000000000000, -2.896874999385512517 ) ) ;
#18014 = DIRECTION ( 'NONE',  ( 0.000000000000000000, -1.000000000000000000, 0.000000000000000000 ) ) ;
#18015 = PLANE ( 'NONE',  #2495 ) ;
#18016 = CARTESIAN_POINT ( 'NONE',  ( -47.00000000000000711, 252.0000000000000000, 2.500000000000001776 ) ) ;
#18017 = CARTESIAN_POINT ( 'NONE',  ( -8.152565276336710909, 113.0476862821014663, 5.233372021372435512 ) ) ;
#18018 = CARTESIAN_POINT ( 'NONE',  ( 15.00000000000000000, 0.000000000000000000, -2.193749998770949894 ) ) ;
#18019 = CARTESIAN_POINT ( 'NONE',  ( 10.83675517735155225, 18.46018628210144286, 11.08355503943142573 ) ) ;
#18020 = CARTESIAN_POINT ( 'NONE',  ( -13.62178482187500528, 196.6343750006145399, -23.59362340125807123 ) ) ;
#18021 = CARTESIAN_POINT ( 'NONE',  ( 26.75643035624999655, 241.8718750006145228, -7.049594010296217766E-16 ) ) ;
#18022 = ORIENTED_EDGE ( 'NONE', *, *, #12859, .T. ) ;
#18023 = CARTESIAN_POINT ( 'NONE',  ( 24.99456971211191103, -3.604726614523240613, 167.2950684582310146 ) ) ;
#18024 = CARTESIAN_POINT ( 'NONE',  ( 18.12178482187499640, 4.985214923628404904, -2.465624999385462868 ) ) ;
#18025 = ADVANCED_FACE ( 'NONE', ( #12432, #35547 ), #9592, .F. ) ;
#18026 = CARTESIAN_POINT ( 'NONE',  ( -13.62178482187498396, 199.0343750006145456, 23.59362340125808188 ) ) ;
#18028 = FACE_OUTER_BOUND ( 'NONE', #10357, .T. ) ;
#18027 =( BOUNDED_CURVE ( )  B_SPLINE_CURVE ( 2, ( #2644, #14220, #9280, #14966, #24064, #3960, #32958 ),
 .UNSPECIFIED., .F., .F. ) 
 B_SPLINE_CURVE_WITH_KNOTS ( ( 3, 2, 2, 3 ),
 ( 0.2826086956521750015, 0.2898550724637684040, 0.2971014492753618064, 0.3043478260869552088 ),
 .UNSPECIFIED. ) 
 CURVE ( )  GEOMETRIC_REPRESENTATION_ITEM ( )  RATIONAL_B_SPLINE_CURVE ( ( 0.9999999999999794609, 0.8660254037844592467, 1.000000000000000000, 0.8660254037844387076, 1.000000000000000000, 0.8660254037844633546, 0.9999999999999753530 ) ) 
 REPRESENTATION_ITEM ( '' )  );
#18029 = DIRECTION ( 'NONE',  ( 0.000000000000000000, -0.000000000000000000, 1.000000000000000000 ) ) ;
#18030 = CARTESIAN_POINT ( 'NONE',  ( 28.08444087378459741, -5.196152422706638241, 165.3966694601965060 ) ) ;
#18031 = FACE_OUTER_BOUND ( 'NONE', #13507, .T. ) ;
#18032 = CARTESIAN_POINT ( 'NONE',  ( 8.710071997420211432, 28.91481371789854649, -3.796722387233181895 ) ) ;
#18033 = CARTESIAN_POINT ( 'NONE',  ( 31.15473347688575956, -6.928203230275514990, 166.0691347614145741 ) ) ;
#18034 = VERTEX_POINT ( 'NONE', #9891 ) ;
#18035 = CARTESIAN_POINT ( 'NONE',  ( 15.24356964374999990, 246.5593750006144944, -3.323476615752268604 ) ) ;
#18036 = CARTESIAN_POINT ( 'NONE',  ( 2.660918448318003282, 40.70231371789854791, 12.46528703574811558 ) ) ;
#18037 = CARTESIAN_POINT ( 'NONE',  ( 21.00000000000000000, 6.646953231504538984, -0.7031249993854685743 ) ) ;
#18038 = CARTESIAN_POINT ( 'NONE',  ( -15.53471296425188442, 135.5773137178985905, -2.908627838312459080 ) ) ;
#18039 = CARTESIAN_POINT ( 'NONE',  ( 24.00000000000000000, -5.196152422706629359, -6.093749998770964460 ) ) ;
#18040 = CARTESIAN_POINT ( 'NONE',  ( 10.49999999999999822, 210.0000000000000284, 2.500000000000000000 ) ) ;
#18041 = ORIENTED_EDGE ( 'NONE', *, *, #37182, .T. ) ;
#18042 = CARTESIAN_POINT ( 'NONE',  ( 13.44051670066911441, -5.407089921784865361, -4.171874999385538629 ) ) ;
#18043 = ORIENTED_EDGE ( 'NONE', *, *, #6796, .T. ) ;
#18044 = AXIS2_PLACEMENT_3D ( 'NONE', #6718, #5962, #29646 ) ;
#18045 = CARTESIAN_POINT ( 'NONE',  ( 13.62178482187501416, 199.0531250006145285, 23.59362340125806767 ) ) ;
#18046 = CARTESIAN_POINT ( 'NONE',  ( 27.97210741594907901, 5.407089921784862696, 165.5100162856553538 ) ) ;
#18047 =( BOUNDED_CURVE ( )  B_SPLINE_CURVE ( 2, ( #13280, #37131, #7409, #25019, #30902, #31273, #16693 ),
 .UNSPECIFIED., .F., .F. ) 
 B_SPLINE_CURVE_WITH_KNOTS ( ( 3, 2, 2, 3 ),
 ( 0.2173913043478263585, 0.2246376811594206213, 0.2318840579710148841, 0.2391304347826091470 ),
 .UNSPECIFIED. ) 
 CURVE ( )  GEOMETRIC_REPRESENTATION_ITEM ( )  RATIONAL_B_SPLINE_CURVE ( ( 0.9999999999999948930, 0.8660254037844438146, 1.000000000000000000, 0.8660254037844387076, 1.000000000000000000, 0.8660254037844304920, 1.000000000000008216 ) ) 
 REPRESENTATION_ITEM ( '' )  );
#18048 = CARTESIAN_POINT ( 'NONE',  ( -64.04836230271183695, 202.5810206699313767, -4.149950860017804111 ) ) ;
#18049 = AXIS2_PLACEMENT_3D ( 'NONE', #6308, #9153, #20536 ) ;
#18050 = CARTESIAN_POINT ( 'NONE',  ( 18.12178482187500350, 249.3718750006145228, 4.985214923628407568 ) ) ;
#18051 = CARTESIAN_POINT ( 'NONE',  ( 7.234628195640363302, 196.7174038105676459, -26.99999999999996803 ) ) ;
#18052 = CARTESIAN_POINT ( 'NONE',  ( -50.59002896937850835, 206.1606490808709111, 2.350049139982143931 ) ) ;
#18053 = CARTESIAN_POINT ( 'NONE',  ( 27.00000000000000355, 197.0749999999999886, -3.306546357697854128E-15 ) ) ;
#18054 = CARTESIAN_POINT ( 'NONE',  ( 28.10774354060011504, -5.407089921784859143, 167.0603442845606139 ) ) ;
#18055 = ORIENTED_EDGE ( 'NONE', *, *, #8424, .F. ) ;
#18056 = CARTESIAN_POINT ( 'NONE',  ( -13.23911966647199812, 7.352313717898546486, -8.632099005475788900 ) ) ;
#18057 = CARTESIAN_POINT ( 'NONE',  ( -63.46205436395489841, 216.1378603801730094, 6.307003348497944195 ) ) ;
#18058 = CARTESIAN_POINT ( 'NONE',  ( 7.954856959092191815, 128.5726862821014436, 5.529263428287477744 ) ) ;
#18059 = CARTESIAN_POINT ( 'NONE',  ( 15.00000000000000178, 249.1937500012290343, 3.464101615137757051 ) ) ;
#18060 = EDGE_CURVE ( 'NONE', #24643, #36194, #10971, .T. ) ;
#18061 = CARTESIAN_POINT ( 'NONE',  ( -8.715434833791929847, 23.06018628210145138, -8.962234695871762469 ) ) ;
#18062 = CARTESIAN_POINT ( 'NONE',  ( 19.56230152254412502, 5.196152422706637353, -6.000000000000060396 ) ) ;
#18063 = CLOSED_SHELL ( 'NONE', ( #30103, #12216, #28031, #18693, #12453, #20499, #30224, #10277, #19793, #11676, #32555, #3446 ) ) ;
#18064 = VECTOR ( 'NONE', #27188, 1000.000000000000000 ) ;
#18065 = ORIENTED_EDGE ( 'NONE', *, *, #31699, .F. ) ;
#18066 = DIRECTION ( 'NONE',  ( 0.000000000000000000, 0.000000000000000000, -1.000000000000000000 ) ) ;
#18067 = CARTESIAN_POINT ( 'NONE',  ( 14.38691631536207538, 127.1351862821014720, -5.770363421893813793 ) ) ;
#18068 = DIRECTION ( 'NONE',  ( 0.000000000000000000, 1.000000000000000000, 0.000000000000000000 ) ) ;
#18069 = CARTESIAN_POINT ( 'NONE',  ( -9.500000000000005329, 144.4898137178985280, 0.1745138560723101806 ) ) ;
#18070 = CARTESIAN_POINT ( 'NONE',  ( -13.62178482187500528, 198.8281250006145342, -23.59362340125807123 ) ) ;
#18071 = CARTESIAN_POINT ( 'NONE',  ( 16.25485273795005625, -6.235291796180306712, -10.00000000000000000 ) ) ;
#18072 = ADVANCED_FACE ( 'NONE', ( #36039, #21652 ), #35662, .T. ) ;
#18073 = CARTESIAN_POINT ( 'NONE',  ( 15.93765667431398825, -3.220065975715824536, -8.000000000000000000 ) ) ;
#18074 = CYLINDRICAL_SURFACE ( 'NONE', #29645, 5.999999999999994671 ) ;
#18075 = CARTESIAN_POINT ( 'NONE',  ( -8.710071997420207879, 79.51481371789856212, 3.796722387233182339 ) ) ;
#18076 = LINE ( 'NONE', #35487, #9386 ) ;
#18077 = ORIENTED_EDGE ( 'NONE', *, *, #22157, .F. ) ;
#18078 = PRODUCT_DEFINITION ( 'UNKNOWN', '', #19036, #21021 ) ;
#18079 = CARTESIAN_POINT ( 'NONE',  ( 21.00000000000000000, 243.1937500012290627, -6.928203230275506996 ) ) ;
#18080 = CARTESIAN_POINT ( 'NONE',  ( -4.622313124798826500, 105.9648137178985650, 11.61527771782809637 ) ) ;
#18081 = CARTESIAN_POINT ( 'NONE',  ( 10.31873187879410736, 0.000000000000000000, -3.346874999385518468 ) ) ;
#18082 = CARTESIAN_POINT ( 'NONE',  ( 18.00000000000000355, 246.9250000000000114, 5.196152422706632912 ) ) ;
#18083 = CARTESIAN_POINT ( 'NONE',  ( 18.12178482187500350, -4.985214923628407568, -5.578124999385480898 ) ) ;
#18084 = CARTESIAN_POINT ( 'NONE',  ( -2.311890736173448424, 68.87731371789855928, 12.53471296425189330 ) ) ;
#18085 = CARTESIAN_POINT ( 'NONE',  ( 13.62178482187501416, 197.3093750006145513, 23.59362340125806767 ) ) ;
#18086 = ORIENTED_EDGE ( 'NONE', *, *, #5692, .T. ) ;
#18087 = VERTEX_POINT ( 'NONE', #12739 ) ;
#18088 = CARTESIAN_POINT ( 'NONE',  ( 15.24356964375000167, -3.323476615752272600, -5.953124999385460470 ) ) ;
#18089 = LINE ( 'NONE', #20740, #28195 ) ;
#18090 =( BOUNDED_CURVE ( )  B_SPLINE_CURVE ( 2, ( #30975, #4251, #27752, #27375, #30607, #21886, #4992 ),
 .UNSPECIFIED., .F., .F. ) 
 B_SPLINE_CURVE_WITH_KNOTS ( ( 3, 2, 2, 3 ),
 ( 0.6739130434782595325, 0.6811594202898538786, 0.6884057971014482247, 0.6956521739130425708 ),
 .UNSPECIFIED. ) 
 CURVE ( )  GEOMETRIC_REPRESENTATION_ITEM ( )  RATIONAL_B_SPLINE_CURVE ( ( 1.000000000000024647, 0.8660254037844140607, 1.000000000000000000, 0.8660254037844387076, 1.000000000000000000, 0.8660254037844551389, 0.9999999999999835687 ) ) 
 REPRESENTATION_ITEM ( '' )  );
#18091 = CARTESIAN_POINT ( 'NONE',  ( 23.87821517812499650, 245.9968750006145228, -4.985214923628404904 ) ) ;
#18092 = CARTESIAN_POINT ( 'NONE',  ( 2.311890736173175753, 37.72268628210144215, 12.53471296425194836 ) ) ;
#18093 = CARTESIAN_POINT ( 'NONE',  ( -33.76711230271184405, 216.4690446883607535, -1.857196546604089393 ) ) ;
#18094 = CARTESIAN_POINT ( 'NONE',  ( 22.80587116629410716, 3.604726614523238837, -1.678124999385517846 ) ) ;
#18095 = AXIS2_PLACEMENT_3D ( 'NONE', #25365, #33897, #37289 ) ;
#18096 = CARTESIAN_POINT ( 'NONE',  ( -63.65252896937849414, 206.6499508600178387, -5.571401726697954970 ) ) ;
#18097 = CARTESIAN_POINT ( 'NONE',  ( 27.84585202812001015, 5.196152422706630247, 162.6695864753947660 ) ) ;
#18098 = CARTESIAN_POINT ( 'NONE',  ( -2.660918448318004614, 82.10231371789855359, -12.46528703574811558 ) ) ;
#18099 = CARTESIAN_POINT ( 'NONE',  ( -54.95163769728822700, 213.9548777149308592, -2.149950860017830756 ) ) ;
#18100 = CARTESIAN_POINT ( 'NONE',  ( -37.73288769728823411, 201.5309553116392181, -2.393094931466246855 ) ) ;
#18101 = CARTESIAN_POINT ( 'NONE',  ( 20.99999999999999645, -6.646953231504538984, -5.990624999385490312 ) ) ;
#18102 = CARTESIAN_POINT ( 'NONE',  ( 10.56230152254438970, 3.464101615137910706, -0.8249999987710033844 ) ) ;
#18103 = CARTESIAN_POINT ( 'NONE',  ( 13.23911966647199812, 57.95231371789854791, 8.632099005475788900 ) ) ;
#18104 = CARTESIAN_POINT ( 'NONE',  ( -58.30877896937849414, 212.1620413398627534, -8.530955311639255356 ) ) ;
#18105 = DIRECTION ( 'NONE',  ( -0.000000000000000000, 1.000000000000000000, -0.000000000000000000 ) ) ;
#18106 = CARTESIAN_POINT ( 'NONE',  ( -10.49813415415989581, 77.97268628210144925, -7.228626920339068285 ) ) ;
#18107 = CARTESIAN_POINT ( 'NONE',  ( -11.08355503943142573, 29.96018628210143575, 10.83675517735155402 ) ) ;
#18108 = CARTESIAN_POINT ( 'NONE',  ( 15.00000000000000000, 0.000000000000000000, -6.693749998770953447 ) ) ;
#18109 = CARTESIAN_POINT ( 'NONE',  ( -35.67863628793905661, 245.9410842096246483, 5.000000000000000000 ) ) ;
#18110 = CARTESIAN_POINT ( 'NONE',  ( 14.25334919248782661, 45.48518628210144499, 6.092822981423971385 ) ) ;
#18111 = CARTESIAN_POINT ( 'NONE',  ( 27.24356964374999279, 199.6156250006145285, -15.72908226750539207 ) ) ;
#18112 = CARTESIAN_POINT ( 'NONE',  ( 10.31873187879411091, -3.604726614523240613, -9.103124999385528326 ) ) ;
#18113 = CYLINDRICAL_SURFACE ( 'NONE', #31106, 27.00000000000000000 ) ;
#18114 = CARTESIAN_POINT ( 'NONE',  ( -38.12872103062154849, 203.4690446883607535, 1.626142955000567936 ) ) ;
#18115 = CARTESIAN_POINT ( 'NONE',  ( 26.99999999999999645, 195.7625000000000171, -15.58845726811990495 ) ) ;
#18116 = CARTESIAN_POINT ( 'NONE',  ( 2.660918448318279950, 15.29768628210143078, -12.46528703574805697 ) ) ;
#18117 = CARTESIAN_POINT ( 'NONE',  ( -27.00000000000000355, 199.6625000012290343, 0.000000000000000000 ) ) ;
#18118 = CARTESIAN_POINT ( 'NONE',  ( 9.500000000000005329, 130.6898137178985451, -0.1745138560723090149 ) ) ;
#18119 = CARTESIAN_POINT ( 'NONE',  ( 26.75643035624999655, 245.5843750006145285, -7.049594010296217766E-16 ) ) ;
#18120 = EDGE_LOOP ( 'NONE', ( #18065, #23114, #32511, #23525 ) ) ;
#18121 = CARTESIAN_POINT ( 'NONE',  ( 26.99999999999999645, -3.464101615137751278, -6.562499999999983125 ) ) ;
#18122 = CARTESIAN_POINT ( 'NONE',  ( 20.99999999999999645, 6.928203230275506996, -3.262499999999992628 ) ) ;
#18123 = DIRECTION ( 'NONE',  ( 0.000000000000000000, 1.000000000000000000, 0.000000000000000000 ) ) ;
#18124 = CARTESIAN_POINT ( 'NONE',  ( 10.31873187879411269, -3.604726614523240613, -6.403124999385521043 ) ) ;
#18125 = CARTESIAN_POINT ( 'NONE',  ( 31.22091736908830839, -7.209453229046475009, 166.8256201108902133 ) ) ;
#18126 = CARTESIAN_POINT ( 'NONE',  ( 15.00000000000000178, 241.0374999999999943, 3.464101615137757051 ) ) ;
#18127 = CARTESIAN_POINT ( 'NONE',  ( 24.66443585301628616, 3.464101615138150514, 160.7269729341096536 ) ) ;
#18128 = EDGE_CURVE ( 'NONE', #3827, #21562, #788, .T. ) ;
#18129 = CARTESIAN_POINT ( 'NONE',  ( -12.46528703574805874, 49.79768628210144499, -2.660918448318280838 ) ) ;
#18130 = ORIENTED_EDGE ( 'NONE', *, *, #9448, .F. ) ;
#18131 = ORIENTED_EDGE ( 'NONE', *, *, #22482, .T. ) ;
#18132 = LINE ( 'NONE', #29674, #20646 ) ;
#18133 = CARTESIAN_POINT ( 'NONE',  ( 10.56230152254472188, -3.464101615138113210, -3.112499999999997158 ) ) ;
#18134 = CARTESIAN_POINT ( 'NONE',  ( 15.00000000000000000, 0.000000000000000000, -3.543749998770939769 ) ) ;
#18135 = CARTESIAN_POINT ( 'NONE',  ( 15.00000000000000000, 248.1625000000000227, -3.464101615137752610 ) ) ;
#18136 = CARTESIAN_POINT ( 'NONE',  ( 18.12178482187500350, -4.985214923628407568, -7.265624999385461358 ) ) ;
#18137 = CARTESIAN_POINT ( 'NONE',  ( -10.69584247140444866, 103.8476862821014493, 6.932735513423972762 ) ) ;
#18138 = CARTESIAN_POINT ( 'NONE',  ( -2.908627838312453306, 13.67731371789853867, 15.53471296425188797 ) ) ;
#18139 = CARTESIAN_POINT ( 'NONE',  ( -7.234628195640328663, 197.3924038105676857, 26.99999999999999289 ) ) ;
#18140 = CARTESIAN_POINT ( 'NONE',  ( 26.75643035624999655, 241.5343750006145456, -7.049594010296217766E-16 ) ) ;
#18141 = CARTESIAN_POINT ( 'NONE',  ( -35.15997103062156270, 213.8393509191290889, 2.350049139982164359 ) ) ;
#18142 = CARTESIAN_POINT ( 'NONE',  ( 0.000000000000000000, 200.0000000000000000, 0.000000000000000000 ) ) ;
#18143 = CARTESIAN_POINT ( 'NONE',  ( 28.41103801510778837, 5.957546011302761180, 159.5877722384327342 ) ) ;
#18144 = CARTESIAN_POINT ( 'NONE',  ( 2.660918448318002838, 132.7023137178985621, 12.46528703574811558 ) ) ;
#18145 = CARTESIAN_POINT ( 'NONE',  ( -55.54538769728823411, 211.8571965466039444, -6.469044688360768625 ) ) ;
#18146 = EDGE_CURVE ( 'NONE', #6822, #30347, #29982, .T. ) ;
#18147 = CARTESIAN_POINT ( 'NONE',  ( -34.95461230271183695, 207.6069050685336492, -8.469044688360751749 ) ) ;
#18148 = CARTESIAN_POINT ( 'NONE',  ( 20.99999999999997513, 247.1875000000000284, -5.999999999999999112 ) ) ;
#18149 = EDGE_CURVE ( 'NONE', #12997, #2700, #29792, .T. ) ;
#18150 = CARTESIAN_POINT ( 'NONE',  ( 13.62178482187501416, 197.7031250006145342, 23.59362340125806767 ) ) ;
#18151 = CARTESIAN_POINT ( 'NONE',  ( -15.50000000000000533, 116.8898137178985621, 0.1745138560722471477 ) ) ;
#18152 = CARTESIAN_POINT ( 'NONE',  ( -64.44419563604516554, 203.5000000000000000, 0.1155267958017914542 ) ) ;
#18153 = ORIENTED_EDGE ( 'NONE', *, *, #12470, .F. ) ;
#18154 = CARTESIAN_POINT ( 'NONE',  ( 4.622313124798573369, 19.03518628210144925, 11.61527771782819940 ) ) ;
#18155 = CARTESIAN_POINT ( 'NONE',  ( 26.99999999999999645, 7.347880794884117764E-16, -7.874999999999992895 ) ) ;
#18156 = CARTESIAN_POINT ( 'NONE',  ( 37.41297893579764633, -3.464101615137622936, 168.7589282062745610 ) ) ;
#18157 = CARTESIAN_POINT ( 'NONE',  ( 34.44684893975629336, -5.407089921784861808, 167.8797228278759803 ) ) ;
#18158 = CARTESIAN_POINT ( 'NONE',  ( -14.25334919248782306, 105.2851862821014777, -6.092822981423979378 ) ) ;
#18159 = DIRECTION ( 'NONE',  ( 0.000000000000000000, -1.000000000000000000, 0.000000000000000000 ) ) ;
#18160 = CARTESIAN_POINT ( 'NONE',  ( 19.68408634441910721, -5.407089921784855591, -2.240624999385543159 ) ) ;
#18161 = CARTESIAN_POINT ( 'NONE',  ( 8.843639120294328748, 53.53518628210145636, -3.474262827703334722 ) ) ;
#18162 = CARTESIAN_POINT ( 'NONE',  ( 15.00000000000000000, 240.5687500012290343, -3.464101615137752610 ) ) ;
#18163 = CARTESIAN_POINT ( 'NONE',  ( 26.99999999999999645, 244.7874999999999943, 3.464101615137751278 ) ) ;
#18164 = CARTESIAN_POINT ( 'NONE',  ( 12.50000000000000355, 81.71018628210144641, 0.1745138560725507937 ) ) ;
#18165 = CARTESIAN_POINT ( 'NONE',  ( 22.56230152254411792, 7.347880794884125653E-16, -5.175000000000040679 ) ) ;
#18166 = CARTESIAN_POINT ( 'NONE',  ( 16.56230152254410370, -6.928203230275506996, -7.874999998770976006 ) ) ;
#18167 = CARTESIAN_POINT ( 'NONE',  ( -4.694659320240884604E-14, 197.8625000000000114, 27.00000000000000000 ) ) ;
#18168 = CARTESIAN_POINT ( 'NONE',  ( 36.85896376251805862, -3.604726614523235284, 159.6318575514300449 ) ) ;
#18169 = CARTESIAN_POINT ( 'NONE',  ( 26.75643035624999655, 7.049594010296217766E-16, -8.915624999385475036 ) ) ;
#18170 = VECTOR ( 'NONE', #37207, 1000.000000000000000 ) ;
#18171 = CARTESIAN_POINT ( 'NONE',  ( 31.38024896135242159, 6.928203230275506996, 168.6467885439513452 ) ) ;
#18172 = CARTESIAN_POINT ( 'NONE',  ( 34.21152843433763024, -5.407089921784861808, 165.1899971430282505 ) ) ;
#18173 = CARTESIAN_POINT ( 'NONE',  ( 30.99785313993998415, -6.928203230275514990, 164.2759843048494872 ) ) ;
#18174 = CARTESIAN_POINT ( 'NONE',  ( 28.14980768084533125, 5.196152422706636465, 166.1438154837653656 ) ) ;
#18175 = CARTESIAN_POINT ( 'NONE',  ( 24.00000000000000000, 249.2500000000000000, 5.196152422706629359 ) ) ;
#18176 = CARTESIAN_POINT ( 'NONE',  ( 27.24356964375000700, 195.9406250006145456, 15.72908226750537075 ) ) ;
#18177 = EDGE_CURVE ( 'NONE', #8033, #36288, #19259, .T. ) ;
#18178 = CARTESIAN_POINT ( 'NONE',  ( 12.50000000000000355, 103.0898137178985650, -0.1745138560722771515 ) ) ;
#18179 = CARTESIAN_POINT ( 'NONE',  ( 2.660918448318279950, 98.09768628210146346, -12.46528703574805874 ) ) ;
#18180 = EDGE_LOOP ( 'NONE', ( #26341, #19730, #4967, #8426 ) ) ;
#18181 = CARTESIAN_POINT ( 'NONE',  ( -20.86978604919638869, 194.8026013911397740, -17.51182792271053046 ) ) ;
#18182 = CARTESIAN_POINT ( 'NONE',  ( 23.87821517812500005, 240.8968750006145285, 4.985214923628404016 ) ) ;
#18183 = CARTESIAN_POINT ( 'NONE',  ( -8.632099005475794229, 78.65231371789856496, 13.23911966647199812 ) ) ;
#18184 = CARTESIAN_POINT ( 'NONE',  ( 26.75643035624999655, -3.323476615752267715, -5.015624999385472904 ) ) ;
#18185 = CARTESIAN_POINT ( 'NONE',  ( 15.24356964375000167, 246.7468750006145228, 3.323476615752272600 ) ) ;
#18186 = VECTOR ( 'NONE', #10222, 1000.000000000000000 ) ;
#18187 = CARTESIAN_POINT ( 'NONE',  ( 9.465287035748067623, 91.19768628210145778, 2.064181346179272847 ) ) ;
#18188 = CARTESIAN_POINT ( 'NONE',  ( 10.56230152254410903, 7.347880794884117764E-16, -10.00000000000000000 ) ) ;
#18189 = CARTESIAN_POINT ( 'NONE',  ( -6.840914352311947333, 62.83981371789855785, -6.594114490232462877 ) ) ;
#18190 = CARTESIAN_POINT ( 'NONE',  ( 10.31873187879411091, 0.000000000000000000, -5.090624999385534366 ) ) ;
#18191 = EDGE_CURVE ( 'NONE', #22619, #23933, #596, .T. ) ;
#18192 = CARTESIAN_POINT ( 'NONE',  ( 6.840914352311949109, 104.2398137178985706, 6.594114490232462877 ) ) ;
#18193 = CARTESIAN_POINT ( 'NONE',  ( 0.000000000000000000, 210.0000000000000284, 0.000000000000000000 ) ) ;
#18194 = CARTESIAN_POINT ( 'NONE',  ( -7.228626920338836470, 44.72731371789855359, -10.49813415416005213 ) ) ;
#18195 = CARTESIAN_POINT ( 'NONE',  ( 2.999999999999997780, 244.5000000000000000, -2.500000000000000000 ) ) ;
#18196 = AXIS2_PLACEMENT_3D ( 'NONE', #9411, #28741, #14354 ) ;
#18197 = CARTESIAN_POINT ( 'NONE',  ( -4.622313124798576922, 97.23518628210145209, -11.61527771782819762 ) ) ;
#18198 = CARTESIAN_POINT ( 'NONE',  ( 10.56230152254411259, 3.464101615137752166, -6.224999998771012955 ) ) ;
#18199 = CARTESIAN_POINT ( 'NONE',  ( -63.46205436395489841, 213.2096571498974242, 3.378800118222489601 ) ) ;
#18200 = CARTESIAN_POINT ( 'NONE',  ( -11.48171059495397373, 132.8851862821014720, -4.944772684328680334 ) ) ;
#18201 = CARTESIAN_POINT ( 'NONE',  ( 24.75924920669326212, -3.604726614523240613, 164.6053427733833132 ) ) ;
#18202 = CARTESIAN_POINT ( 'NONE',  ( -15.46528703574804986, 86.59768628210143504, -3.257655550457287497 ) ) ;
#18203 = CARTESIAN_POINT ( 'NONE',  ( 22.80587116629412492, 3.604726614523243278, -3.534374999385544669 ) ) ;
#18204 = CARTESIAN_POINT ( 'NONE',  ( 18.00000000000000355, -5.196152422706632912, -4.874999999999990230 ) ) ;
#18205 = DIRECTION ( 'NONE',  ( 0.000000000000000000, 0.000000000000000000, 1.000000000000000000 ) ) ;
#18206 = CARTESIAN_POINT ( 'NONE',  ( -3.796722387233375073, 112.1851862821014691, 8.710071997420127943 ) ) ;
#18207 = CARTESIAN_POINT ( 'NONE',  ( 13.50000000000001421, 198.9125000012290343, 23.38268590217984055 ) ) ;
#18208 = CARTESIAN_POINT ( 'NONE',  ( -14.25334919248782306, 4.085186282101443744, -6.092822981423979378 ) ) ;
#18209 = CARTESIAN_POINT ( 'NONE',  ( 13.62178482187499640, 196.5593750006145513, -23.59362340125807123 ) ) ;
#18210 = CARTESIAN_POINT ( 'NONE',  ( 26.75643035624999655, 241.4218750006145058, -7.049594010296217766E-16 ) ) ;
#18212 = ORIENTED_EDGE ( 'NONE', *, *, #3126, .F. ) ;
#18211 = VECTOR ( 'NONE', #10271, 999.9999999999998863 ) ;
#18213 = CARTESIAN_POINT ( 'NONE',  ( 24.98803303140584120, 3.604726614523236616, 167.2203538558741513 ) ) ;
#18214 = CARTESIAN_POINT ( 'NONE',  ( 15.24356964374999990, 3.323476615752268604, -2.428124999385457894 ) ) ;
#18215 = EDGE_CURVE ( 'NONE', #3975, #2189, #14366, .T. ) ;
#18216 = CARTESIAN_POINT ( 'NONE',  ( 13.62178482187499640, 199.7093750006145285, -23.59362340125807123 ) ) ;
#18217 = DIRECTION ( 'NONE',  ( 1.000000000000000000, 0.000000000000000000, 0.000000000000000000 ) ) ;
#18218 = LINE ( 'NONE', #946, #26338 ) ;
#18219 = CARTESIAN_POINT ( 'NONE',  ( 20.99999999999999645, 6.928203230275506996, -3.206249998770952292 ) ) ;
#18220 = CARTESIAN_POINT ( 'NONE',  ( 27.00000000000001421, 198.8374999999999773, 15.58845726811988897 ) ) ;
#18221 = CARTESIAN_POINT ( 'NONE',  ( -5.529263428287297444, 26.32731371789854791, -7.954856959092311719 ) ) ;
#18222 = CARTESIAN_POINT ( 'NONE',  ( -13.62178482187498396, 197.2343750006145626, 23.59362340125808188 ) ) ;
#18224 = ORIENTED_EDGE ( 'NONE', *, *, #18646, .F. ) ;
#18223 = ORIENTED_EDGE ( 'NONE', *, *, #1576, .F. ) ;
#18225 = CARTESIAN_POINT ( 'NONE',  ( 23.87821517812499650, 245.9968750006145228, -4.985214923628404904 ) ) ;
#18226 = CARTESIAN_POINT ( 'NONE',  ( 4.622313124798831829, 27.76481371789854435, -11.61527771782809282 ) ) ;
#18227 = CARTESIAN_POINT ( 'NONE',  ( 15.24356964374999990, 0.000000000000000000, -1.490624999385459226 ) ) ;
#18228 = CARTESIAN_POINT ( 'NONE',  ( -15.53471296425188442, 126.3773137178985309, -2.908627838312459080 ) ) ;
#18229 = CARTESIAN_POINT ( 'NONE',  ( 21.00000000000000000, 6.928203230275506996, -7.706249998770941190 ) ) ;
#18230 = CARTESIAN_POINT ( 'NONE',  ( 1.120210788295102201E-13, 196.4000000012290741, -27.00000000000000711 ) ) ;
#18231 = ORIENTED_EDGE ( 'NONE', *, *, #18215, .F. ) ;
#18232 = CARTESIAN_POINT ( 'NONE',  ( 10.31873187879410558, 0.000000000000000000, -6.496874999385504168 ) ) ;
#18233 = CARTESIAN_POINT ( 'NONE',  ( -13.62178482187500528, 196.5781250006145342, -23.59362340125807123 ) ) ;
#18234 = CARTESIAN_POINT ( 'NONE',  ( 34.10694154304044901, 5.407089921784862696, 163.9945635053181547 ) ) ;
#18235 = CARTESIAN_POINT ( 'NONE',  ( -62.66294563604517265, 216.1378603801729241, -6.307003348498026796 ) ) ;
#18236 = CARTESIAN_POINT ( 'NONE',  ( 20.99999999999999645, 248.2843750006145171, -6.646953231504538984 ) ) ;
#18237 =( NAMED_UNIT ( * ) SI_UNIT ( $, .STERADIAN. ) SOLID_ANGLE_UNIT ( ) );
#18238 = CARTESIAN_POINT ( 'NONE',  ( -7.234628195640302017, 199.3049038117967200, 27.00000000000000711 ) ) ;
#18239 = CARTESIAN_POINT ( 'NONE',  ( -51.38169563604516554, 210.1155267958017703, 4.499999999999996447 ) ) ;
#18240 = DIRECTION ( 'NONE',  ( 0.000000000000000000, 1.000000000000000000, 0.000000000000000000 ) ) ;
#18241 = CARTESIAN_POINT ( 'NONE',  ( 37.36882485759181804, -3.604726614523235284, 165.4595965352667690 ) ) ;
#18242 = ORIENTED_EDGE ( 'NONE', *, *, #6466, .T. ) ;
#18243 = CARTESIAN_POINT ( 'NONE',  ( 20.99999999999999289, 241.8437500012290400, -5.999999999999997335 ) ) ;
#18244 = CARTESIAN_POINT ( 'NONE',  ( 14.25334919248795451, 10.51481371789855679, -6.092822981423661410 ) ) ;
#18245 = CARTESIAN_POINT ( 'NONE',  ( -49.80580436395490551, 218.5000000000000000, 0.1155267958017064944 ) ) ;
#18246 = CARTESIAN_POINT ( 'NONE',  ( 6.840914352312096547, 135.7601862821014720, -6.594114490232313663 ) ) ;
#18247 =( BOUNDED_CURVE ( )  B_SPLINE_CURVE ( 2, ( #30060, #33094, #27400, #26839, #9968, #18894, #7139 ),
 .UNSPECIFIED., .F., .F. ) 
 B_SPLINE_CURVE_WITH_KNOTS ( ( 3, 2, 2, 3 ),
 ( 0.3260869565217406896, 0.3333333333333340920, 0.3405797101449276054, 0.3478260869565210078 ),
 .UNSPECIFIED. ) 
 CURVE ( )  GEOMETRIC_REPRESENTATION_ITEM ( )  RATIONAL_B_SPLINE_CURVE ( ( 0.9999999999999712452, 0.8660254037844674624, 1.000000000000000000, 0.8660254037844387076, 1.000000000000000000, 0.8660254037844520303, 0.9999999999999866773 ) ) 
 REPRESENTATION_ITEM ( '' )  );
#18248 = FACE_OUTER_BOUND ( 'NONE', #34451, .T. ) ;
#18249 = CARTESIAN_POINT ( 'NONE',  ( -11.48171059495397373, 22.48518628210144499, -4.944772684328680334 ) ) ;
#18250 = CARTESIAN_POINT ( 'NONE',  ( 10.56230152254411259, 3.464101615137757051, -7.237500000000056666 ) ) ;
#18251 = VERTEX_POINT ( 'NONE', #26947 ) ;
#18252 = CARTESIAN_POINT ( 'NONE',  ( 13.49999999999999645, 197.7125000012290172, -23.38268590217984766 ) ) ;
#18253 = CARTESIAN_POINT ( 'NONE',  ( -15.46528703574804986, 123.3976862821014606, -3.257655550457287497 ) ) ;
#18254 = SURFACE_STYLE_FILL_AREA ( #15215 ) ;
#18255 = CARTESIAN_POINT ( 'NONE',  ( -5.233372021372430183, 4.947686282101431132, -8.152565276336710909 ) ) ;
#18256 = CARTESIAN_POINT ( 'NONE',  ( -27.24356964374999990, 197.5156250006145626, -15.72908226750537786 ) ) ;
#18257 = CARTESIAN_POINT ( 'NONE',  ( -55.52725981217218276, 242.6196170348268879, -0.4999999999999978351 ) ) ;
#18258 = CARTESIAN_POINT ( 'NONE',  ( 17.00000000000002132, -2.343145750507694913, 50.17464377163449285 ) ) ;
#18259 = CARTESIAN_POINT ( 'NONE',  ( -27.00000000000000355, 200.0000000000000000, 0.000000000000000000 ) ) ;
#18260 = CARTESIAN_POINT ( 'NONE',  ( 6.000769315822030740E-16, -20.00000000000000000, -4.899999999999999467 ) ) ;
#18261 = CARTESIAN_POINT ( 'NONE',  ( 9.500000000000005329, 66.28981371789855359, -0.1745138560723090149 ) ) ;
#18262 = DIRECTION ( 'NONE',  ( -0.000000000000000000, -1.000000000000000000, -0.000000000000000000 ) ) ;
#18263 = ORIENTED_EDGE ( 'NONE', *, *, #28378, .T. ) ;
#18264 = CARTESIAN_POINT ( 'NONE',  ( 18.00000000000000000, 244.5812500012290513, -5.196152422706630247 ) ) ;
#18265 = CARTESIAN_POINT ( 'NONE',  ( 7.228626920338837358, 76.92731371789857064, 10.49813415416005036 ) ) ;
#18266 = CARTESIAN_POINT ( 'NONE',  ( 22.80587116629412137, 7.646167579472024665E-16, -4.471874999385533123 ) ) ;
#18267 = CARTESIAN_POINT ( 'NONE',  ( -13.62178482187498396, 199.4281250006145569, 23.59362340125808188 ) ) ;
#18268 = CARTESIAN_POINT ( 'NONE',  ( 21.00000000000000000, 6.646953231504538984, -3.515624999385498217 ) ) ;
#18269 = CARTESIAN_POINT ( 'NONE',  ( 2.660918448318002838, 40.70231371789854791, 12.46528703574811558 ) ) ;
#18270 = CARTESIAN_POINT ( 'NONE',  ( -27.24356964374999990, 198.4718750006145171, -15.72908226750537786 ) ) ;
#18271 = VERTEX_POINT ( 'NONE', #7246 ) ;
#18272 =( BOUNDED_CURVE ( )  B_SPLINE_CURVE ( 2, ( #19506, #31052, #31232, #5074, #34259, #17763, #17019 ),
 .UNSPECIFIED., .F., .F. ) 
 B_SPLINE_CURVE_WITH_KNOTS ( ( 3, 2, 2, 3 ),
 ( 0.5652173913043473386, 0.5724637681159415736, 0.5797101449275359197, 0.5869565217391301548 ),
 .UNSPECIFIED. ) 
 CURVE ( )  GEOMETRIC_REPRESENTATION_ITEM ( )  RATIONAL_B_SPLINE_CURVE ( ( 1.000000000000008216, 0.8660254037844304920, 1.000000000000000000, 0.8660254037844387076, 1.000000000000000000, 0.8660254037844448138, 0.9999999999999938938 ) ) 
 REPRESENTATION_ITEM ( '' )  );
#18273 = EDGE_LOOP ( 'NONE', ( #17507, #19442 ) ) ;
#18274 = CARTESIAN_POINT ( 'NONE',  ( 15.24356964375000167, -3.323476615752272600, -5.503124999385465621 ) ) ;
#18275 = CARTESIAN_POINT ( 'NONE',  ( 21.00000000000000000, 244.6843750006144944, -6.646953231504538984 ) ) ;
#18276 = CARTESIAN_POINT ( 'NONE',  ( -12.50000000000000355, 21.91018628210143859, -0.1745138560725492671 ) ) ;
#18277 = CARTESIAN_POINT ( 'NONE',  ( -31.98586230271182984, 206.8500491399821328, 5.686928522499748340 ) ) ;
#18278 = CARTESIAN_POINT ( 'NONE',  ( 10.31873187879411091, 3.604726614523236616, -1.528124999385497729 ) ) ;
#18279 = CARTESIAN_POINT ( 'NONE',  ( -62.06919563604516554, 216.5000000000000000, -0.1155267958017906493 ) ) ;
#18280 = FACE_BOUND ( 'NONE', #34728, .T. ) ;
#18281 = CARTESIAN_POINT ( 'NONE',  ( 7.228626920338837358, 86.12731371789855928, 10.49813415416005036 ) ) ;
#18282 = EDGE_CURVE ( 'NONE', #35202, #22557, #23120, .T. ) ;
#18283 = CARTESIAN_POINT ( 'NONE',  ( -51.38913769728824121, 207.8500491399821613, -3.954877714930864485 ) ) ;
#18285 = ADVANCED_FACE ( 'NONE', ( #18820 ), #12930, .F. ) ;
#18284 = CARTESIAN_POINT ( 'NONE',  ( -69.99330436395490551, 210.1155267958017134, -6.500000000000000888 ) ) ;
#18286 = CARTESIAN_POINT ( 'NONE',  ( 15.24356964375000167, -3.323476615752272600, -6.515624999385480010 ) ) ;
#18287 = CARTESIAN_POINT ( 'NONE',  ( 23.99999999999999645, 5.196152422706631135, -2.400000000000013234 ) ) ;
#18288 = CARTESIAN_POINT ( 'NONE',  ( 13.04141134922778988, 65.42731371789857064, -8.927990412390371944 ) ) ;
#18289 = CARTESIAN_POINT ( 'NONE',  ( -42.47544563604517265, 216.3070033484980854, 6.137860380172893926 ) ) ;
#18290 = VECTOR ( 'NONE', #17364, 1000.000000000000000 ) ;
#18291 = CARTESIAN_POINT ( 'NONE',  ( 36.83775103377001869, 7.347880794884117764E-16, 162.1840432000934129 ) ) ;
#18292 = CARTESIAN_POINT ( 'NONE',  ( 12.53471296425194836, 90.62268628210146915, -2.311890736173178418 ) ) ;
#18293 = CARTESIAN_POINT ( 'NONE',  ( 3.257655550457285720, 24.49768628210144072, -15.46528703574804986 ) ) ;
#18295 = ADVANCED_FACE ( 'NONE', ( #18248 ), #15209, .T. ) ;
#18294 = CARTESIAN_POINT ( 'NONE',  ( 20.99999999999998579, 248.3124999999999716, 5.999999999999998224 ) ) ;
#18296 = DIRECTION ( 'NONE',  ( -0.000000000000000000, -0.000000000000000000, -1.000000000000000000 ) ) ;
#18297 = B_SPLINE_CURVE_WITH_KNOTS ( 'NONE', 3,
 ( #34109, #10990, #33371, #8161, #4741, #14028, #33559, #22006 ),
 .UNSPECIFIED., .F., .F.,
 ( 4, 2, 2, 4 ),
 ( 0.000000000000000000, 0.001245943103805707310, 0.002491886207611414619, 0.004983772415222829238 ),
 .UNSPECIFIED. ) ;
#18298 = CARTESIAN_POINT ( 'NONE',  ( -10.83675517735155047, 50.66018628210144925, -11.08355503943142750 ) ) ;
#18299 = CARTESIAN_POINT ( 'NONE',  ( -27.24356964375000345, 197.5531250006145285, 0.000000000000000000 ) ) ;
#18300 = CARTESIAN_POINT ( 'NONE',  ( 19.56230152254411081, -5.196152422706629359, -0.6374999987710516791 ) ) ;
#18301 = CARTESIAN_POINT ( 'NONE',  ( 20.99999999999999645, 185.0294372515228645, 0.000000000000000000 ) ) ;
#18302 = CARTESIAN_POINT ( 'NONE',  ( -32.58705436395489841, 205.3262412349647263, -4.842901733360204020 ) ) ;
#18303 = DIRECTION ( 'NONE',  ( -0.5887012860850802110, 0.8083506638593009885, 0.000000000000000000 ) ) ;
#18304 = CARTESIAN_POINT ( 'NONE',  ( -12.53471296425194836, 12.42268628210144321, 2.311890736173176641 ) ) ;
#18305 = CARTESIAN_POINT ( 'NONE',  ( 18.12178482187499640, 249.7843750006145456, -4.985214923628404904 ) ) ;
#18306 = CARTESIAN_POINT ( 'NONE',  ( -3.474262827703527901, 124.3648137178985849, 8.843639120294245259 ) ) ;
#18307 = CARTESIAN_POINT ( 'NONE',  ( 20.99999999999999645, 246.5968750006145456, -6.646953231504538984 ) ) ;
#18308 = ORIENTED_EDGE ( 'NONE', *, *, #34950, .T. ) ;
#18309 = CARTESIAN_POINT ( 'NONE',  ( 23.99999999999999645, 5.196152422706631135, -6.450000000000011724 ) ) ;
#18310 =( BOUNDED_CURVE ( )  B_SPLINE_CURVE ( 2, ( #24906, #37016, #19802, #22818, #10686, #8410, #31161 ),
 .UNSPECIFIED., .F., .F. ) 
 B_SPLINE_CURVE_WITH_KNOTS ( ( 3, 2, 2, 3 ),
 ( 0.4782608695652184050, 0.4855072463768126956, 0.4927536231884070417, 0.5000000000000013323 ),
 .UNSPECIFIED. ) 
 CURVE ( )  GEOMETRIC_REPRESENTATION_ITEM ( )  RATIONAL_B_SPLINE_CURVE ( ( 0.9999999999999815703, 0.8660254037844571373, 1.000000000000000000, 0.8660254037844387076, 1.000000000000000000, 0.8660254037844140607, 1.000000000000024647 ) ) 
 REPRESENTATION_ITEM ( '' )  );
#18311 = CYLINDRICAL_SURFACE ( 'NONE', #18411, 27.00000000000000355 ) ;
#18312 = CARTESIAN_POINT ( 'NONE',  ( -8.715434833792127023, 134.1398137178985621, 8.962234695871568846 ) ) ;
#18313 = CARTESIAN_POINT ( 'NONE',  ( 19.68408634441910365, -5.407089921784855591, -6.290624999385540761 ) ) ;
#18314 = CARTESIAN_POINT ( 'NONE',  ( 31.20130732697009535, 7.209453229046475009, 166.6014763038195383 ) ) ;
#18315 = DIRECTION ( 'NONE',  ( 1.000000000000000000, 0.000000000000000000, 0.000000000000000000 ) ) ;
#18316 = CARTESIAN_POINT ( 'NONE',  ( -11.18916359670908989, 217.4947517841555680, 4.100269900002030177 ) ) ;
#18317 = CARTESIAN_POINT ( 'NONE',  ( 4.944772684328679446, 43.18518628210144072, -11.48171059495397373 ) ) ;
#18318 = ORIENTED_EDGE ( 'NONE', *, *, #23982, .T. ) ;
#18319 = ORIENTED_EDGE ( 'NONE', *, *, #28562, .F. ) ;
#18320 = CARTESIAN_POINT ( 'NONE',  ( -27.00000000000000355, 195.9500000000000171, 0.000000000000000000 ) ) ;
#18321 = CARTESIAN_POINT ( 'NONE',  ( 20.99999999999997513, 244.9937500012290457, -5.999999999999999112 ) ) ;
#18322 = CARTESIAN_POINT ( 'NONE',  ( 19.39230484541326049, 248.1075961894323711, -5.999999999999994671 ) ) ;
#18323 = CARTESIAN_POINT ( 'NONE',  ( 15.24356964375000167, -3.323476615752272600, -8.653124999385468641 ) ) ;
#18324 = CARTESIAN_POINT ( 'NONE',  ( -10.49813415415989581, 87.17268628210143788, -7.228626920339068285 ) ) ;
#18325 = CARTESIAN_POINT ( 'NONE',  ( -10.83675517735179028, 23.73981371789854222, 11.08355503943118947 ) ) ;
#18326 = CARTESIAN_POINT ( 'NONE',  ( 24.00000000000000000, 243.4562500012290513, 5.196152422706629359 ) ) ;
#18327 = CARTESIAN_POINT ( 'NONE',  ( 18.90563079128947166, 210.7853884532676432, 5.961323472697788617 ) ) ;
#18328 = CARTESIAN_POINT ( 'NONE',  ( -64.04836230271183695, 206.0451222850691977, -2.149950860017851184 ) ) ;
#18329 = CYLINDRICAL_SURFACE ( 'NONE', #1668, 27.00000000000000000 ) ;
#18330 = CARTESIAN_POINT ( 'NONE',  ( 25.29522554115172639, 0.000000000000000000, 167.9369320615487311 ) ) ;
#18331 = CARTESIAN_POINT ( 'NONE',  ( -2.064181346179062349, 8.502313717898553946, -9.465287035748106703 ) ) ;
#18332 = CARTESIAN_POINT ( 'NONE',  ( -49.60788769728823411, 216.4690446883607535, 1.857196546604031662 ) ) ;
#18333 = CARTESIAN_POINT ( 'NONE',  ( -69.99330436395489130, 210.1155267958016850, -8.500000000000003553 ) ) ;
#18334 = CARTESIAN_POINT ( 'NONE',  ( 22.60769515458672529, 247.1674038105676630, -6.000000000000004441 ) ) ;
#18335 = CARTESIAN_POINT ( 'NONE',  ( 13.62178482187501416, 199.0531250006145285, 23.59362340125806767 ) ) ;
#18336 = CARTESIAN_POINT ( 'NONE',  ( 14.38691631536194393, 112.8648137178985564, 5.770363421894124656 ) ) ;
#18337 = CARTESIAN_POINT ( 'NONE',  ( -60.48586230271183695, 206.8500491399821328, 5.686928522499748340 ) ) ;
#18338 = EDGE_LOOP ( 'NONE', ( #33881, #31312, #21491, #11680 ) ) ;
#18339 = CARTESIAN_POINT ( 'NONE',  ( -10.49813415415989581, 31.97268628210143859, -7.228626920339068285 ) ) ;
#18340 = CARTESIAN_POINT ( 'NONE',  ( -4.500000000000002665, 227.3990362376858627, -2.500000000000000000 ) ) ;
#18341 = VECTOR ( 'NONE', #36761, 1000.000000000000000 ) ;
#18342 = FACE_OUTER_BOUND ( 'NONE', #33834, .T. ) ;
#18343 = CARTESIAN_POINT ( 'NONE',  ( 25.10405911393864642, 0.000000000000000000, 168.5465380477087933 ) ) ;
#18344 = CARTESIAN_POINT ( 'NONE',  ( 3.257655550457285720, 98.09768628210146346, -15.46528703574804986 ) ) ;
#18345 =( NAMED_UNIT ( * ) PLANE_ANGLE_UNIT ( ) SI_UNIT ( $, .RADIAN. ) );
#18346 = CARTESIAN_POINT ( 'NONE',  ( 10.31873187879411091, 3.604726614523236616, -3.328124999385545291 ) ) ;
#18347 = CARTESIAN_POINT ( 'NONE',  ( -5.233372021372430183, 50.94768628210145067, -8.152565276336710909 ) ) ;
#18348 = FACE_OUTER_BOUND ( 'NONE', #37258, .T. ) ;
#18349 = CARTESIAN_POINT ( 'NONE',  ( -32.19122103062156270, 207.8379586601371329, -8.530955311639223382 ) ) ;
#18350 = PLANE ( 'NONE',  #18947 ) ;
#18351 = CARTESIAN_POINT ( 'NONE',  ( -12.53471296425194836, 76.82268628210145778, 2.311890736173176641 ) ) ;
#18352 = LINE ( 'NONE', #1085, #16684 ) ;
#18353 = FACE_OUTER_BOUND ( 'NONE', #299, .T. ) ;
#18355 = DIRECTION ( 'NONE',  ( -0.000000000000000000, 1.000000000000000000, -0.000000000000000000 ) ) ;
#18354 = CARTESIAN_POINT ( 'NONE',  ( -9.500000000000005329, 49.51018628210145067, -0.1745138560725176813 ) ) ;
#18356 = CARTESIAN_POINT ( 'NONE',  ( 20.99999999999997868, 244.7687500012290513, 5.999999999999999112 ) ) ;
#18357 = CARTESIAN_POINT ( 'NONE',  ( 26.75643035624999655, 3.323476615752271712, -9.328124999385446259 ) ) ;
#18358 = DIRECTION ( 'NONE',  ( 0.000000000000000000, 1.000000000000000000, 0.000000000000000000 ) ) ;
#18359 = CARTESIAN_POINT ( 'NONE',  ( 28.01132750018552287, 5.407089921784862696, 165.9583038997966185 ) ) ;
#18360 = CARTESIAN_POINT ( 'NONE',  ( 30.93902301358532014, 6.928203230275514990, 163.6035528836375192 ) ) ;
#18361 = CARTESIAN_POINT ( 'NONE',  ( 15.00000000000000000, 245.9499999999999886, 0.000000000000000000 ) ) ;
#18362 = VECTOR ( 'NONE', #19702, 1000.000000000000000 ) ;
#18363 = CARTESIAN_POINT ( 'NONE',  ( 5.778771075727756162E-15, 195.4156250006145399, 31.45816453501076637 ) ) ;
#18364 = CARTESIAN_POINT ( 'NONE',  ( 4.622313124798831829, 110.5648137178985593, -11.61527771782809282 ) ) ;
#18365 = CARTESIAN_POINT ( 'NONE',  ( -8.962234695871760692, 112.7601862821014720, 8.715434833791933400 ) ) ;
#18366 = ORIENTED_EDGE ( 'NONE', *, *, #9372, .T. ) ;
#18367 = ORIENTED_EDGE ( 'NONE', *, *, #7373, .T. ) ;
#18368 = CARTESIAN_POINT ( 'NONE',  ( -13.62178482187498396, 195.3781250006145171, 23.59362340125808188 ) ) ;
#18369 = DIRECTION ( 'NONE',  ( 0.08715574274765150453, 0.000000000000000000, 0.9961946980917461003 ) ) ;
#18370 = CARTESIAN_POINT ( 'NONE',  ( 8.632099005475788900, 74.05231371789854222, -13.23911966647199812 ) ) ;
#18371 = CARTESIAN_POINT ( 'NONE',  ( 15.24356964374999990, 3.323476615752268604, -6.140624999385478233 ) ) ;
#18372 = CARTESIAN_POINT ( 'NONE',  ( 26.75643035624999655, 245.6218750006145513, -3.323476615752271712 ) ) ;
#18373 = CARTESIAN_POINT ( 'NONE',  ( 7.954856959092191815, 100.9726862821014635, 5.529263428287477744 ) ) ;
#18374 = VECTOR ( 'NONE', #16378, 1000.000000000000000 ) ;
#18375 = CARTESIAN_POINT ( 'NONE',  ( -27.00000000000000355, 194.6888594429640591, -9.827195528215911580 ) ) ;
#18376 = CARTESIAN_POINT ( 'NONE',  ( -8.843639120294245259, 53.06481371789855928, -3.474262827703533230 ) ) ;
#18377 = CARTESIAN_POINT ( 'NONE',  ( 10.31873187879410914, 0.000000000000000000, -5.540624999385540761 ) ) ;
#18378 = CARTESIAN_POINT ( 'NONE',  ( 3.796722387233182339, 114.0148137178985763, 8.710071997420207879 ) ) ;
#18379 = CARTESIAN_POINT ( 'NONE',  ( 18.12178482187500350, 240.3718750006145228, 4.985214923628407568 ) ) ;
#18380 = CARTESIAN_POINT ( 'NONE',  ( 11.61527771782809637, 30.06481371789855572, 4.622313124798827388 ) ) ;
#18381 =( GEOMETRIC_REPRESENTATION_CONTEXT ( 3 ) GLOBAL_UNCERTAINTY_ASSIGNED_CONTEXT ( ( #12742 ) ) GLOBAL_UNIT_ASSIGNED_CONTEXT ( ( #3858, #20942, #12014 ) ) REPRESENTATION_CONTEXT ( 'NONE', 'WORKASPACE' ) );
#18382 = DIRECTION ( 'NONE',  ( 0.000000000000000000, 0.000000000000000000, 1.000000000000000000 ) ) ;
#18383 = CARTESIAN_POINT ( 'NONE',  ( 4.944772684328679446, 79.98518628210145209, -11.48171059495397373 ) ) ;
#18384 = CARTESIAN_POINT ( 'NONE',  ( 13.56230152254410370, 5.196152422706630247, -5.362499998771003362 ) ) ;
#18385 = DIRECTION ( 'NONE',  ( 0.000000000000000000, 0.000000000000000000, 1.000000000000000000 ) ) ;
#18386 = CARTESIAN_POINT ( 'NONE',  ( 34.15106413780644345, 5.407089921784857367, 164.4988870712271023 ) ) ;
#18387 = CARTESIAN_POINT ( 'NONE',  ( 6.092822981423978490, 79.98518628210145209, -14.25334919248782306 ) ) ;
#18388 = CARTESIAN_POINT ( 'NONE',  ( 13.44051670066910731, 5.407089921784862696, -5.221874999385534011 ) ) ;
#18389 = SURFACE_STYLE_FILL_AREA ( #32965 ) ;
#18390 = CARTESIAN_POINT ( 'NONE',  ( -89.83814373643217266, 60.44923248139874516, 5.000000000000000000 ) ) ;
#18391 = CARTESIAN_POINT ( 'NONE',  ( -13.50000000000000533, 199.0250000000000057, -23.38268590217984411 ) ) ;
#18392 = CARTESIAN_POINT ( 'NONE',  ( -9.534712964251941258, 113.6226862821014549, 1.715153634034234154 ) ) ;
#18393 = DIRECTION ( 'NONE',  ( 0.000000000000000000, 0.000000000000000000, 1.000000000000000000 ) ) ;
#18394 = CARTESIAN_POINT ( 'NONE',  ( 8.962234695871762469, 135.7601862821014720, -8.715434833791931624 ) ) ;
#18395 = VECTOR ( 'NONE', #14841, 1000.000000000000000 ) ;
#18396 = CYLINDRICAL_SURFACE ( 'NONE', #31782, 5.999999999999998224 ) ;
#18397 = CARTESIAN_POINT ( 'NONE',  ( 26.75643035624999655, 240.5218750006145001, -7.049594010296217766E-16 ) ) ;
#18398 = ORIENTED_EDGE ( 'NONE', *, *, #8236, .T. ) ;
#18399 = CARTESIAN_POINT ( 'NONE',  ( 24.95208128752243226, 0.000000000000000000, 166.8094235429113041 ) ) ;
#18400 = CARTESIAN_POINT ( 'NONE',  ( 21.00000000000000000, -6.646953231504538984, -1.828124999385473792 ) ) ;
#18401 = DIRECTION ( 'NONE',  ( 0.2588190451025212391, 3.169619151431769872E-17, -0.9659258262890682012 ) ) ;
#18402 = CARTESIAN_POINT ( 'NONE',  ( 14.99999999999965539, 3.464101615137553658, -3.637499999999990852 ) ) ;
#18403 = DIRECTION ( 'NONE',  ( -0.000000000000000000, 1.000000000000000000, -0.000000000000000000 ) ) ;
#18404 = CYLINDRICAL_SURFACE ( 'NONE', #4724, 27.00000000000000000 ) ;
#18405 = EDGE_CURVE ( 'NONE', #27793, #33064, #36314, .T. ) ;
#18406 = CARTESIAN_POINT ( 'NONE',  ( -20.74539548491456031, 194.7088513915494445, -17.40745275905709377 ) ) ;
#18407 = CARTESIAN_POINT ( 'NONE',  ( 2.064181346179061460, 22.30231371789854933, 9.465287035748106703 ) ) ;
#18408 = CARTESIAN_POINT ( 'NONE',  ( 27.24356964375000700, 196.8968750006144717, 15.72908226750537075 ) ) ;
#18410 = ORIENTED_EDGE ( 'NONE', *, *, #3630, .T. ) ;
#18409 = ORIENTED_EDGE ( 'NONE', *, *, #4833, .T. ) ;
#18411 = AXIS2_PLACEMENT_3D ( 'NONE', #3887, #27012, #1039 ) ;
#18412 = COLOUR_RGB ( '',0.8941176470588234615, 0.8941176470588234615, 0.8941176470588234615 ) ;
#18413 = CARTESIAN_POINT ( 'NONE',  ( 26.75643035624999655, 245.9593750006145001, -3.323476615752271712 ) ) ;
#18414 = CARTESIAN_POINT ( 'NONE',  ( -4.944772684328424539, 17.41481371789854649, -11.48171059495408031 ) ) ;
#18415 = CARTESIAN_POINT ( 'NONE',  ( 26.75643035624999655, 3.323476615752271712, -0.7781249993854945091 ) ) ;
#18416 = CARTESIAN_POINT ( 'NONE',  ( 0.1745138560722461762, 123.7898137178985678, 15.50000000000000533 ) ) ;
#18417 = VECTOR ( 'NONE', #33867, 1000.000000000000000 ) ;
#18418 = CARTESIAN_POINT ( 'NONE',  ( 26.99999999999999645, 3.464101615137755275, -10.03124999877094581 ) ) ;
#18419 = EDGE_CURVE ( 'NONE', #4550, #22630, #13299, .T. ) ;
#18420 = DIRECTION ( 'NONE',  ( 1.000000000000000000, 0.000000000000000000, 0.000000000000000000 ) ) ;
#18421 = ORIENTED_EDGE ( 'NONE', *, *, #29074, .F. ) ;
#18422 = CARTESIAN_POINT ( 'NONE',  ( 10.31873187879410736, -3.604726614523244610, -6.459374999385468996 ) ) ;
#18423 = CARTESIAN_POINT ( 'NONE',  ( 5.778771075727756162E-15, 195.4156250006145399, 31.45816453501075927 ) ) ;
#18424 = CARTESIAN_POINT ( 'NONE',  ( 7.228626920339068285, 126.2726862821014606, -10.49813415415989581 ) ) ;
#18425 = CARTESIAN_POINT ( 'NONE',  ( 27.90674060888834518, -5.407089921784865361, 164.7628702620865226 ) ) ;
#18426 = EDGE_CURVE ( 'NONE', #5428, #55, #30865, .T. ) ;
#18427 = CARTESIAN_POINT ( 'NONE',  ( -57.51711230271184405, 218.4690446883607535, -2.393094931466363651 ) ) ;
#18428 = CARTESIAN_POINT ( 'NONE',  ( 26.75643035624999655, 246.3343750006145285, 3.323476615752267271 ) ) ;
#18429 = FILL_AREA_STYLE_COLOUR ( '', #8710 ) ;
#18430 = EDGE_CURVE ( 'NONE', #5908, #26373, #34714, .T. ) ;
#18431 = CARTESIAN_POINT ( 'NONE',  ( 10.56230152254209642, -3.464101615136592649, -9.749999998771011533 ) ) ;
#18432 = CARTESIAN_POINT ( 'NONE',  ( -42.67336230271183695, 213.9548777149308023, 2.149950860017852960 ) ) ;
#18433 = CARTESIAN_POINT ( 'NONE',  ( 8.715434833791931624, 138.0601862821014549, 8.962234695871760692 ) ) ;
#18434 = CARTESIAN_POINT ( 'NONE',  ( 31.27974749544297595, 7.209453229046475009, 167.4980515321021244 ) ) ;
#18435 = VERTEX_POINT ( 'NONE', #19559 ) ;
#18436 = CARTESIAN_POINT ( 'NONE',  ( 15.00000000000000000, 248.6125000000000114, -3.464101615137752610 ) ) ;
#18437 = CARTESIAN_POINT ( 'NONE',  ( -6.092822981423970496, 139.7851862821014493, 14.25334919248782661 ) ) ;
#18438 = AXIS2_PLACEMENT_3D ( 'NONE', #22264, #31521, #5181 ) ;
#18439 = CARTESIAN_POINT ( 'NONE',  ( -44.26413769728823411, 214.1499508600179240, 7.418979330068584233 ) ) ;
#18440 = CARTESIAN_POINT ( 'NONE',  ( 3.474262827703335166, 120.2351862821014521, 8.843639120294326972 ) ) ;
#18441 = AXIS2_PLACEMENT_3D ( 'NONE', #3992, #21453, #21266 ) ;
#18442 = CARTESIAN_POINT ( 'NONE',  ( 8.715434833791931624, 36.86018628210144499, 8.962234695871760692 ) ) ;
#18443 = CARTESIAN_POINT ( 'NONE',  ( 10.56230152254410726, 0.000000000000000000, -7.650000000000045652 ) ) ;
#18444 = UNCERTAINTY_MEASURE_WITH_UNIT (LENGTH_MEASURE( 1.000000000000000082E-05 ), #20330, 'distance_accuracy_value', 'NONE');
#18445 = ORIENTED_EDGE ( 'NONE', *, *, #16584, .T. ) ;
#18446 = FILL_AREA_STYLE_COLOUR ( '', #13702 ) ;
#18447 = CARTESIAN_POINT ( 'NONE',  ( 3.257655550457285720, 116.4976862821014549, -15.46528703574804986 ) ) ;
#18448 = CARTESIAN_POINT ( 'NONE',  ( 21.00000000000000355, 0.000000000000000000, 50.00000000000001421 ) ) ;
#18449 = CARTESIAN_POINT ( 'NONE',  ( 6.594114490232462877, 138.7398137178985564, -6.840914352311949109 ) ) ;
#18450 = CARTESIAN_POINT ( 'NONE',  ( -1.926257025242585782E-15, 197.8906250006145342, -31.45816453501075927 ) ) ;
#18451 = DIRECTION ( 'NONE',  ( -0.000000000000000000, -0.000000000000000000, 1.000000000000000000 ) ) ;
#18452 = CARTESIAN_POINT ( 'NONE',  ( 13.49999999999999645, 195.3500000000000227, -23.38268590217984766 ) ) ;
#18453 = CARTESIAN_POINT ( 'NONE',  ( 22.56230152254476451, 3.464101615137376022, -1.424999998770992038 ) ) ;
#18454 = CARTESIAN_POINT ( 'NONE',  ( 18.20792125986140064, 5.080248635121038525, -7.999999999999994671 ) ) ;
#18455 = CARTESIAN_POINT ( 'NONE',  ( -50.22894823740647041, 235.3444610600932094, 2.500000000000000000 ) ) ;
#18456 = CARTESIAN_POINT ( 'NONE',  ( -7.954856959092309943, 79.22731371789853938, 5.529263428287300108 ) ) ;
#18457 = CARTESIAN_POINT ( 'NONE',  ( 0.000000000000000000, 210.0000000000000284, 0.000000000000000000 ) ) ;
#18458 = ORIENTED_EDGE ( 'NONE', *, *, #16987, .F. ) ;
#18459 = CARTESIAN_POINT ( 'NONE',  ( 15.00000000000000000, 242.8562500012290286, 0.000000000000000000 ) ) ;
#18460 = CARTESIAN_POINT ( 'NONE',  ( 11.61527771782809637, 85.26481371789856212, 4.622313124798827388 ) ) ;
#18461 = EDGE_CURVE ( 'NONE', #23355, #14430, #30895, .T. ) ;
#18462 = CARTESIAN_POINT ( 'NONE',  ( 16.56230152254411436, -7.209453229046482114, -3.684374999385500615 ) ) ;
#18463 = DIRECTION ( 'NONE',  ( -0.1155267958017757585, -0.9933043639548629899, 1.378486719154166141E-14 ) ) ;
#18464 = CARTESIAN_POINT ( 'NONE',  ( 21.00000000000000000, 6.646953231504538984, -4.415624999385457272 ) ) ;
#18465 = CARTESIAN_POINT ( 'NONE',  ( 6.932735513424201024, 55.65231371789855785, -10.69584247140429412 ) ) ;
#18466 = EDGE_CURVE ( 'NONE', #36062, #5775, #27857, .T. ) ;
#18467 = VERTEX_POINT ( 'NONE', #19381 ) ;
#18468 = CARTESIAN_POINT ( 'NONE',  ( 20.99999999999999645, -6.646953231504538984, -7.678124999385482319 ) ) ;
#18469 = CARTESIAN_POINT ( 'NONE',  ( 21.00000000000000000, 244.9093750006145456, 6.646953231504538984 ) ) ;
#18470 = CARTESIAN_POINT ( 'NONE',  ( 10.69584247140445221, 16.44768628210144001, -6.932735513423970097 ) ) ;
#18471 = ADVANCED_FACE ( 'NONE', ( #34128 ), #33579, .F. ) ;
#18472 = CARTESIAN_POINT ( 'NONE',  ( -40.29836230271182984, 204.3130714775002446, -3.149950860017828091 ) ) ;
#18473 = CARTESIAN_POINT ( 'NONE',  ( -51.18377896937847993, 208.3738570449995109, 6.530955311639247363 ) ) ;
#18474 = SURFACE_STYLE_FILL_AREA ( #32852 ) ;
#18475 = CARTESIAN_POINT ( 'NONE',  ( 33.62038311478219299, 5.196152422706631135, 159.8304993458455385 ) ) ;
#18476 = CARTESIAN_POINT ( 'NONE',  ( -0.1745138560722763466, 82.38981371789854791, -12.50000000000000355 ) ) ;
#18477 = CARTESIAN_POINT ( 'NONE',  ( -47.82663769728823411, 206.0451222850691408, 2.149950860017832532 ) ) ;
#18478 =( BOUNDED_CURVE ( )  B_SPLINE_CURVE ( 2, ( #33603, #1189, #7643, #19219, #15427, #26976, #27166 ),
 .UNSPECIFIED., .F., .F. ) 
 B_SPLINE_CURVE_WITH_KNOTS ( ( 3, 2, 2, 3 ),
 ( 0.4565217391304338679, 0.4637681159420281585, 0.4710144927536223936, 0.4782608695652166841 ),
 .UNSPECIFIED. ) 
 CURVE ( )  GEOMETRIC_REPRESENTATION_ITEM ( )  RATIONAL_B_SPLINE_CURVE ( ( 1.000000000000016431, 0.8660254037844222763, 1.000000000000000000, 0.8660254037844387076, 1.000000000000000000, 0.8660254037844520303, 0.9999999999999866773 ) ) 
 REPRESENTATION_ITEM ( '' )  );
#18479 = CARTESIAN_POINT ( 'NONE',  ( -34.76413769728823411, 214.1499508600179240, 7.418979330068584233 ) ) ;
#18480 = CARTESIAN_POINT ( 'NONE',  ( 26.75643035624999655, -3.323476615752267271, -5.915624999385464378 ) ) ;
#18481 = CARTESIAN_POINT ( 'NONE',  ( 13.56230152254410548, 5.196152422706636465, -7.275000000000058975 ) ) ;
#18482 = CARTESIAN_POINT ( 'NONE',  ( 13.23911966647199812, 67.15231371789852233, 8.632099005475788900 ) ) ;
#18483 = CARTESIAN_POINT ( 'NONE',  ( -48.01711230271184405, 218.4690446883607535, -2.393094931466363651 ) ) ;
#18484 = CARTESIAN_POINT ( 'NONE',  ( 7.234628195640312676, 199.8674038105676800, -27.00000000000000711 ) ) ;
#18485 = CARTESIAN_POINT ( 'NONE',  ( -4.944772684328673229, 93.78518628210144925, 11.48171059495397728 ) ) ;
#18486 = CARTESIAN_POINT ( 'NONE',  ( -6.092822981423970496, 29.38518628210144712, 14.25334919248782661 ) ) ;
#18487 = CARTESIAN_POINT ( 'NONE',  ( 22.56230152254411792, 7.347880794884125653E-16, -0.2250000000000584865 ) ) ;
#18488 = CARTESIAN_POINT ( 'NONE',  ( 29.48995970988985604, 6.148715791637015649, 159.4803054849043633 ) ) ;
#18489 = ORIENTED_EDGE ( 'NONE', *, *, #29560, .T. ) ;
#18490 = CARTESIAN_POINT ( 'NONE',  ( 5.770363421893814682, 55.83518628210145351, 14.38691631536207183 ) ) ;
#18491 = CARTESIAN_POINT ( 'NONE',  ( -27.24356964375000345, 198.4156250006145399, -15.72908226750537786 ) ) ;
#18492 = CARTESIAN_POINT ( 'NONE',  ( 27.24356964374999635, 199.6718750006145058, -15.72908226750539029 ) ) ;
#18493 = CARTESIAN_POINT ( 'NONE',  ( 15.00000000000000000, 0.000000000000000000, -1.799999999999996048 ) ) ;
#18494 = CARTESIAN_POINT ( 'NONE',  ( -32.19122103062156981, 208.3738570449993404, -6.530955311639226935 ) ) ;
#18495 = DIRECTION ( 'NONE',  ( 0.000000000000000000, 0.000000000000000000, -1.000000000000000000 ) ) ;
#18496 = CARTESIAN_POINT ( 'NONE',  ( -11.61527771782819940, 21.33518628210144641, 4.622313124798574258 ) ) ;
#18497 =( BOUNDED_CURVE ( )  B_SPLINE_CURVE ( 2, ( #8390, #22981, #28098, #8205, #5158, #19782, #25442 ),
 .UNSPECIFIED., .F., .F. ) 
 B_SPLINE_CURVE_WITH_KNOTS ( ( 3, 2, 2, 3 ),
 ( 0.8260869565217379140, 0.8333333333333329263, 0.8405797101449278275, 0.8478260869565228397 ),
 .UNSPECIFIED. ) 
 CURVE ( )  GEOMETRIC_REPRESENTATION_ITEM ( )  RATIONAL_B_SPLINE_CURVE ( ( 1.000000000000022649, 0.8660254037844161701, 1.000000000000000000, 0.8660254037844387076, 1.000000000000000000, 0.8660254037844181685, 1.000000000000020428 ) ) 
 REPRESENTATION_ITEM ( '' )  );
#18498 = LINE ( 'NONE', #16021, #22626 ) ;
#18499 = CARTESIAN_POINT ( 'NONE',  ( -6.594114490232462877, 134.1398137178985621, 6.840914352311949109 ) ) ;
#18500 = CARTESIAN_POINT ( 'NONE',  ( 26.75643035624999655, 243.7468750006145228, 3.323476615752267271 ) ) ;
#18501 = ORIENTED_EDGE ( 'NONE', *, *, #36268, .F. ) ;
#18502 = CARTESIAN_POINT ( 'NONE',  ( 15.00000000000000000, 0.000000000000000000, -6.750000000000006217 ) ) ;
#18503 = CARTESIAN_POINT ( 'NONE',  ( 15.00000000000000000, 245.1062500012290286, 0.000000000000000000 ) ) ;
#18504 = EDGE_CURVE ( 'NONE', #26034, #11516, #1520, .T. ) ;
#18505 = DIRECTION ( 'NONE',  ( -1.000000000000000000, 0.000000000000000000, 0.000000000000000000 ) ) ;
#18506 = CARTESIAN_POINT ( 'NONE',  ( 19.68408634441910721, -5.407089921784855591, -6.740624999385547156 ) ) ;
#18507 = CARTESIAN_POINT ( 'NONE',  ( 31.08364707426076023, 7.209453229046475009, 165.2566134613956876 ) ) ;
#18508 = CARTESIAN_POINT ( 'NONE',  ( 0.000000000000000000, 200.0000000000000000, 0.000000000000000000 ) ) ;
#18509 = CARTESIAN_POINT ( 'NONE',  ( -13.49999999999998401, 199.6250000000000284, 23.38268590217985476 ) ) ;
#18510 = VERTEX_POINT ( 'NONE', #25231 ) ;
#18511 = CARTESIAN_POINT ( 'NONE',  ( 0.1745138560725515708, 51.81018628210144783, -12.50000000000000355 ) ) ;
#18512 = VERTEX_POINT ( 'NONE', #30560 ) ;
#18513 = EDGE_LOOP ( 'NONE', ( #32193, #33166, #18086, #11598 ) ) ;
#18514 = CARTESIAN_POINT ( 'NONE',  ( 10.56230152254410903, 0.000000000000000000, -9.787499998771043153 ) ) ;
#18515 = CARTESIAN_POINT ( 'NONE',  ( 15.24356964374999990, 0.000000000000000000, -0.1406249993854691294 ) ) ;
#18516 = CARTESIAN_POINT ( 'NONE',  ( 27.00000000000058620, -3.464101615137410661, -1.162499999999995204 ) ) ;
#18517 = CARTESIAN_POINT ( 'NONE',  ( 18.00000000000000000, 248.1250000000000000, -5.196152422706630247 ) ) ;
#18518 = CARTESIAN_POINT ( 'NONE',  ( 15.24356964374999990, 0.000000000000000000, -9.590624999385454430 ) ) ;
#18519 = CARTESIAN_POINT ( 'NONE',  ( 2.311890736173175753, 74.52268628210146062, 12.53471296425194836 ) ) ;
#18520 = CARTESIAN_POINT ( 'NONE',  ( 6.092822981423662299, 22.01481371789855501, 14.25334919248795096 ) ) ;
#18521 = DIRECTION ( 'NONE',  ( 1.000000000000000000, 0.000000000000000000, 1.636531581110199847E-16 ) ) ;
#18522 = CARTESIAN_POINT ( 'NONE',  ( 8.278277990406262887, 214.7706457535967104, 3.659938751168453130 ) ) ;
#18523 = CARTESIAN_POINT ( 'NONE',  ( -61.47544563604516554, 213.3788001182224718, 3.209657149897419348 ) ) ;
#18524 = AXIS2_PLACEMENT_3D ( 'NONE', #25607, #36977, #31300 ) ;
#18525 = CYLINDRICAL_SURFACE ( 'NONE', #25257, 4.000000000000000888 ) ;
#18526 = CARTESIAN_POINT ( 'NONE',  ( 25.25273711656224407, 3.464101615137752166, 167.4512871462289922 ) ) ;
#18527 = CARTESIAN_POINT ( 'NONE',  ( 12.50000000000000355, 139.8898137178985621, -0.1745138560722771515 ) ) ;
#18528 = CARTESIAN_POINT ( 'NONE',  ( -52.37872103062156270, 203.4690446883607535, 1.626142955000567936 ) ) ;
#18529 = CARTESIAN_POINT ( 'NONE',  ( -64.84747103062156270, 214.3500491399821044, -7.303452534266878793 ) ) ;
#18530 =( REPRESENTATION_RELATIONSHIP ('NONE','NONE', #4304, #10836 ) REPRESENTATION_RELATIONSHIP_WITH_TRANSFORMATION ( #21557 )SHAPE_REPRESENTATION_RELATIONSHIP( ) );
#18531 = LINE ( 'NONE', #27409, #13711 ) ;
#18532 = CARTESIAN_POINT ( 'NONE',  ( -1.926257025242585782E-15, 199.6906250006145456, -31.45816453501075927 ) ) ;
#18533 = CARTESIAN_POINT ( 'NONE',  ( 10.83675517735179206, 111.1398137178985621, -11.08355503943118769 ) ) ;
#18534 = CARTESIAN_POINT ( 'NONE',  ( -39.50669563604517265, 209.8844732041982013, -6.500000000000000888 ) ) ;
#18535 = ORIENTED_EDGE ( 'NONE', *, *, #14038, .F. ) ;
#18536 = CARTESIAN_POINT ( 'NONE',  ( -4.622313124798576922, 32.83518628210143930, -11.61527771782819762 ) ) ;
#18537 = CARTESIAN_POINT ( 'NONE',  ( 33.72497000607938844, -5.196152422706629359, 161.0259329835556059 ) ) ;
#18538 = DIRECTION ( 'NONE',  ( 0.08715574274765150453, 0.000000000000000000, 0.9961946980917461003 ) ) ;
#18539 = CARTESIAN_POINT ( 'NONE',  ( 34.34226204845910502, 5.407089921784862696, 166.6842891901658845 ) ) ;
#18540 = CARTESIAN_POINT ( 'NONE',  ( -8.927990412390661490, 112.4726862821014635, 13.04141134922759804 ) ) ;
#18541 =( BOUNDED_CURVE ( )  B_SPLINE_CURVE ( 2, ( #13913, #17312, #14648, #14094, #25831, #37378, #22634 ),
 .UNSPECIFIED., .F., .F. ) 
 B_SPLINE_CURVE_WITH_KNOTS ( ( 3, 2, 2, 3 ),
 ( 0.5869565217391301548, 0.5942028985507243899, 0.6014492753623187360, 0.6086956521739130821 ),
 .UNSPECIFIED. ) 
 CURVE ( )  GEOMETRIC_REPRESENTATION_ITEM ( )  RATIONAL_B_SPLINE_CURVE ( ( 1.000000000000006217, 0.8660254037844326014, 1.000000000000000000, 0.8660254037844387076, 1.000000000000000000, 0.8660254037844387076, 1.000000000000000000 ) ) 
 REPRESENTATION_ITEM ( '' )  );
#18542 = CARTESIAN_POINT ( 'NONE',  ( -61.08705436395489841, 205.3262412349647548, -4.842901733360204908 ) ) ;
#18543 = CARTESIAN_POINT ( 'NONE',  ( 19.68408634441910365, -5.407089921784855591, -5.390624999385557281 ) ) ;
#18544 = CARTESIAN_POINT ( 'NONE',  ( 5.233372021372432847, 46.34768628210144925, 8.152565276336710909 ) ) ;
#18545 = ADVANCED_FACE ( 'NONE', ( #24670 ), #5130, .T. ) ;
#18546 = FACE_OUTER_BOUND ( 'NONE', #12515, .T. ) ;
#18547 = CARTESIAN_POINT ( 'NONE',  ( -39.51413769728823411, 214.1499508600179240, 7.418979330068584233 ) ) ;
#18548 = FACE_OUTER_BOUND ( 'NONE', #4308, .T. ) ;
#18549 = CARTESIAN_POINT ( 'NONE',  ( -4.944772684328673229, 75.38518628210144357, 11.48171059495397728 ) ) ;
#18550 = CARTESIAN_POINT ( 'NONE',  ( -1.909035429704832693E-15, 199.8875000000000171, -31.17691453623979214 ) ) ;
#18551 = CARTESIAN_POINT ( 'NONE',  ( 15.24356964374999990, 249.8593750006145342, 0.000000000000000000 ) ) ;
#18553 = CARTESIAN_POINT ( 'NONE',  ( 16.56230152254411436, 6.928203230275514990, -1.912500000000037836 ) ) ;
#18552 = CARTESIAN_POINT ( 'NONE',  ( -0.1745138560725182642, 38.01018628210144357, 9.500000000000005329 ) ) ;
#18554 = CARTESIAN_POINT ( 'NONE',  ( 24.36051168362275021, 3.604726614523236616, 160.0477520296135765 ) ) ;
#18555 = ORIENTED_EDGE ( 'NONE', *, *, #29307, .T. ) ;
#18556 = CARTESIAN_POINT ( 'NONE',  ( 15.24356964374999990, 0.000000000000000000, -10.04062499938546082 ) ) ;
#18557 = CARTESIAN_POINT ( 'NONE',  ( 24.63014976274829593, 3.604726614523240613, 163.1297293768349164 ) ) ;
#18558 = CARTESIAN_POINT ( 'NONE',  ( 24.81477950914817754, 0.000000000000000000, 162.4454087870936121 ) ) ;
#18559 = CARTESIAN_POINT ( 'NONE',  ( 23.99999999999999645, 247.1500000000000057, -5.196152422706631135 ) ) ;
#18560 = CARTESIAN_POINT ( 'NONE',  ( -27.24356964375000345, 196.2031250006145342, 0.000000000000000000 ) ) ;
#18561 = EDGE_CURVE ( 'NONE', #35079, #32003, #20903, .T. ) ;
#18562 = AXIS2_PLACEMENT_3D ( 'NONE', #23093, #13822, #19519 ) ;
#18563 = CARTESIAN_POINT ( 'NONE',  ( 11.61527771782809637, 94.46481371789855075, 4.622313124798827388 ) ) ;
#18564 = CARTESIAN_POINT ( 'NONE',  ( -10.69584247140444866, 113.0476862821014663, 6.932735513423972762 ) ) ;
#18565 = VERTEX_POINT ( 'NONE', #29175 ) ;
#18566 = VERTEX_POINT ( 'NONE', #31472 ) ;
#18567 = CARTESIAN_POINT ( 'NONE',  ( -27.24356964374999635, 194.8906250006145342, 15.72908226750539384 ) ) ;
#18568 = CARTESIAN_POINT ( 'NONE',  ( 26.75643035624999655, 240.9718750006145171, -7.049594010296217766E-16 ) ) ;
#18569 = CARTESIAN_POINT ( 'NONE',  ( 11.08355503943118769, 76.63981371789854791, 10.83675517735179028 ) ) ;
#18570 = CARTESIAN_POINT ( 'NONE',  ( 23.87821517812499650, 4.985214923628404904, -5.803124999385484095 ) ) ;
#18571 = CARTESIAN_POINT ( 'NONE',  ( 21.00000000000000000, 244.3468750006145171, -6.646953231504538984 ) ) ;
#18572 = CARTESIAN_POINT ( 'NONE',  ( 8.152565276336714462, 99.24768628210145494, -5.233372021372432847 ) ) ;
#18573 = VECTOR ( 'NONE', #14082, 1000.000000000000000 ) ;
#18574 = CARTESIAN_POINT ( 'NONE',  ( 15.26155779561005232, -6.106572496351636126, -10.00000000000000000 ) ) ;
#18575 = CARTESIAN_POINT ( 'NONE',  ( -5.529263428287297444, 53.92731371789854222, -7.954856959092311719 ) ) ;
#18576 = CARTESIAN_POINT ( 'NONE',  ( 10.31873187879411091, 0.000000000000000000, -7.340624999385508609 ) ) ;
#18577 = CARTESIAN_POINT ( 'NONE',  ( 9.465287035748106703, 112.0023137178985451, -2.064181346179063237 ) ) ;
#18578 = CARTESIAN_POINT ( 'NONE',  ( 22.56230152254410370, 7.347880794884117764E-16, -0.5624999987710044280 ) ) ;
#18579 = CARTESIAN_POINT ( 'NONE',  ( -10.69584247140429412, 34.95231371789854791, -6.932735513424201024 ) ) ;
#18580 = CARTESIAN_POINT ( 'NONE',  ( -11.61527771782819940, 85.73518628210143788, 4.622313124798574258 ) ) ;
#18581 = CARTESIAN_POINT ( 'NONE',  ( 13.56230152254410548, 5.196152422706630247, -6.712499998771020771 ) ) ;
#18582 = CARTESIAN_POINT ( 'NONE',  ( 26.99999999999999645, 7.347880794884117764E-16, -2.925000000000010925 ) ) ;
#18583 = CARTESIAN_POINT ( 'NONE',  ( 37.14004103287923186, 3.604726614523238837, 162.8445854527759309 ) ) ;
#18584 = CARTESIAN_POINT ( 'NONE',  ( 19.68408634441910721, 5.407089921784862696, -3.046874999385523530 ) ) ;
#18585 = SURFACE_SIDE_STYLE ('',( #30511 ) ) ;
#18586 = FACE_OUTER_BOUND ( 'NONE', #14655, .T. ) ;
#18587 = CARTESIAN_POINT ( 'NONE',  ( 18.00000000000000355, 244.2249999999999943, 5.196152422706632912 ) ) ;
#18588 = CARTESIAN_POINT ( 'NONE',  ( -8.710071997420127943, 96.08518628210146062, -3.796722387233380402 ) ) ;
#18589 = FACE_OUTER_BOUND ( 'NONE', #24828, .T. ) ;
#18590 = CARTESIAN_POINT ( 'NONE',  ( -12.50000000000000355, 123.1101862821014663, -0.1745138560725492671 ) ) ;
#18591 = CARTESIAN_POINT ( 'NONE',  ( 22.56230152254412502, 7.347880794884125653E-16, -3.375000000000044409 ) ) ;
#18592 = CARTESIAN_POINT ( 'NONE',  ( 26.75643035624999655, 240.0718750006145399, -7.049594010296217766E-16 ) ) ;
#18593 = ORIENTED_EDGE ( 'NONE', *, *, #35785, .T. ) ;
#18594 = CARTESIAN_POINT ( 'NONE',  ( 37.37209319794485651, 7.646167579472015790E-16, 165.4969538364452148 ) ) ;
#18595 = CARTESIAN_POINT ( 'NONE',  ( 23.87821517812499650, 4.985214923628404904, -3.440624999385466509 ) ) ;
#18596 = VECTOR ( 'NONE', #35790, 1000.000000000000000 ) ;
#18597 = DIRECTION ( 'NONE',  ( 0.000000000000000000, 1.000000000000000000, 0.000000000000000000 ) ) ;
#18598 = CARTESIAN_POINT ( 'NONE',  ( 34.00277893598041601, 5.196152422706637353, 164.2013035824986957 ) ) ;
#18599 = CARTESIAN_POINT ( 'NONE',  ( 0.000000000000000000, 0.000000000000000000, 0.000000000000000000 ) ) ;
#18600 = CARTESIAN_POINT ( 'NONE',  ( 7.234628195640322446, 199.3450961906613657, 26.99999999999999645 ) ) ;
#18601 = CARTESIAN_POINT ( 'NONE',  ( 23.87821517812500005, 242.3593750006145342, 4.985214923628404016 ) ) ;
#18602 = CARTESIAN_POINT ( 'NONE',  ( 13.44051670066910908, -5.407089921784859143, -0.5156249993855110958 ) ) ;
#18603 = CARTESIAN_POINT ( 'NONE',  ( -5.529263428287297444, 17.12731371789855217, -7.954856959092311719 ) ) ;
#18604 = CARTESIAN_POINT ( 'NONE',  ( 13.62178482187499640, 197.9093750006145456, -23.59362340125807123 ) ) ;
#18606 = ORIENTED_EDGE ( 'NONE', *, *, #20272, .T. ) ;
#18605 = VERTEX_POINT ( 'NONE', #371 ) ;
#18607 = CARTESIAN_POINT ( 'NONE',  ( 15.24356964375000167, 246.1843750006145513, 3.323476615752272600 ) ) ;
#18608 = CARTESIAN_POINT ( 'NONE',  ( -4.622313124798826500, 32.36481371789854933, 11.61527771782809637 ) ) ;
#18609 = CARTESIAN_POINT ( 'NONE',  ( 18.12178482187500350, -4.985214923628407568, -2.765624999385457805 ) ) ;
#18610 = CARTESIAN_POINT ( 'NONE',  ( -0.1745138560722442889, 128.3898137178985621, -15.50000000000000533 ) ) ;
#18611 = CARTESIAN_POINT ( 'NONE',  ( 18.12178482187499640, 4.985214923628404904, -0.3281249993854762348 ) ) ;
#18612 =( BOUNDED_CURVE ( )  B_SPLINE_CURVE ( 2, ( #31667, #2852, #3981, #18219, #24458, #27112, #27294 ),
 .UNSPECIFIED., .F., .F. ) 
 B_SPLINE_CURVE_WITH_KNOTS ( ( 3, 2, 2, 3 ),
 ( 0.2608695652173921298, 0.2681159420289864759, 0.2753623188405807110, 0.2826086956521750015 ),
 .UNSPECIFIED. ) 
 CURVE ( )  GEOMETRIC_REPRESENTATION_ITEM ( )  RATIONAL_B_SPLINE_CURVE ( ( 0.9999999999999845679, 0.8660254037844541397, 1.000000000000000000, 0.8660254037844387076, 1.000000000000000000, 0.8660254037844181685, 1.000000000000020428 ) ) 
 REPRESENTATION_ITEM ( '' )  );
#18613 = FACE_OUTER_BOUND ( 'NONE', #31787, .T. ) ;
#18614 = ORIENTED_EDGE ( 'NONE', *, *, #31562, .F. ) ;
#18615 = CARTESIAN_POINT ( 'NONE',  ( 19.68408634441911431, -5.407089921784861808, -5.446874999385537208 ) ) ;
#18616 = ORIENTED_EDGE ( 'NONE', *, *, #34724, .T. ) ;
#18617 = CARTESIAN_POINT ( 'NONE',  ( 27.24356964375000700, 195.4906250006145001, 15.72908226750537075 ) ) ;
#18618 = CARTESIAN_POINT ( 'NONE',  ( -2.660918448318275509, 139.4976862821014549, 12.46528703574805874 ) ) ;
#18619 = CARTESIAN_POINT ( 'NONE',  ( 34.01542801315541453, -5.407089921784861808, 162.9485590723218422 ) ) ;
#18620 = CARTESIAN_POINT ( 'NONE',  ( -60.48586230271183695, 205.8500491399821613, 7.418979330068642852 ) ) ;
#18621 = CARTESIAN_POINT ( 'NONE',  ( 18.12178482187499640, 246.9718750006145171, -4.985214923628404904 ) ) ;
#18622 = SURFACE_STYLE_FILL_AREA ( #24846 ) ;
#18623 = AXIS2_PLACEMENT_3D ( 'NONE', #7969, #10433, #19361 ) ;
#18624 = FACE_OUTER_BOUND ( 'NONE', #13420, .T. ) ;
#18625 = CARTESIAN_POINT ( 'NONE',  ( -41.09002896937850124, 206.1606490808709111, 2.350049139982143931 ) ) ;
#18627 = EDGE_CURVE ( 'NONE', #14808, #18936, #27422, .T. ) ;
#18626 = CARTESIAN_POINT ( 'NONE',  ( 10.49813415415989581, 137.7726862821014606, 7.228626920339068285 ) ) ;
#18628 = CARTESIAN_POINT ( 'NONE',  ( 34.29487111334006499, -5.407089921784855591, 166.1426083230784911 ) ) ;
#18629 = ORIENTED_EDGE ( 'NONE', *, *, #24986, .T. ) ;
#18630 = CARTESIAN_POINT ( 'NONE',  ( -69.00000000000002842, 206.0000000000000000, -2.499999999999998668 ) ) ;
#18631 = CARTESIAN_POINT ( 'NONE',  ( -6.092822981423970496, 130.5851862821014606, 14.25334919248782661 ) ) ;
#18632 = CARTESIAN_POINT ( 'NONE',  ( -50.39955436395490551, 216.3070033484980002, -6.137860380172975638 ) ) ;
#18633 = CARTESIAN_POINT ( 'NONE',  ( 8.152565276336714462, 117.6476862821014322, -5.233372021372432847 ) ) ;
#18634 = DIRECTION ( 'NONE',  ( 0.000000000000000000, -0.000000000000000000, 1.000000000000000000 ) ) ;
#18635 = CARTESIAN_POINT ( 'NONE',  ( -8.715434833791929847, 32.26018628210145067, -8.962234695871762469 ) ) ;
#18636 = CARTESIAN_POINT ( 'NONE',  ( 16.56230152254411436, -6.928203230275514990, -7.537500000000000533 ) ) ;
#18637 = VERTEX_POINT ( 'NONE', #11937 ) ;
#18638 = CARTESIAN_POINT ( 'NONE',  ( -4.694659320240884604E-14, 197.5250000012290172, 27.00000000000000000 ) ) ;
#18639 = CARTESIAN_POINT ( 'NONE',  ( -14.25334919248782306, 114.4851862821014663, -6.092822981423979378 ) ) ;
#18640 = CYLINDRICAL_SURFACE ( 'NONE', #3663, 6.000000000000001776 ) ;
#18641 = CARTESIAN_POINT ( 'NONE',  ( 5.529263428287477744, 6.672686282101436106, -7.954856959092191815 ) ) ;
#18642 = CARTESIAN_POINT ( 'NONE',  ( 13.62178482187499640, 199.2031250006145342, -23.59362340125807123 ) ) ;
#18643 = CARTESIAN_POINT ( 'NONE',  ( 27.00000000000036593, -3.464101615137536783, -5.662499999999986322 ) ) ;
#18644 = CARTESIAN_POINT ( 'NONE',  ( 27.00000000000001066, 195.6875000000000000, 15.58845726811988897 ) ) ;
#18645 = CARTESIAN_POINT ( 'NONE',  ( 21.97516523924395315, -2.816244198902225992, -10.00000000000000178 ) ) ;
#18646 = EDGE_CURVE ( 'NONE', #25890, #18678, #35161, .T. ) ;
#18647 = DIRECTION ( 'NONE',  ( 0.000000000000000000, 0.000000000000000000, 1.000000000000000000 ) ) ;
#18648 = CARTESIAN_POINT ( 'NONE',  ( -8.710071997420207879, 70.31481371789853085, 3.796722387233182339 ) ) ;
#18649 = ORIENTED_EDGE ( 'NONE', *, *, #894, .F. ) ;
#18650 = CARTESIAN_POINT ( 'NONE',  ( 15.00000000000000000, 244.1687500012290570, -3.464101615137752166 ) ) ;
#18651 = CARTESIAN_POINT ( 'NONE',  ( 2.311890736173452421, 82.67731371789854222, -12.53471296425189152 ) ) ;
#18652 = CARTESIAN_POINT ( 'NONE',  ( 10.31873187879411091, -3.604726614523244610, -4.659374999385518024 ) ) ;
#18653 = CARTESIAN_POINT ( 'NONE',  ( 3.253724281355069334E-15, 199.5500000012290513, -27.00000000000000355 ) ) ;
#18654 = CARTESIAN_POINT ( 'NONE',  ( 23.87821517812499650, 4.985214923628404904, -3.553124999385481875 ) ) ;
#18655 = CARTESIAN_POINT ( 'NONE',  ( -8.715434833792127023, 51.33981371789855785, 8.962234695871568846 ) ) ;
#18656 = ADVANCED_FACE ( 'NONE', ( #14414 ), #11752, .F. ) ;
#18657 = EDGE_LOOP ( 'NONE', ( #26819, #17568, #15940, #25194 ) ) ;
#18658 = CIRCLE ( 'NONE', #16837, 7.500000000000000000 ) ;
#18659 = DIRECTION ( 'NONE',  ( -0.000000000000000000, -1.000000000000000000, -0.000000000000000000 ) ) ;
#18660 = CARTESIAN_POINT ( 'NONE',  ( 15.24356964375000167, 243.9343750006145228, 3.323476615752272600 ) ) ;
#18661 = CARTESIAN_POINT ( 'NONE',  ( 6.932735513423970097, 18.74768628210143717, 10.69584247140445044 ) ) ;
#18662 = CARTESIAN_POINT ( 'NONE',  ( -41.48586230271182984, 206.8500491399821328, 5.686928522499748340 ) ) ;
#18663 = CARTESIAN_POINT ( 'NONE',  ( -51.38169563604516554, 210.1155267958017703, 6.500000000000000888 ) ) ;
#18664 = CARTESIAN_POINT ( 'NONE',  ( 0.3500000000000069722, 244.5000000000000000, 2.500000000000000000 ) ) ;
#18665 = CARTESIAN_POINT ( 'NONE',  ( -6.932735513424201912, 78.65231371789855075, 10.69584247140429412 ) ) ;
#18666 = CARTESIAN_POINT ( 'NONE',  ( -51.58705436395489841, 206.7903428501026042, -3.378800118222489157 ) ) ;
#18667 = CARTESIAN_POINT ( 'NONE',  ( -52.77455436395490551, 205.1570982666397356, 4.673758765035198159 ) ) ;
#18668 = VECTOR ( 'NONE', #11716, 1000.000000000000000 ) ;
#18669 = CARTESIAN_POINT ( 'NONE',  ( 15.24356964374999990, 0.000000000000000000, -5.653124999385472194 ) ) ;
#18670 = CARTESIAN_POINT ( 'NONE',  ( 10.56230152254410903, 0.000000000000000000, -0.7874999987710074034 ) ) ;
#18671 = CARTESIAN_POINT ( 'NONE',  ( 11.08355503943118769, 49.03981371789855359, 10.83675517735179028 ) ) ;
#18672 = CARTESIAN_POINT ( 'NONE',  ( -45.84002896937850124, 202.6965474657332038, 4.350049139982197666 ) ) ;
#18673 = CARTESIAN_POINT ( 'NONE',  ( 22.12957385106072294, -6.276043463296034908, -7.973380326861742695 ) ) ;
#18674 = CARTESIAN_POINT ( 'NONE',  ( 0.1745138560725515708, 79.41018628210144925, -12.50000000000000355 ) ) ;
#18675 = CARTESIAN_POINT ( 'NONE',  ( -15.53471296425195369, 21.62268628210143717, 2.908627838312118019 ) ) ;
#18676 = CARTESIAN_POINT ( 'NONE',  ( 13.56230152254411436, -5.196152422706638241, -0.3750000000000419664 ) ) ;
#18677 = CARTESIAN_POINT ( 'NONE',  ( -13.49999999999998401, 197.4875000012290229, 23.38268590217985476 ) ) ;
#18678 = VERTEX_POINT ( 'NONE', #20486 ) ;
#18679 = VECTOR ( 'NONE', #14017, 1000.000000000000000 ) ;
#18680 = CARTESIAN_POINT ( 'NONE',  ( -15.50000000000000533, 40.31018628210145494, -0.1745138560725808530 ) ) ;
#18681 = CARTESIAN_POINT ( 'NONE',  ( 27.24356964375000345, 197.7781250006145228, -3.336375036156643733E-15 ) ) ;
#18682 = EDGE_CURVE ( 'NONE', #19052, #25162, #9277, .T. ) ;
#18683 = DIRECTION ( 'NONE',  ( -1.000000000000000000, 0.000000000000000000, 0.000000000000000000 ) ) ;
#18684 = CARTESIAN_POINT ( 'NONE',  ( 22.60769515458672885, 247.6174038105676516, -6.000000000000000000 ) ) ;
#18685 = CARTESIAN_POINT ( 'NONE',  ( -40.50372103062156981, 216.5309553116391612, -1.626142955000564383 ) ) ;
#18686 = CARTESIAN_POINT ( 'NONE',  ( 37.29858702344112231, 7.347880794884125653E-16, 167.4514226650291562 ) ) ;
#18687 = CARTESIAN_POINT ( 'NONE',  ( -12.46528703574805697, 22.19768628210145067, -2.660918448318280838 ) ) ;
#18688 = CARTESIAN_POINT ( 'NONE',  ( 15.24356964374999990, 249.3718750006145228, -3.323476615752268604 ) ) ;
#18689 = CARTESIAN_POINT ( 'NONE',  ( 5.233372021372610483, 138.4523137178985621, -8.152565276336593669 ) ) ;
#18690 = CARTESIAN_POINT ( 'NONE',  ( 20.99999999999999645, 243.6718750006145058, 6.646953231504538984 ) ) ;
#18691 = ORIENTED_EDGE ( 'NONE', *, *, #7625, .F. ) ;
#18692 = FACE_OUTER_BOUND ( 'NONE', #14009, .T. ) ;
#18693 = ADVANCED_FACE ( 'NONE', ( #34501 ), #34681, .F. ) ;
#18694 = CARTESIAN_POINT ( 'NONE',  ( -0.1745138560722763466, 128.3898137178985621, -12.50000000000000355 ) ) ;
#18695 = CARTESIAN_POINT ( 'NONE',  ( 10.31873187879411091, 3.604726614523236616, -7.378124999385539340 ) ) ;
#18696 = CARTESIAN_POINT ( 'NONE',  ( 34.11184405356999605, 5.407089921784857367, 164.0505994570858093 ) ) ;
#18697 = LINE ( 'NONE', #7491, #21451 ) ;
#18698 = CARTESIAN_POINT ( 'NONE',  ( 26.99999999999999645, 196.6625000000000227, -15.58845726811990495 ) ) ;
#18699 = ORIENTED_EDGE ( 'NONE', *, *, #34367, .T. ) ;
#18700 = CARTESIAN_POINT ( 'NONE',  ( -12.50000000000000355, 49.51018628210145067, -0.1745138560725492671 ) ) ;
#18701 = ORIENTED_EDGE ( 'NONE', *, *, #2517, .F. ) ;
#18702 = VECTOR ( 'NONE', #12457, 1000.000000000000000 ) ;
#18703 = ORIENTED_EDGE ( 'NONE', *, *, #5546, .F. ) ;
#18704 = DIRECTION ( 'NONE',  ( 0.000000000000000000, 0.000000000000000000, 1.000000000000000000 ) ) ;
#18705 = CARTESIAN_POINT ( 'NONE',  ( 1.120210788295102201E-13, 195.0500000012290513, -27.00000000000000711 ) ) ;
#18706 = CARTESIAN_POINT ( 'NONE',  ( 2.999999999999997335, 244.5000000000000000, 0.000000000000000000 ) ) ;
#18707 = CARTESIAN_POINT ( 'NONE',  ( 20.99999999999999645, 185.0294372515228645, -5.999999999999999112 ) ) ;
#18708 = CARTESIAN_POINT ( 'NONE',  ( 26.75643035624999655, 3.323476615752271712, -8.428124999385486760 ) ) ;
#18709 = CARTESIAN_POINT ( 'NONE',  ( -10.69584247140444866, 85.44768628210144357, 6.932735513423972762 ) ) ;
#18710 = CARTESIAN_POINT ( 'NONE',  ( 14.38691631536207538, 136.3351862821014606, -5.770363421893813793 ) ) ;
#18711 =( BOUNDED_CURVE ( )  B_SPLINE_CURVE ( 2, ( #1967, #13916, #13165, #25093, #19804, #24721, #10317 ),
 .UNSPECIFIED., .F., .F. ) 
 B_SPLINE_CURVE_WITH_KNOTS ( ( 3, 2, 2, 3 ),
 ( 0.3695652173913035465, 0.3768115942028978371, 0.3840579710144921277, 0.3913043478260864183 ),
 .UNSPECIFIED. ) 
 CURVE ( )  GEOMETRIC_REPRESENTATION_ITEM ( )  RATIONAL_B_SPLINE_CURVE ( ( 1.000000000000014433, 0.8660254037844243857, 1.000000000000000000, 0.8660254037844387076, 1.000000000000000000, 0.8660254037844489217, 0.9999999999999897859 ) ) 
 REPRESENTATION_ITEM ( '' )  );
#18712 = EDGE_CURVE ( 'NONE', #25502, #27686, #14602, .T. ) ;
#18713 = CARTESIAN_POINT ( 'NONE',  ( 14.04484906357221341, 216.9551509364261790, 0.1802446458343258673 ) ) ;
#18714 = CARTESIAN_POINT ( 'NONE',  ( -58.90252896937851546, 207.6499508600178387, -3.839350919129087547 ) ) ;
#18715 = DIRECTION ( 'NONE',  ( 0.000000000000000000, 0.000000000000000000, -1.000000000000000000 ) ) ;
#18716 = CARTESIAN_POINT ( 'NONE',  ( 25.17756528844239483, 0.000000000000000000, 166.5920692191248804 ) ) ;
#18717 = CARTESIAN_POINT ( 'NONE',  ( -4.622313124798826500, 133.5648137178985735, 11.61527771782809637 ) ) ;
#18718 = CARTESIAN_POINT ( 'NONE',  ( -42.68080436395489841, 203.5000000000000000, -0.1155267958017335561 ) ) ;
#18719 = CARTESIAN_POINT ( 'NONE',  ( -53.76413769728823411, 214.1499508600179240, 7.418979330068584233 ) ) ;
#18720 = ITEM_DEFINED_TRANSFORMATION ( 'NONE', 'NONE', #31118,  #17215 ) ;
#18721 = CARTESIAN_POINT ( 'NONE',  ( 30.78214267663954473, 6.928203230275514990, 161.8104024270723755 ) ) ;
#18722 = CARTESIAN_POINT ( 'NONE',  ( -1.926257025242585782E-15, 197.4406250006145740, -31.45816453501075927 ) ) ;
#18723 = CARTESIAN_POINT ( 'NONE',  ( -13.04141134922778456, 116.0273137178985792, 8.927990412390377273 ) ) ;
#18724 = CARTESIAN_POINT ( 'NONE',  ( -46.43377896937850835, 208.3738570449995109, 6.530955311639247363 ) ) ;
#18725 = EDGE_CURVE ( 'NONE', #18565, #36216, #28438, .T. ) ;
#18726 = VERTEX_POINT ( 'NONE', #20669 ) ;
#18727 = CARTESIAN_POINT ( 'NONE',  ( -13.50000000000000533, 197.6750000000000114, -23.38268590217984411 ) ) ;
#18728 =( BOUNDED_CURVE ( )  B_SPLINE_CURVE ( 2, ( #34132, #20110, #8544, #17082, #37334, #22771, #36970 ),
 .UNSPECIFIED., .F., .F. ) 
 B_SPLINE_CURVE_WITH_KNOTS ( ( 3, 2, 2, 3 ),
 ( 0.8260869565217394683, 0.8333333333333347026, 0.8405797101449297148, 0.8478260869565249491 ),
 .UNSPECIFIED. ) 
 CURVE ( )  GEOMETRIC_REPRESENTATION_ITEM ( )  RATIONAL_B_SPLINE_CURVE ( ( 0.9999999999999938938, 0.8660254037844448138, 1.000000000000000000, 0.8660254037844387076, 1.000000000000000000, 0.8660254037843791997, 1.000000000000059508 ) ) 
 REPRESENTATION_ITEM ( '' )  );
#18729 = CARTESIAN_POINT ( 'NONE',  ( 24.74781001545762393, 3.604726614523240613, 164.4745922192587670 ) ) ;
#18730 = CARTESIAN_POINT ( 'NONE',  ( -11.08355503943142573, 112.7601862821014720, 10.83675517735155402 ) ) ;
#18731 = CARTESIAN_POINT ( 'NONE',  ( -55.34747103062156981, 213.3500491399821328, -5.571401726697985168 ) ) ;
#18732 = CARTESIAN_POINT ( 'NONE',  ( 10.31873187879410736, 0.000000000000000000, -4.190624999385549998 ) ) ;
#18733 = CARTESIAN_POINT ( 'NONE',  ( 8.843639120294328748, 35.13518628210143646, -3.474262827703334722 ) ) ;
#18734 = CARTESIAN_POINT ( 'NONE',  ( 1.069080835302379631E-14, 198.8750000012290400, 27.00000000000000000 ) ) ;
#18735 = CARTESIAN_POINT ( 'NONE',  ( -34.36830436395490551, 209.8844732041983150, 8.500000000000003553 ) ) ;
#18736 = CARTESIAN_POINT ( 'NONE',  ( 13.44051670066910908, 5.407089921784862696, -9.721874999385510918 ) ) ;
#18737 = CARTESIAN_POINT ( 'NONE',  ( 4.944772684328679446, 70.78518628210144925, -11.48171059495397373 ) ) ;
#18738 = CARTESIAN_POINT ( 'NONE',  ( -27.00000000000000355, 199.5124999999999886, -15.58845726811989429 ) ) ;
#18739 = DIRECTION ( 'NONE',  ( -0.000000000000000000, -1.000000000000000000, 0.000000000000000000 ) ) ;
#18741 = ORIENTED_EDGE ( 'NONE', *, *, #2507, .T. ) ;
#18740 = CARTESIAN_POINT ( 'NONE',  ( 2.064181346179272847, 42.89768628210143220, -9.465287035748065847 ) ) ;
#18742 = CARTESIAN_POINT ( 'NONE',  ( 24.00000000000000000, -5.196152422706629359, -6.093749998770964460 ) ) ;
#18743 = VERTEX_POINT ( 'NONE', #5319 ) ;
#18744 = CARTESIAN_POINT ( 'NONE',  ( 18.00000000000000000, 5.196152422706630247, -1.425000000000009592 ) ) ;
#18745 = CARTESIAN_POINT ( 'NONE',  ( -61.87872103062154849, 203.4690446883607535, 1.626142955000567936 ) ) ;
#18746 = CARTESIAN_POINT ( 'NONE',  ( 27.82830044041545747, -5.407089921784865361, 163.8662950338039650 ) ) ;
#18747 = CARTESIAN_POINT ( 'NONE',  ( 27.71838675424445597, 5.196152422706636465, 161.2126517282112275 ) ) ;
#18748 = CARTESIAN_POINT ( 'NONE',  ( 21.00000000000000000, 245.1625000000000227, 6.928203230275506996 ) ) ;
#18749 = DIRECTION ( 'NONE',  ( -1.000000000000000000, 0.000000000000000000, -0.000000000000000000 ) ) ;
#18750 = CARTESIAN_POINT ( 'NONE',  ( 11.48171059495408208, 93.31481371789855928, -4.944772684328420986 ) ) ;
#18751 = CARTESIAN_POINT ( 'NONE',  ( 4.944772684328679446, 98.38518628210145778, -11.48171059495397373 ) ) ;
#18752 = VERTEX_POINT ( 'NONE', #28434 ) ;
#18753 = EDGE_LOOP ( 'NONE', ( #30518, #16799, #9120, #3993, #19005, #30918 ) ) ;
#18754 = CARTESIAN_POINT ( 'NONE',  ( 27.00000000000001066, 198.0500000012290513, 15.58845726811988897 ) ) ;
#18755 = CARTESIAN_POINT ( 'NONE',  ( -7.234628195640263826, 196.7575961894323484, -27.00000000000003553 ) ) ;
#18756 = CARTESIAN_POINT ( 'NONE',  ( 2.908627838312458636, 82.67731371789852801, -15.53471296425188442 ) ) ;
#18757 = CARTESIAN_POINT ( 'NONE',  ( 15.24356964374999990, 3.323476615752268604, -7.040624999385501681 ) ) ;
#18758 = CARTESIAN_POINT ( 'NONE',  ( 21.00000000000000000, 246.3718750006145228, 6.646953231504538984 ) ) ;
#18759 = CARTESIAN_POINT ( 'NONE',  ( -51.19122103062157692, 208.9097554298617752, -4.530955311639240257 ) ) ;
#18760 = ADVANCED_BREP_SHAPE_REPRESENTATION ( '', ( #21172, #17215 ), #1426 ) ;
#18761 = CARTESIAN_POINT ( 'NONE',  ( 27.00000000000000355, 194.9375000012290400, -3.306546357697854128E-15 ) ) ;
#18762 = CARTESIAN_POINT ( 'NONE',  ( 9.465287035748106703, 66.00231371789855928, -2.064181346179063237 ) ) ;
#18763 = EDGE_CURVE ( 'NONE', #22653, #11771, #14048, .T. ) ;
#18764 = CARTESIAN_POINT ( 'NONE',  ( 10.31873187879410914, 0.000000000000000000, -8.240624999385548932 ) ) ;
#18765 = CARTESIAN_POINT ( 'NONE',  ( 6.594114490232462877, 120.3398137178985507, -6.840914352311949109 ) ) ;
#18766 = CARTESIAN_POINT ( 'NONE',  ( 15.24356964375000167, 240.3343750006145285, 3.323476615752272600 ) ) ;
#18767 = CARTESIAN_POINT ( 'NONE',  ( 4.944772684328420986, 31.21481371789855430, 11.48171059495408208 ) ) ;
#18768 =( BOUNDED_CURVE ( )  B_SPLINE_CURVE ( 2, ( #27794, #36498, #30268, #10541, #27976, #22301, #25133 ),
 .UNSPECIFIED., .F., .F. ) 
 B_SPLINE_CURVE_WITH_KNOTS ( ( 3, 2, 2, 3 ),
 ( 0.6521739130434773823, 0.6594202898550715064, 0.6666666666666654084, 0.6739130434782595325 ),
 .UNSPECIFIED. ) 
 CURVE ( )  GEOMETRIC_REPRESENTATION_ITEM ( )  RATIONAL_B_SPLINE_CURVE ( ( 1.000000000000016431, 0.8660254037844222763, 1.000000000000000000, 0.8660254037844387076, 1.000000000000000000, 0.8660254037844633546, 0.9999999999999753530 ) ) 
 REPRESENTATION_ITEM ( '' )  );
#18769 = EDGE_CURVE ( 'NONE', #407, #18510, #13149, .T. ) ;
#18770 = CARTESIAN_POINT ( 'NONE',  ( -12.53471296425194836, 86.02268628210146062, 2.311890736173176641 ) ) ;
#18771 = CARTESIAN_POINT ( 'NONE',  ( 19.56230152254411436, -5.196152422706629359, -8.737499998771019349 ) ) ;
#18772 = ADVANCED_FACE ( 'NONE', ( #15731 ), #32591, .T. ) ;
#18773 = CYLINDRICAL_SURFACE ( 'NONE', #23770, 5.999999999999999112 ) ;
#18774 = CARTESIAN_POINT ( 'NONE',  ( 24.79846929092969887, -3.604726614523240613, 165.0536303875245778 ) ) ;
#18775 = PRODUCT_DEFINITION ( 'UNKNOWN', '', #4487, #32371 ) ;
#18776 = CARTESIAN_POINT ( 'NONE',  ( 10.31873187879411091, -3.604726614523244610, -3.759374999385526106 ) ) ;
#18777 = CARTESIAN_POINT ( 'NONE',  ( 16.56230152254411792, -6.928203230275514990, -1.687500000000023981 ) ) ;
#18778 = LINE ( 'NONE', #27470, #679 ) ;
#18779 = CARTESIAN_POINT ( 'NONE',  ( -9.534712964251941258, 95.22268628210143504, 1.715153634034234154 ) ) ;
#18780 = DIRECTION ( 'NONE',  ( 1.000000000000000000, 0.000000000000000000, 0.000000000000000000 ) ) ;
#18781 = CARTESIAN_POINT ( 'NONE',  ( -4.944772684328673229, 130.5851862821014606, 11.48171059495397728 ) ) ;
#18782 = CARTESIAN_POINT ( 'NONE',  ( 20.99999999999999289, 248.9874999999999829, -5.999999999999997335 ) ) ;
#18783 = CARTESIAN_POINT ( 'NONE',  ( 26.75643035624999655, 240.9343750006144944, 3.323476615752267715 ) ) ;
#18784 = ORIENTED_EDGE ( 'NONE', *, *, #3203, .F. ) ;
#18785 = CARTESIAN_POINT ( 'NONE',  ( 37.32960477335537774, -3.604726614523235284, 165.0113089211254760 ) ) ;
#18786 = CARTESIAN_POINT ( 'NONE',  ( 26.75643035624999655, 3.323476615752271712, -3.928124999385464999 ) ) ;
#18787 = DIRECTION ( 'NONE',  ( 0.000000000000000000, 0.000000000000000000, 1.000000000000000000 ) ) ;
#18788 = CARTESIAN_POINT ( 'NONE',  ( 34.35575969410840003, 5.196152422706637353, 168.2358921097703046 ) ) ;
#18789 = FACE_OUTER_BOUND ( 'NONE', #14519, .T. ) ;
#18790 = CARTESIAN_POINT ( 'NONE',  ( 15.24356964374999990, 241.7593750006145399, 0.000000000000000000 ) ) ;
#18791 = CARTESIAN_POINT ( 'NONE',  ( 19.68408634441910721, -5.407089921784855591, -2.240624999385543159 ) ) ;
#18792 = CARTESIAN_POINT ( 'NONE',  ( -8.152565276336593669, 7.352313717898546486, -5.233372021372610483 ) ) ;
#18793 = CARTESIAN_POINT ( 'NONE',  ( 27.24356964375000700, 197.7968750006145342, 15.72908226750537075 ) ) ;
#18794 = VECTOR ( 'NONE', #743, 1000.000000000000000 ) ;
#18796 = ORIENTED_EDGE ( 'NONE', *, *, #35289, .F. ) ;
#18795 = ORIENTED_EDGE ( 'NONE', *, *, #425, .F. ) ;
#18797 = CARTESIAN_POINT ( 'NONE',  ( 23.87821517812500005, 246.2968750006145058, 4.985214923628404016 ) ) ;
#18798 = CARTESIAN_POINT ( 'NONE',  ( -8.715434833792127023, 32.93981371789854506, 8.962234695871568846 ) ) ;
#18799 = CARTESIAN_POINT ( 'NONE',  ( 23.87821517812500005, -4.985214923628404016, -0.8906249993854697955 ) ) ;
#18800 = CARTESIAN_POINT ( 'NONE',  ( -3.257655550456946880, 128.1023137178985678, -15.46528703574811736 ) ) ;
#18801 = CARTESIAN_POINT ( 'NONE',  ( 26.99999999999999645, -3.464101615137751278, -9.206249998770948295 ) ) ;
#18802 = ORIENTED_EDGE ( 'NONE', *, *, #3340, .T. ) ;
#18803 = CARTESIAN_POINT ( 'NONE',  ( 16.56230152254411436, 7.209453229046482114, -6.159374999385524241 ) ) ;
#18804 = ORIENTED_EDGE ( 'NONE', *, *, #8505, .F. ) ;
#18805 = CARTESIAN_POINT ( 'NONE',  ( 5.778771075727756162E-15, 197.2156250006145513, 31.45816453501075927 ) ) ;
#18806 = AXIS2_PLACEMENT_3D ( 'NONE', #28632, #25980, #2670 ) ;
#18807 = CARTESIAN_POINT ( 'NONE',  ( 12.50000000000000355, 127.7101862821014606, 0.1745138560725507937 ) ) ;
#18808 = CARTESIAN_POINT ( 'NONE',  ( 27.69756682629397915, 5.407089921784862696, 162.3720029866663594 ) ) ;
#18809 = CARTESIAN_POINT ( 'NONE',  ( -55.34002896937850124, 202.6965474657332038, 4.350049139982197666 ) ) ;
#18810 = CARTESIAN_POINT ( 'NONE',  ( 23.87821517812499650, 246.4468750006145115, -4.985214923628404904 ) ) ;
#18811 = DIRECTION ( 'NONE',  ( 1.000000000000000000, 0.000000000000000000, 0.000000000000000000 ) ) ;
#18812 = CARTESIAN_POINT ( 'NONE',  ( -49.79836230271183695, 206.0451222850691977, -2.149950860017851184 ) ) ;
#18813 =( BOUNDED_SURFACE ( )  B_SPLINE_SURFACE ( 1, 2, ( 
 ( #12615, #24181, #665, #481, #26827, #32326, #17749, #12236, #34982, #3329, #18509, #30048, #6554, #12048, #15274, #21349, #6741, #857, #12428, #23997, #3894, #296, #21161, #15465, #15654, #32889, #27019, #11861, #9025, #14900, #23619, #9212, #1228, #27580, #30620, #4451, #21718, #7680, #16031, #13179, #21902, #1609, #36102, #30991, #1796, #36662, #27766, #33083, #33641, #5009, #12799, #16403, #27203, #27949, #24369, #24733, #12996, #10331, #36283, #30239, #35913, #30431, #33449, #24552, #1979, #19260, #4265, #7492, #33830, #19068, #4637, #7126, #33269, #16216, #10511, #13363, #21537, #30799, #10145, #24918, #36470, #7867, #9956, #7308, #10700, #22091, #4822, #13551, #18880, #18698, #25104, #22277, #19441, #15840, #27388, #1418, #8053, #36845, #28500, #2356, #11075, #2164, #11264, #61, #2722, #17147, #17330, #2543, #10888, #14110, #13929, #31909, #5377, #22461, #37398, #37217, #11628, #16772, #16957, #28873, #2908, #25662, #28318, #5562, #37029, #34008, #34196, #13747, #19629, #23203, #34751, #22650, #5197, #22834, #14480 ),
 ( #11448, #16591, #28683, #23015, #8794, #26033, #19816, #31536, #8242, #8423, #20366, #25478, #28135, #34382, #19992, #31351, #14297, #34565, #25850, #8605, #20175, #31723, #5751, #25293, #31175, #23953, #32093, #15043, #23574, #6125, #6699, #15232, #9357, #26214, #6321, #17703, #35119, #18270, #32278, #29052, #20550, #26591, #251, #9168, #20735, #3284, #3096, #12383, #438, #29243, #35301, #17893, #12003, #14856, #20928, #32467, #621, #6510, #29438, #3474, #21119, #11815, #812, #12190, #26782, #14664, #23762, #26405, #18085, #32658, #29626, #5939, #8979, #23385, #17518, #3661, #35495, #9545, #34934, #3782, #9296, #32028, #29945, #3973, #29372, #11942, #18020, #35622, #18209, #20868, #748, #3410, #29751, #23322, #35433, #15357, #15546, #24077, #26528, #12319, #6259, #15168, #9668, #20672, #34873, #23700, #26716, #559, #17836, #26911, #12125, #32407, #29565, #35243, #32220, #27104, #9481, #32785, #35057, #23892, #6447, #14979, #1128, #12513, #32595, #29179, #3602, #21057, #3221, #939, #8914, #20489, #21245, #6058, #6820 ) ),
 .UNSPECIFIED., .F., .F., .F. ) 
 B_SPLINE_SURFACE_WITH_KNOTS ( ( 2, 2 ),
 ( 3, 2, 2, 2, 2, 2, 2, 2, 2, 2, 2, 2, 2, 2, 2, 2, 2, 2, 2, 2, 2, 2, 2, 2, 2, 2, 2, 2, 2, 2, 2, 2, 2, 2, 2, 2, 2, 2, 2, 2, 2, 2, 2, 2, 2, 2, 2, 2, 2, 2, 2, 2, 2, 2, 2, 2, 2, 2, 2, 2, 2, 2, 2, 2, 2, 2, 2, 3 ),
 ( 0.000000000000000000, 1.000000000000000000 ),
 ( 0.000000000000000000, 0.01388888888888888812, 0.02777777777777777624, 0.04166666666666666435, 0.05555555555555555247, 0.06944444444444444753, 0.08333333333333332871, 0.09722222222222222376, 0.1111111111111111049, 0.1250000000000000000, 0.1388888888888888951, 0.1527777777777777901, 0.1666666666666666574, 0.1805555555555555525, 0.1944444444444444475, 0.2083333333333333426, 0.2222222222222222099, 0.2361111111111111049, 0.2500000000000000000, 0.2638888888888888951, 0.2777777777777777901, 0.2916666666666666852, 0.3055555555555555802, 0.3194444444444444198, 0.3333333333333333148, 0.3472222222222222099, 0.3611111111111111049, 0.3750000000000000000, 0.3888888888888888951, 0.4027777777777777901, 0.4166666666666666852, 0.4305555555555555802, 0.4444444444444444198, 0.4583333333333333148, 0.4722222222222222099, 0.4861111111111111049, 0.5000000000000000000, 0.5138888888888888395, 0.5277777777777777901, 0.5416666666666666297, 0.5555555555555555802, 0.5694444444444444198, 0.5833333333333333703, 0.5972222222222222099, 0.6111111111111111605, 0.6250000000000000000, 0.6388888888888888395, 0.6527777777777777901, 0.6666666666666666297, 0.6805555555555555802, 0.6944444444444444198, 0.7083333333333333703, 0.7222222222222222099, 0.7361111111111111605, 0.7500000000000000000, 0.7638888888888888395, 0.7777777777777777901, 0.7916666666666666297, 0.8055555555555555802, 0.8194444444444444198, 0.8333333333333333703, 0.8472222222222222099, 0.8611111111111111605, 0.8750000000000000000, 0.8888888888888888395, 0.9027777777777777901, 0.9166666666666666297, 0.9258785558164617235 ),
 .UNSPECIFIED. ) 
 GEOMETRIC_REPRESENTATION_ITEM ( )  RATIONAL_B_SPLINE_SURFACE ( (
 ( 1.000000000000000000, 0.8660254037844387076, 1.000000000000000000, 0.8660254037844387076, 1.000000000000000000, 0.8660254037844387076, 1.000000000000000000, 0.8660254037844387076, 1.000000000000000000, 0.8660254037844387076, 1.000000000000000000, 0.8660254037844387076, 1.000000000000000000, 0.8660254037844387076, 1.000000000000000000, 0.8660254037844387076, 1.000000000000000000, 0.8660254037844387076, 1.000000000000000000, 0.8660254037844387076, 1.000000000000000000, 0.8660254037844387076, 1.000000000000000000, 0.8660254037844387076, 1.000000000000000000, 0.8660254037844387076, 1.000000000000000000, 0.8660254037844387076, 1.000000000000000000, 0.8660254037844387076, 1.000000000000000000, 0.8660254037844387076, 1.000000000000000000, 0.8660254037844387076, 1.000000000000000000, 0.8660254037844387076, 1.000000000000000000, 0.8660254037844387076, 1.000000000000000000, 0.8660254037844387076, 1.000000000000000000, 0.8660254037844387076, 1.000000000000000000, 0.8660254037844387076, 1.000000000000000000, 0.8660254037844387076, 1.000000000000000000, 0.8660254037844387076, 1.000000000000000000, 0.8660254037844387076, 1.000000000000000000, 0.8660254037844387076, 1.000000000000000000, 0.8660254037844387076, 1.000000000000000000, 0.8660254037844387076, 1.000000000000000000, 0.8660254037844387076, 1.000000000000000000, 0.8660254037844387076, 1.000000000000000000, 0.8660254037844387076, 1.000000000000000000, 0.8660254037844387076, 1.000000000000000000, 0.8660254037844387076, 1.000000000000000000, 0.8660254037844387076, 1.000000000000000000, 0.8660254037844387076, 1.000000000000000000, 0.8660254037844387076, 1.000000000000000000, 0.8660254037844387076, 1.000000000000000000, 0.8660254037844387076, 1.000000000000000000, 0.8660254037844387076, 1.000000000000000000, 0.8660254037844387076, 1.000000000000000000, 0.8660254037844387076, 1.000000000000000000, 0.8660254037844387076, 1.000000000000000000, 0.8660254037844387076, 1.000000000000000000, 0.8660254037844387076, 1.000000000000000000, 0.8660254037844387076, 1.000000000000000000, 0.8660254037844387076, 1.000000000000000000, 0.8660254037844387076, 1.000000000000000000, 0.8660254037844387076, 1.000000000000000000, 0.8660254037844387076, 1.000000000000000000, 0.8660254037844387076, 1.000000000000000000, 0.8660254037844387076, 1.000000000000000000, 0.8660254037844387076, 1.000000000000000000, 0.8660254037844387076, 1.000000000000000000, 0.8660254037844387076, 1.000000000000000000, 0.8660254037844387076, 1.000000000000000000, 0.8660254037844387076, 1.000000000000000000, 0.8660254037844387076, 1.000000000000000000, 0.8660254037844387076, 1.000000000000000000, 0.8660254037844387076, 1.000000000000000000, 0.8660254037844387076, 1.000000000000000000, 0.8660254037844387076, 1.000000000000000000, 0.8660254037844387076, 1.000000000000000000, 0.8660254037844387076, 1.000000000000000000, 0.8660254037844387076, 1.000000000000000000, 0.8660254037844387076, 1.000000000000000000, 0.8660254037844387076, 1.000000000000000000, 0.9111405426957062126, 0.9401542251575389919),
 ( 1.000000000000000000, 0.8660254037844387076, 1.000000000000000000, 0.8660254037844387076, 1.000000000000000000, 0.8660254037844387076, 1.000000000000000000, 0.8660254037844387076, 1.000000000000000000, 0.8660254037844387076, 1.000000000000000000, 0.8660254037844387076, 1.000000000000000000, 0.8660254037844387076, 1.000000000000000000, 0.8660254037844387076, 1.000000000000000000, 0.8660254037844387076, 1.000000000000000000, 0.8660254037844387076, 1.000000000000000000, 0.8660254037844387076, 1.000000000000000000, 0.8660254037844387076, 1.000000000000000000, 0.8660254037844387076, 1.000000000000000000, 0.8660254037844387076, 1.000000000000000000, 0.8660254037844387076, 1.000000000000000000, 0.8660254037844387076, 1.000000000000000000, 0.8660254037844387076, 1.000000000000000000, 0.8660254037844387076, 1.000000000000000000, 0.8660254037844387076, 1.000000000000000000, 0.8660254037844387076, 1.000000000000000000, 0.8660254037844387076, 1.000000000000000000, 0.8660254037844387076, 1.000000000000000000, 0.8660254037844387076, 1.000000000000000000, 0.8660254037844387076, 1.000000000000000000, 0.8660254037844387076, 1.000000000000000000, 0.8660254037844387076, 1.000000000000000000, 0.8660254037844387076, 1.000000000000000000, 0.8660254037844387076, 1.000000000000000000, 0.8660254037844387076, 1.000000000000000000, 0.8660254037844387076, 1.000000000000000000, 0.8660254037844387076, 1.000000000000000000, 0.8660254037844387076, 1.000000000000000000, 0.8660254037844387076, 1.000000000000000000, 0.8660254037844387076, 1.000000000000000000, 0.8660254037844387076, 1.000000000000000000, 0.8660254037844387076, 1.000000000000000000, 0.8660254037844387076, 1.000000000000000000, 0.8660254037844387076, 1.000000000000000000, 0.8660254037844387076, 1.000000000000000000, 0.8660254037844387076, 1.000000000000000000, 0.8660254037844387076, 1.000000000000000000, 0.8660254037844387076, 1.000000000000000000, 0.8660254037844387076, 1.000000000000000000, 0.8660254037844387076, 1.000000000000000000, 0.8660254037844387076, 1.000000000000000000, 0.8660254037844387076, 1.000000000000000000, 0.8660254037844387076, 1.000000000000000000, 0.8660254037844387076, 1.000000000000000000, 0.8660254037844387076, 1.000000000000000000, 0.8660254037844387076, 1.000000000000000000, 0.8660254037844387076, 1.000000000000000000, 0.8660254037844387076, 1.000000000000000000, 0.8660254037844387076, 1.000000000000000000, 0.8660254037844387076, 1.000000000000000000, 0.8660254037844387076, 1.000000000000000000, 0.8660254037844387076, 1.000000000000000000, 0.8660254037844387076, 1.000000000000000000, 0.8660254037844387076, 1.000000000000000000, 0.8660254037844387076, 1.000000000000000000, 0.8660254037844387076, 1.000000000000000000, 0.8660254037844387076, 1.000000000000000000, 0.8660254037844387076, 1.000000000000000000, 0.8660254037844387076, 1.000000000000000000, 0.8660254037844387076, 1.000000000000000000, 0.8660254037844387076, 1.000000000000000000, 0.8660254037844387076, 1.000000000000000000, 0.9111405426957062126, 0.9401542251575389919) ) ) 
 REPRESENTATION_ITEM ( '' )  SURFACE ( )  );
#18814 = CARTESIAN_POINT ( 'NONE',  ( -12.50000000000000355, 141.5101862821014720, -0.1745138560725492671 ) ) ;
#18815 = CARTESIAN_POINT ( 'NONE',  ( 13.56230152254411436, -5.196152422706632912, -2.062499998771005760 ) ) ;
#18816 = VERTEX_POINT ( 'NONE', #10030 ) ;
#18817 = CARTESIAN_POINT ( 'NONE',  ( -14.25334919248782306, 114.4851862821014663, -6.092822981423979378 ) ) ;
#18818 = CARTESIAN_POINT ( 'NONE',  ( -48.22247103062156981, 205.6499508600178956, 7.303452534266880569 ) ) ;
#18819 = CARTESIAN_POINT ( 'NONE',  ( -5.233372021372430183, 115.3476862821014493, -8.152565276336710909 ) ) ;
#18820 = FACE_OUTER_BOUND ( 'NONE', #28924, .T. ) ;
#18821 = CARTESIAN_POINT ( 'NONE',  ( 11.61527771782819940, 7.535186282101452804, -4.622313124798573369 ) ) ;
#18822 = CARTESIAN_POINT ( 'NONE',  ( 10.31873187879411091, -3.604726614523240613, -0.5531249993855127389 ) ) ;
#18823 = ORIENTED_EDGE ( 'NONE', *, *, #14956, .F. ) ;
#18824 = CARTESIAN_POINT ( 'NONE',  ( -35.15997103062156270, 215.5714017266979852, 3.350049139982118618 ) ) ;
#18825 = CARTESIAN_POINT ( 'NONE',  ( -6.594114490232312775, 87.46018628210146062, -6.840914352312096547 ) ) ;
#18826 = CARTESIAN_POINT ( 'NONE',  ( -56.70466238434235606, 244.2363183625454894, 7.500000000000000000 ) ) ;
#18827 = CARTESIAN_POINT ( 'NONE',  ( -9.500000000000005329, 126.0898137178985650, 0.1745138560723101806 ) ) ;
#18828 = CARTESIAN_POINT ( 'NONE',  ( 27.24356964375000700, 197.7406250006145285, 15.72908226750537075 ) ) ;
#18829 = CARTESIAN_POINT ( 'NONE',  ( 3.551475717527324030E-15, 210.0000000000000284, 28.99999999999999645 ) ) ;
#18830 = CARTESIAN_POINT ( 'NONE',  ( -1.926257025242585782E-15, 197.4968750006145513, -31.45816453501075927 ) ) ;
#18831 = DIRECTION ( 'NONE',  ( -0.000000000000000000, -1.000000000000000000, -0.000000000000000000 ) ) ;
#18832 = CARTESIAN_POINT ( 'NONE',  ( 26.99999999999999645, 243.9250000000000114, -7.347880794884117764E-16 ) ) ;
#18833 =( BOUNDED_CURVE ( )  B_SPLINE_CURVE ( 2, ( #3335, #4090, #1050, #21168, #27213, #6948, #672, #35170, #12243 ),
 .UNSPECIFIED., .F., .F. ) 
 B_SPLINE_CURVE_WITH_KNOTS ( ( 3, 2, 2, 2, 3 ),
 ( 0.2291666666666666574, 0.2361111111111111049, 0.2500000000000000000, 0.2638888888888888951, 0.2708333333333333703 ),
 .UNSPECIFIED. ) 
 CURVE ( )  GEOMETRIC_REPRESENTATION_ITEM ( )  RATIONAL_B_SPLINE_CURVE ( ( 0.9330127018922194093, 0.9330127018922194093, 1.000000000000000000, 0.8660254037844387076, 1.000000000000000000, 0.8660254037844387076, 1.000000000000000000, 0.9330127018922190762, 0.9330127018922194093 ) ) 
 REPRESENTATION_ITEM ( '' )  );
#18834 = CARTESIAN_POINT ( 'NONE',  ( -5.529263428287297444, 72.32731371789854791, -7.954856959092311719 ) ) ;
#18835 = ORIENTED_EDGE ( 'NONE', *, *, #35764, .F. ) ;
#18836 = CARTESIAN_POINT ( 'NONE',  ( 21.00000000000000000, 244.3187500012290627, 6.928203230275506996 ) ) ;
#18837 = CARTESIAN_POINT ( 'NONE',  ( -10.49813415416004858, 79.22731371789855359, 7.228626920338840023 ) ) ;
#18838 = CARTESIAN_POINT ( 'NONE',  ( 13.44051670066911441, -5.407089921784865361, -4.171874999385538629 ) ) ;
#18839 = CARTESIAN_POINT ( 'NONE',  ( -9.862825201705371470, 142.9999999999999716, 9.257821876896041857 ) ) ;
#18840 = CARTESIAN_POINT ( 'NONE',  ( 26.75643035624999655, 7.049594010296217766E-16, -4.078124999385480010 ) ) ;
#18841 = CARTESIAN_POINT ( 'NONE',  ( -8.962234695871565293, 44.43981371789855217, -8.715434833792128799 ) ) ;
#18842 = AXIS2_PLACEMENT_3D ( 'NONE', #7979, #13856, #16327 ) ;
#18843 = EDGE_LOOP ( 'NONE', ( #35272, #65 ) ) ;
#18844 = CARTESIAN_POINT ( 'NONE',  ( 15.24356964375000167, -3.323476615752272600, -7.303124999385448568 ) ) ;
#18845 = CARTESIAN_POINT ( 'NONE',  ( 21.00000000000000000, 245.3593750006145342, 6.646953231504538984 ) ) ;
#18846 = CARTESIAN_POINT ( 'NONE',  ( 2.660918448318279950, 15.29768628210143078, -12.46528703574805697 ) ) ;
#18847 = CARTESIAN_POINT ( 'NONE',  ( -36.53794563604517265, 205.3262412349648116, 4.842901733360249317 ) ) ;
#18848 = CARTESIAN_POINT ( 'NONE',  ( -48.80877896937850835, 211.6261429550004607, -6.530955311639245586 ) ) ;
#18849 = CARTESIAN_POINT ( 'NONE',  ( 36.59916218799832421, -3.464101615137751278, 159.4569602140672089 ) ) ;
#18850 = CARTESIAN_POINT ( 'NONE',  ( -11.48171059495408208, 70.31481371789854506, 4.944772684328421875 ) ) ;
#18851 = CARTESIAN_POINT ( 'NONE',  ( -53.17038769728823411, 208.6787018382581778, 4.469044688360752637 ) ) ;
#18852 = CARTESIAN_POINT ( 'NONE',  ( -57.32663769728823411, 204.3130714775002730, 3.149950860017883603 ) ) ;
#18853 = DIRECTION ( 'NONE',  ( 0.000000000000000000, 0.000000000000000000, 1.000000000000000000 ) ) ;
#18854 = CARTESIAN_POINT ( 'NONE',  ( 36.79853094953357129, 7.347880794884117764E-16, 161.7357555859521199 ) ) ;
#18855 = CARTESIAN_POINT ( 'NONE',  ( 15.46528703574811736, 66.00231371789855928, -3.257655550456947768 ) ) ;
#18856 = CARTESIAN_POINT ( 'NONE',  ( -46.23586230271182984, 205.8500491399821613, 7.418979330068642852 ) ) ;
#18857 = CARTESIAN_POINT ( 'NONE',  ( 20.99999999999999645, 185.0294372515228645, 0.000000000000000000 ) ) ;
#18858 = CARTESIAN_POINT ( 'NONE',  ( -2.660918448318275509, 65.89768628210146062, 12.46528703574805874 ) ) ;
#18859 = CARTESIAN_POINT ( 'NONE',  ( 2.908627838312118019, 28.52268628210144286, 15.53471296425195369 ) ) ;
#18860 = CARTESIAN_POINT ( 'NONE',  ( 22.56230152254412147, 3.464101615137759271, -0.6375000000000446976 ) ) ;
#18861 = CARTESIAN_POINT ( 'NONE',  ( -28.26183920611484979, 205.3333679525152888, -6.503129933765640303 ) ) ;
#18862 = AXIS2_PLACEMENT_3D ( 'NONE', #26906, #27099, #12689 ) ;
#18863 = ORIENTED_EDGE ( 'NONE', *, *, #37125, .F. ) ;
#18864 = CARTESIAN_POINT ( 'NONE',  ( -3.257655550457281723, 38.29768628210144499, 15.46528703574804986 ) ) ;
#18865 = CARTESIAN_POINT ( 'NONE',  ( 13.62178482187499640, 198.3031250006145285, -23.59362340125807123 ) ) ;
#18866 = CARTESIAN_POINT ( 'NONE',  ( 10.56230152254410903, 0.000000000000000000, -8.437499998771025744 ) ) ;
#18867 = DIRECTION ( 'NONE',  ( 1.000000000000000000, 0.000000000000000000, 0.000000000000000000 ) ) ;
#18868 = CARTESIAN_POINT ( 'NONE',  ( -35.95163769728823411, 215.6869285224996986, -3.149950860017881382 ) ) ;
#18869 = CARTESIAN_POINT ( 'NONE',  ( 31.33122385594975512, 6.928203230275514990, 168.0864290250503643 ) ) ;
#18870 = CARTESIAN_POINT ( 'NONE',  ( -4.622313124798576922, 23.63518628210144357, -11.61527771782819762 ) ) ;
#18871 = DIRECTION ( 'NONE',  ( -0.000000000000000000, -0.000000000000000000, 1.000000000000000000 ) ) ;
#18872 = CARTESIAN_POINT ( 'NONE',  ( -8.710071997420207879, 134.7148137178985507, 3.796722387233182339 ) ) ;
#18873 = CARTESIAN_POINT ( 'NONE',  ( 26.75643035624999655, 245.0968750006145456, 3.323476615752267271 ) ) ;
#18874 = EDGE_LOOP ( 'NONE', ( #8951, #16217, #28875, #32072, #27196, #6228, #3794, #23763, #20153, #4957, #24023, #32419, #8418, #35456, #18691, #1476, #26913, #26311, #18703, #5792, #34146, #2327, #3243, #19632, #6511, #16960 ) ) ;
#18875 = CARTESIAN_POINT ( 'NONE',  ( 20.99999999999999645, -6.928203230275506996, -7.031249998770932486 ) ) ;
#18876 = CARTESIAN_POINT ( 'NONE',  ( 11.48171059495408208, 139.3148137178985451, -4.944772684328420986 ) ) ;
#18877 = CARTESIAN_POINT ( 'NONE',  ( 22.80587116629410360, 7.646167579472015790E-16, -8.015624999385517313 ) ) ;
#18878 = CARTESIAN_POINT ( 'NONE',  ( 24.75271252598717808, 3.604726614523236616, 164.5306281710264216 ) ) ;
#18879 = LINE ( 'NONE', #35912, #10525 ) ;
#18880 = CARTESIAN_POINT ( 'NONE',  ( 13.49999999999999645, 196.7000000000000171, -23.38268590217984766 ) ) ;
#18881 = EDGE_CURVE ( 'NONE', #2700, #36053, #23613, .T. ) ;
#18882 = VERTEX_POINT ( 'NONE', #21053 ) ;
#18883 = CARTESIAN_POINT ( 'NONE',  ( 4.944772684328679446, 33.98518628210143788, -11.48171059495397373 ) ) ;
#18884 = ORIENTED_EDGE ( 'NONE', *, *, #10325, .T. ) ;
#18885 = EDGE_LOOP ( 'NONE', ( #12989, #36475 ) ) ;
#18886 = CARTESIAN_POINT ( 'NONE',  ( 24.58926402489574770, 0.000000000000000000, 159.8677550070055702 ) ) ;
#18887 = CARTESIAN_POINT ( 'NONE',  ( 20.99999999999999645, 185.0294372515228645, -5.999999999999999112 ) ) ;
#18888 = CARTESIAN_POINT ( 'NONE',  ( 10.56230152254463661, -3.464101615138067469, -9.412500000000033396 ) ) ;
#18889 = CARTESIAN_POINT ( 'NONE',  ( 14.99999999999978684, 3.464101615137630485, -5.887500000000001954 ) ) ;
#18890 = CARTESIAN_POINT ( 'NONE',  ( 23.87821517812500005, -4.985214923628404016, -8.090624999385454430 ) ) ;
#18891 = CIRCLE ( 'NONE', #7973, 2.649999999999985700 ) ;
#18892 = CARTESIAN_POINT ( 'NONE',  ( 8.715434833791931624, 82.86018628210145209, 8.962234695871760692 ) ) ;
#18893 = CARTESIAN_POINT ( 'NONE',  ( -14.38691631536207183, 131.7351862821014663, 5.770363421893814682 ) ) ;
#18894 = CARTESIAN_POINT ( 'NONE',  ( 10.56230152254446075, -3.464101615137956003, -3.899999998771003895 ) ) ;
#18895 = CARTESIAN_POINT ( 'NONE',  ( 17.03503949639500448, 220.5732280096259217, 4.520320870633568688 ) ) ;
#18896 = CARTESIAN_POINT ( 'NONE',  ( -56.92336230271183695, 213.9548777149308023, 2.149950860017852960 ) ) ;
#18897 = SURFACE_STYLE_USAGE ( .BOTH. , #16232 ) ;
#18898 = CARTESIAN_POINT ( 'NONE',  ( -9.000000000000024869, 210.0000000000000000, 0.000000000000000000 ) ) ;
#18899 = CARTESIAN_POINT ( 'NONE',  ( 28.32956640036948315, -5.196152422706632912, 168.1984670498039236 ) ) ;
#18900 = CARTESIAN_POINT ( 'NONE',  ( 2.311890736173452865, 137.8773137178986019, -12.53471296425189152 ) ) ;
#18901 = CARTESIAN_POINT ( 'NONE',  ( -43.07663769728823411, 204.3130714775002730, 3.149950860017883603 ) ) ;
#18902 = CARTESIAN_POINT ( 'NONE',  ( -59.89955436395489841, 216.3070033484980002, -6.137860380172975638 ) ) ;
#18903 = SHAPE_DEFINITION_REPRESENTATION ( #25892, #16167 ) ;
#18904 = CARTESIAN_POINT ( 'NONE',  ( 18.12178482187500350, -4.985214923628407568, -2.428124999385494753 ) ) ;
#18905 = CARTESIAN_POINT ( 'NONE',  ( -27.24356964375000345, 199.8031250006145285, 0.000000000000000000 ) ) ;
#18906 = CARTESIAN_POINT ( 'NONE',  ( 5.770363421894130873, 110.5648137178985593, -14.38691631536193860 ) ) ;
#18907 = CARTESIAN_POINT ( 'NONE',  ( -45.04836230271183695, 204.3130714775002446, -3.149950860017828091 ) ) ;
#18908 = EDGE_CURVE ( 'NONE', #7860, #8427, #24767, .T. ) ;
#18909 = ORIENTED_EDGE ( 'NONE', *, *, #19711, .F. ) ;
#18910 = CARTESIAN_POINT ( 'NONE',  ( -26.99999999999999645, 196.1000000012290627, 15.58845726811991561 ) ) ;
#18911 = CARTESIAN_POINT ( 'NONE',  ( -11.61527771782819940, 131.7351862821014663, 4.622313124798574258 ) ) ;
#18912 = LINE ( 'NONE', #33110, #18702 ) ;
#18913 = CARTESIAN_POINT ( 'NONE',  ( 37.24626209435294300, -3.604726614523238837, 164.0586977410752638 ) ) ;
#18914 = CARTESIAN_POINT ( 'NONE',  ( 13.04141134922759804, 100.9726862821014635, 8.927990412390657937 ) ) ;
#18915 = AXIS2_PLACEMENT_3D ( 'NONE', #25372, #28216, #19710 ) ;
#18916 = CARTESIAN_POINT ( 'NONE',  ( -59.30580436395489841, 216.5000000000000000, 0.1155267958017343610 ) ) ;
#18917 = CARTESIAN_POINT ( 'NONE',  ( 16.56230152254410726, -7.209453229046475009, -3.178124999385525395 ) ) ;
#18918 = CARTESIAN_POINT ( 'NONE',  ( -1.715153634034234598, 33.12268628210143362, -9.534712964251941258 ) ) ;
#18919 = CARTESIAN_POINT ( 'NONE',  ( 15.00000000000000000, 246.3625000000000114, -3.464101615137752610 ) ) ;
#18920 = CARTESIAN_POINT ( 'NONE',  ( -43.47247103062156981, 205.6499508600178956, 7.303452534266880569 ) ) ;
#18921 = CARTESIAN_POINT ( 'NONE',  ( 17.60716167209216110, -6.606202940439405147, -9.971823764164746251 ) ) ;
#18922 = CARTESIAN_POINT ( 'NONE',  ( -11.48171059495397373, 68.48518628210145209, -4.944772684328680334 ) ) ;
#18923 = DIRECTION ( 'NONE',  ( 1.000000000000000000, 0.000000000000000000, -0.000000000000000000 ) ) ;
#18924 = CARTESIAN_POINT ( 'NONE',  ( 1.255007937094097924E-14, 199.4375000000000284, -27.00000000000000000 ) ) ;
#18926 = CARTESIAN_POINT ( 'NONE',  ( 10.31873187879411091, -3.604726614523244610, -1.059374999385519933 ) ) ;
#18925 = CARTESIAN_POINT ( 'NONE',  ( 1.715153634034233487, 46.92268628210143788, 9.534712964251941258 ) ) ;
#18927 = EDGE_LOOP ( 'NONE', ( #26593, #19817, #25205, #27677 ) ) ;
#18928 = CARTESIAN_POINT ( 'NONE',  ( 18.00000000000000000, 5.196152422706630247, -1.874999999999987788 ) ) ;
#18929 = CARTESIAN_POINT ( 'NONE',  ( 24.55170959427540822, 3.604726614523240613, 162.2331541485523587 ) ) ;
#18930 = CARTESIAN_POINT ( 'NONE',  ( 36.75277418448394684, 3.464101615137759271, 161.2127533682296132 ) ) ;
#18931 = CARTESIAN_POINT ( 'NONE',  ( 26.99999999999999645, 245.7624999999999886, -3.464101615137755275 ) ) ;
#18932 = DIRECTION ( 'NONE',  ( -0.000000000000000000, -0.000000000000000000, -1.000000000000000000 ) ) ;
#18933 = CARTESIAN_POINT ( 'NONE',  ( 10.69584247140429589, 76.35231371789855359, 6.932735513424201024 ) ) ;
#18934 = CARTESIAN_POINT ( 'NONE',  ( 11.48171059495397728, 91.48518628210145209, 4.944772684328674117 ) ) ;
#18935 = ORIENTED_EDGE ( 'NONE', *, *, #31965, .T. ) ;
#18936 = VERTEX_POINT ( 'NONE', #6255 ) ;
#18937 = CARTESIAN_POINT ( 'NONE',  ( -27.00000000000000355, 198.7250000012290059, -15.58845726811989429 ) ) ;
#18938 = CARTESIAN_POINT ( 'NONE',  ( 20.99999999999999645, 6.928203230275506996, -1.012500000000014388 ) ) ;
#18939 = EDGE_CURVE ( 'NONE', #11516, #1318, #28628, .T. ) ;
#18940 = CARTESIAN_POINT ( 'NONE',  ( 5.770363421894130873, 55.36481371789856354, -14.38691631536193860 ) ) ;
#18941 = CARTESIAN_POINT ( 'NONE',  ( 26.75643035624999655, -3.323476615752267715, -5.465624999385500615 ) ) ;
#18942 = CARTESIAN_POINT ( 'NONE',  ( 18.12178482187500350, 245.8843750006145115, 4.985214923628407568 ) ) ;
#18943 = CARTESIAN_POINT ( 'NONE',  ( -51.78497103062156981, 206.1606490808709111, -2.350049139982163027 ) ) ;
#18944 = LINE ( 'NONE', #22525, #6453 ) ;
#18945 = CARTESIAN_POINT ( 'NONE',  ( -8.710071997420207879, 61.11481371789854933, 3.796722387233182339 ) ) ;
#18946 = CARTESIAN_POINT ( 'NONE',  ( 19.68408634441910721, 5.407089921784857367, -7.490624999385548044 ) ) ;
#18947 = AXIS2_PLACEMENT_3D ( 'NONE', #3929, #30313, #4337 ) ;
#18948 = CARTESIAN_POINT ( 'NONE',  ( -8.843639120294245259, 117.4648137178985650, -3.474262827703533230 ) ) ;
#18949 = CARTESIAN_POINT ( 'NONE',  ( 5.438367727407757144E-14, 198.0875000000000057, -27.00000000000000000 ) ) ;
#18950 = CARTESIAN_POINT ( 'NONE',  ( 2.660918448318002838, 31.50231371789854862, 12.46528703574811558 ) ) ;
#18951 = CARTESIAN_POINT ( 'NONE',  ( -10.49813415415989581, 77.97268628210144925, -7.228626920339068285 ) ) ;
#18952 = CARTESIAN_POINT ( 'NONE',  ( 13.56230152254411614, -5.196152422706632912, -7.462499998771049192 ) ) ;
#18953 = CARTESIAN_POINT ( 'NONE',  ( 1.069080835302379631E-14, 196.9624999999999773, 27.00000000000000000 ) ) ;
#18954 = CARTESIAN_POINT ( 'NONE',  ( 36.97989235558041798, 7.646167579472015790E-16, 161.0140776950323698 ) ) ;
#18955 = CARTESIAN_POINT ( 'NONE',  ( 10.31873187879411091, 3.604726614523240613, -6.984374999385522642 ) ) ;
#18956 = CARTESIAN_POINT ( 'NONE',  ( -27.00000000000000355, 197.7125000000000057, -15.58845726811989429 ) ) ;
#18957 = CARTESIAN_POINT ( 'NONE',  ( 29.54925929127992745, 5.908847637349538218, 159.6727443940304738 ) ) ;
#18958 = CARTESIAN_POINT ( 'NONE',  ( -1.715153634034234598, 97.52268628210144641, -9.534712964251941258 ) ) ;
#18959 = DIRECTION ( 'NONE',  ( 1.000000000000000000, 0.000000000000000000, 0.000000000000000000 ) ) ;
#18960 = EDGE_CURVE ( 'NONE', #1148, #7787, #32507, .T. ) ;
#18961 = CARTESIAN_POINT ( 'NONE',  ( 12.46528703574805874, 137.1976862821014720, 2.660918448318279950 ) ) ;
#18962 = CARTESIAN_POINT ( 'NONE',  ( -6.520765304352172720, 143.0000000000000284, 10.25440256910218828 ) ) ;
#18963 = CARTESIAN_POINT ( 'NONE',  ( 20.00041297495057080, 239.7473985277379143, -5.668978411116884608 ) ) ;
#18964 = ORIENTED_EDGE ( 'NONE', *, *, #21799, .T. ) ;
#18965 = CARTESIAN_POINT ( 'NONE',  ( 27.97700992647863316, 5.407089921784856479, 165.5660522374229799 ) ) ;
#18966 = CARTESIAN_POINT ( 'NONE',  ( 15.24356964375000167, -3.323476615752272600, -5.503124999385465621 ) ) ;
#18967 = CARTESIAN_POINT ( 'NONE',  ( -27.24356964374999279, 197.1968750006145115, 15.72908226750539384 ) ) ;
#18968 = CARTESIAN_POINT ( 'NONE',  ( 25.48152094116770883, 0.000000000000000000, 170.0662982274954800 ) ) ;
#18969 = CARTESIAN_POINT ( 'NONE',  ( 0.000000000000000000, 210.0000000000000284, 0.000000000000000000 ) ) ;
#18970 = CARTESIAN_POINT ( 'NONE',  ( 18.12178482187499640, 243.0343750006145456, -4.985214923628404904 ) ) ;
#18971 = CARTESIAN_POINT ( 'NONE',  ( -11.48171059495408208, 134.7148137178985507, 4.944772684328421875 ) ) ;
#18972 = CARTESIAN_POINT ( 'NONE',  ( -0.1745138560725500443, 139.2101862821014606, 12.50000000000000355 ) ) ;
#18974 = ORIENTED_EDGE ( 'NONE', *, *, #27471, .T. ) ;
#18973 = ORIENTED_EDGE ( 'NONE', *, *, #27448, .T. ) ;
#18975 = CARTESIAN_POINT ( 'NONE',  ( 18.12178482187500350, 243.5218750006145001, 4.985214923628407568 ) ) ;
#18976 = FACE_OUTER_BOUND ( 'NONE', #11913, .T. ) ;
#18977 = EDGE_CURVE ( 'NONE', #30621, #21071, #36386, .T. ) ;
#18978 = CARTESIAN_POINT ( 'NONE',  ( 21.00000000000000000, 6.646953231504538984, -4.303124999385465443 ) ) ;
#18979 = CARTESIAN_POINT ( 'NONE',  ( 8.632099005475788900, 110.8523137178985252, -13.23911966647199812 ) ) ;
#18980 = CARTESIAN_POINT ( 'NONE',  ( 22.56230152254411792, 7.347880794884125653E-16, -0.2250000000000584865 ) ) ;
#18981 = CARTESIAN_POINT ( 'NONE',  ( 15.00000000000000000, 0.000000000000000000, -8.493749998770949716 ) ) ;
#18982 = ORIENTED_EDGE ( 'NONE', *, *, #35212, .F. ) ;
#18983 = CARTESIAN_POINT ( 'NONE',  ( 13.44051670066911264, -5.407089921784865361, -5.521874999385528504 ) ) ;
#18984 =( BOUNDED_CURVE ( )  B_SPLINE_CURVE ( 2, ( #6913, #15627, #19046, #24347, #27557, #1396, #35889, #4056, #24157 ),
 .UNSPECIFIED., .F., .F. ) 
 B_SPLINE_CURVE_WITH_KNOTS ( ( 3, 2, 2, 2, 3 ),
 ( 0.3125000000000000000, 0.3194444444444444198, 0.3333333333333333148, 0.3472222222222222099, 0.3541666666666666852 ),
 .UNSPECIFIED. ) 
 CURVE ( )  GEOMETRIC_REPRESENTATION_ITEM ( )  RATIONAL_B_SPLINE_CURVE ( ( 0.9330127018922194093, 0.9330127018922194093, 1.000000000000000000, 0.8660254037844387076, 1.000000000000000000, 0.8660254037844387076, 1.000000000000000000, 0.9330127018922190762, 0.9330127018922194093 ) ) 
 REPRESENTATION_ITEM ( '' )  );
#18985 = VERTEX_POINT ( 'NONE', #6443 ) ;
#18986 = CARTESIAN_POINT ( 'NONE',  ( 13.62178482187501416, 196.8031250006145285, 23.59362340125806767 ) ) ;
#18987 = CARTESIAN_POINT ( 'NONE',  ( 8.715434833791931624, 138.0601862821014549, 8.962234695871760692 ) ) ;
#18988 = CARTESIAN_POINT ( 'NONE',  ( 16.56230152254411081, 7.209453229046475009, -0.7031249993855005487 ) ) ;
#18989 = CARTESIAN_POINT ( 'NONE',  ( 36.89981801693102170, 3.604726614523243278, 160.0988238161606034 ) ) ;
#18990 = EDGE_CURVE ( 'NONE', #29181, #6605, #26524, .T. ) ;
#18991 = CARTESIAN_POINT ( 'NONE',  ( -61.47544563604516554, 216.3070033484980854, 6.137860380172893926 ) ) ;
#18992 = CARTESIAN_POINT ( 'NONE',  ( 15.24356964374999990, 246.1468750006145285, 0.000000000000000000 ) ) ;
#18993 = CARTESIAN_POINT ( 'NONE',  ( 22.56230152254410015, 7.347880794884117764E-16, -7.312499998771010645 ) ) ;
#18994 = CARTESIAN_POINT ( 'NONE',  ( -33.37127896937850124, 214.5309553116392749, 1.090244570138288127 ) ) ;
#18995 = CARTESIAN_POINT ( 'NONE',  ( -4.622313124798576922, 134.0351862821014493, -11.61527771782819762 ) ) ;
#18996 = CARTESIAN_POINT ( 'NONE',  ( 22.56230152254411436, -3.464101615137751278, -1.499999998770977561 ) ) ;
#18997 = VERTEX_POINT ( 'NONE', #554 ) ;
#18998 = CARTESIAN_POINT ( 'NONE',  ( -27.24356964375000345, 199.8593750006145342, 0.000000000000000000 ) ) ;
#18999 = CARTESIAN_POINT ( 'NONE',  ( 19.56230152254412502, -5.196152422706635576, -8.850000000000052935 ) ) ;
#19000 = CARTESIAN_POINT ( 'NONE',  ( -13.23911966647218463, 122.2476862821014691, 8.632099005475506459 ) ) ;
#19001 = CARTESIAN_POINT ( 'NONE',  ( 7.954856959092191815, 110.1726862821014663, 5.529263428287477744 ) ) ;
#19002 = DIRECTION ( 'NONE',  ( 1.000000000000000000, 0.000000000000000000, 0.000000000000000000 ) ) ;
#19003 = CARTESIAN_POINT ( 'NONE',  ( 8.962234695871762469, 16.16018628210144570, -8.715434833791931624 ) ) ;
#19004 = CARTESIAN_POINT ( 'NONE',  ( 16.56230152254411436, -6.928203230275514990, -9.337500000000014566 ) ) ;
#19005 = ORIENTED_EDGE ( 'NONE', *, *, #19096, .T. ) ;
#19006 = CARTESIAN_POINT ( 'NONE',  ( 22.56230152254463306, -3.464101615137464840, -3.412500000000038725 ) ) ;
#19007 = CARTESIAN_POINT ( 'NONE',  ( 2.064181346179272847, 79.69768628210141515, -9.465287035748065847 ) ) ;
#19008 =( GEOMETRIC_REPRESENTATION_CONTEXT ( 3 ) GLOBAL_UNCERTAINTY_ASSIGNED_CONTEXT ( ( #35853 ) ) GLOBAL_UNIT_ASSIGNED_CONTEXT ( ( #9698, #15575, #967 ) ) REPRESENTATION_CONTEXT ( 'NONE', 'WORKASPACE' ) );
#19009 = FACE_OUTER_BOUND ( 'NONE', #12548, .T. ) ;
#19010 = CARTESIAN_POINT ( 'NONE',  ( -1.715153634034442431, 124.0773137178985621, 9.534712964251900402 ) ) ;
#19011 = CARTESIAN_POINT ( 'NONE',  ( 27.24356964375000700, 197.2906250006145399, 15.72908226750537075 ) ) ;
#19012 = CARTESIAN_POINT ( 'NONE',  ( 18.00000000000000355, -5.196152422706632912, -2.175000000000010481 ) ) ;
#19013 = CARTESIAN_POINT ( 'NONE',  ( -27.24356964375000345, 198.5093750006145399, 0.000000000000000000 ) ) ;
#19014 = EDGE_CURVE ( 'NONE', #22958, #36846, #12121, .T. ) ;
#19015 = CARTESIAN_POINT ( 'NONE',  ( 15.00000000000000000, 249.9625000000000057, -3.464101615137752610 ) ) ;
#19016 = VECTOR ( 'NONE', #21576, 1000.000000000000114 ) ;
#19017 = CARTESIAN_POINT ( 'NONE',  ( 23.99999999999999645, 242.1999999999999886, -5.196152422706631135 ) ) ;
#19018 = CARTESIAN_POINT ( 'NONE',  ( -7.954856959092309943, 60.82731371789854080, 5.529263428287300108 ) ) ;
#19019 = VERTEX_POINT ( 'NONE', #18016 ) ;
#19020 = CARTESIAN_POINT ( 'NONE',  ( 21.00000000000000000, 240.4937500012290457, -6.928203230275506996 ) ) ;
#19021 = CARTESIAN_POINT ( 'NONE',  ( 10.49813415416005213, 83.82731371789856212, -7.228626920338837358 ) ) ;
#19022 = CARTESIAN_POINT ( 'NONE',  ( 16.56230152254411081, -7.209453229046482114, -6.834374999385502747 ) ) ;
#19023 = CARTESIAN_POINT ( 'NONE',  ( -1.926257025242585782E-15, 199.6906250006145456, -31.45816453501075927 ) ) ;
#19024 = CARTESIAN_POINT ( 'NONE',  ( 18.12178482187500350, -4.985214923628407568, -6.028124999385486404 ) ) ;
#19025 = CARTESIAN_POINT ( 'NONE',  ( 0.1745138560722779009, 22.58981371789854720, 12.50000000000000355 ) ) ;
#19026 = EDGE_CURVE ( 'NONE', #28968, #19208, #24073, .T. ) ;
#19027 = APPLICATION_CONTEXT ( 'automotive_design' ) ;
#19028 = ORIENTED_EDGE ( 'NONE', *, *, #20721, .F. ) ;
#19029 = CARTESIAN_POINT ( 'NONE',  ( 26.75643035624999655, 3.323476615752271268, -7.078124999385466687 ) ) ;
#19030 = CARTESIAN_POINT ( 'NONE',  ( 0.1745138560725515708, 24.21018628210144641, -12.50000000000000355 ) ) ;
#19031 =( BOUNDED_CURVE ( )  B_SPLINE_CURVE ( 2, ( #21579, #30478, #18742, #7723, #4126, #16448, #25151 ),
 .UNSPECIFIED., .F., .F. ) 
 B_SPLINE_CURVE_WITH_KNOTS ( ( 3, 2, 2, 3 ),
 ( 0.5434782608695644113, 0.5507246376811587574, 0.5579710144927531035, 0.5652173913043473386 ),
 .UNSPECIFIED. ) 
 CURVE ( )  GEOMETRIC_REPRESENTATION_ITEM ( )  RATIONAL_B_SPLINE_CURVE ( ( 1.000000000000014433, 0.8660254037844243857, 1.000000000000000000, 0.8660254037844387076, 1.000000000000000000, 0.8660254037844469233, 0.9999999999999917843 ) ) 
 REPRESENTATION_ITEM ( '' )  );
#19032 = FACE_OUTER_BOUND ( 'NONE', #10228, .T. ) ;
#19033 = CARTESIAN_POINT ( 'NONE',  ( -50.39211230271182274, 203.5309553116391612, 1.857196546604092280 ) ) ;
#19034 = VECTOR ( 'NONE', #28675, 1000.000000000000000 ) ;
#19035 =( NAMED_UNIT ( * ) SI_UNIT ( $, .STERADIAN. ) SOLID_ANGLE_UNIT ( ) );
#19036 = PRODUCT_DEFINITION_FORMATION_WITH_SPECIFIED_SOURCE ( 'ANY', '', #28294, .NOT_KNOWN. ) ;
#19037 = CARTESIAN_POINT ( 'NONE',  ( 28.48305061405702787, 5.725134515572932514, 159.4403097883560179 ) ) ;
#19038 = CARTESIAN_POINT ( 'NONE',  ( -12.53471296425189152, 61.97731371789854649, -2.311890736173453753 ) ) ;
#19039 = CARTESIAN_POINT ( 'NONE',  ( -48.61830436395490551, 209.8844732041982297, 4.499999999999996447 ) ) ;
#19040 = AXIS2_PLACEMENT_3D ( 'NONE', #20447, #11527, #23096 ) ;
#19041 = CARTESIAN_POINT ( 'NONE',  ( -61.48288769728821990, 203.5309553116391612, -1.857196546604028775 ) ) ;
#19042 = CARTESIAN_POINT ( 'NONE',  ( 19.80074372294634344, 5.630122097104456991, -7.999999999999998224 ) ) ;
#19043 = CARTESIAN_POINT ( 'NONE',  ( 19.56230152254411792, -5.196152422706635576, -6.150000000000044764 ) ) ;
#19044 = CARTESIAN_POINT ( 'NONE',  ( -15.46528703574811736, 43.00231371789853796, 3.257655550456946436 ) ) ;
#19045 = CARTESIAN_POINT ( 'NONE',  ( -49.00669563604517265, 209.8844732041981729, -8.500000000000003553 ) ) ;
#19046 = CARTESIAN_POINT ( 'NONE',  ( -13.49999999999998401, 198.2750000000000057, 23.38268590217985476 ) ) ;
#19047 = CARTESIAN_POINT ( 'NONE',  ( 12.46528703574805874, 72.79768628210146630, 2.660918448318279950 ) ) ;
#19048 = CARTESIAN_POINT ( 'NONE',  ( -13.23911966647218463, 11.84768628210144747, 8.632099005475506459 ) ) ;
#19049 = CARTESIAN_POINT ( 'NONE',  ( 22.56230152254411792, 7.347880794884125653E-16, -2.025000000000027001 ) ) ;
#19050 =( BOUNDED_CURVE ( )  B_SPLINE_CURVE ( 2, ( #6420, #24970, #22150, #7553, #10203, #13052, #16462, #4512, #7367 ),
 .UNSPECIFIED., .F., .F. ) 
 B_SPLINE_CURVE_WITH_KNOTS ( ( 3, 2, 2, 2, 3 ),
 ( 0.07608695652173913526, 0.07971014492753622505, 0.08695652173913043237, 0.09420289855072463969, 0.09782608695652174335 ),
 .UNSPECIFIED. ) 
 CURVE ( )  GEOMETRIC_REPRESENTATION_ITEM ( )  RATIONAL_B_SPLINE_CURVE ( ( 0.9330127018922192983, 0.9330127018922194093, 1.000000000000000000, 0.8660254037844387076, 1.000000000000000000, 0.8660254037844387076, 1.000000000000000000, 0.9330127018922194093, 0.9330127018922194093 ) ) 
 REPRESENTATION_ITEM ( '' )  );
#19051 = DIRECTION ( 'NONE',  ( 1.000000000000000000, 0.000000000000000000, 0.000000000000000000 ) ) ;
#19052 = VERTEX_POINT ( 'NONE', #30512 ) ;
#19053 = CARTESIAN_POINT ( 'NONE',  ( -5.770363421893818234, 32.83518628210143930, -14.38691631536207005 ) ) ;
#19054 = CARTESIAN_POINT ( 'NONE',  ( -1.926257025242585782E-15, 196.9906250006145001, -31.45816453501076637 ) ) ;
#19055 = CARTESIAN_POINT ( 'NONE',  ( 5.778771075727756162E-15, 199.5218750006145854, 31.45816453501075927 ) ) ;
#19056 = CARTESIAN_POINT ( 'NONE',  ( 1.120210788295102201E-13, 195.8375000000000057, -27.00000000000000711 ) ) ;
#19057 = CARTESIAN_POINT ( 'NONE',  ( 6.225801843091343102, 50.65819137209577150, 3.000000000000000000 ) ) ;
#19058 = CARTESIAN_POINT ( 'NONE',  ( -4.944772684328673229, 10.98518628210143433, 11.48171059495397728 ) ) ;
#19059 = CARTESIAN_POINT ( 'NONE',  ( 18.12178482187499640, 247.5343750006145456, -4.985214923628404904 ) ) ;
#19060 = CARTESIAN_POINT ( 'NONE',  ( -9.500000000000005329, 107.6898137178985735, 0.1745138560723101806 ) ) ;
#19061 = CARTESIAN_POINT ( 'NONE',  ( 18.12178482187499640, 243.4843750006145342, -4.985214923628404904 ) ) ;
#19062 = ORIENTED_EDGE ( 'NONE', *, *, #30444, .F. ) ;
#19063 = DIRECTION ( 'NONE',  ( 0.000000000000000000, 0.000000000000000000, 1.000000000000000000 ) ) ;
#19064 = CARTESIAN_POINT ( 'NONE',  ( -6.000000000000000888, -30.00000000000000000, -19.99999999999999289 ) ) ;
#19065 = CARTESIAN_POINT ( 'NONE',  ( 19.68408634441910721, 5.407089921784857367, -8.840624999385537919 ) ) ;
#19066 = CARTESIAN_POINT ( 'NONE',  ( 34.09877069215784218, -5.407089921784855591, 163.9011702523720544 ) ) ;
#19067 = LINE ( 'NONE', #2542, #29257 ) ;
#19068 = CARTESIAN_POINT ( 'NONE',  ( 5.727106289114498080E-15, 197.4124999999999943, 31.17691453623979214 ) ) ;
#19069 = ORIENTED_EDGE ( 'NONE', *, *, #17007, .F. ) ;
#19070 = CARTESIAN_POINT ( 'NONE',  ( 10.49813415415989581, 36.57268628210144357, 7.228626920339069173 ) ) ;
#19071 = ORIENTED_EDGE ( 'NONE', *, *, #34130, .F. ) ;
#19072 = VERTEX_POINT ( 'NONE', #16668 ) ;
#19073 = CARTESIAN_POINT ( 'NONE',  ( 24.00000000000000000, -5.196152422706629359, -4.293749998770940657 ) ) ;
#19074 = DIRECTION ( 'NONE',  ( 0.000000000000000000, -1.000000000000000000, 0.000000000000000000 ) ) ;
#19075 = CARTESIAN_POINT ( 'NONE',  ( 1.069080835302379631E-14, 199.3250000012290286, 27.00000000000000000 ) ) ;
#19076 = CARTESIAN_POINT ( 'NONE',  ( -13.49999999999998401, 196.4750000000000227, 23.38268590217985476 ) ) ;
#19077 = CARTESIAN_POINT ( 'NONE',  ( 23.87821517812500005, -4.985214923628404016, -7.640624999385475569 ) ) ;
#19078 = CARTESIAN_POINT ( 'NONE',  ( 2.660918448318279950, 70.49768628210145494, -12.46528703574805697 ) ) ;
#19079 = CARTESIAN_POINT ( 'NONE',  ( 8.632099005475788900, 9.652313717898541867, -13.23911966647199812 ) ) ;
#19080 = CARTESIAN_POINT ( 'NONE',  ( -64.84002896937850835, 204.4285982733020433, 3.350049139982171020 ) ) ;
#19081 = CARTESIAN_POINT ( 'NONE',  ( 16.34449471652106567, 214.6555052834588935, 4.429144169335408776 ) ) ;
#19082 = CARTESIAN_POINT ( 'NONE',  ( -57.31919563604516554, 214.5000000000000284, -0.1155267958017627827 ) ) ;
#19083 =( LENGTH_UNIT ( ) NAMED_UNIT ( * ) SI_UNIT ( .MILLI., .METRE. ) );
#19084 = CARTESIAN_POINT ( 'NONE',  ( 28.21190614766015159, -5.196152422706632912, 166.8536042073800729 ) ) ;
#19085 = CARTESIAN_POINT ( 'NONE',  ( -11.61527771782809282, 117.4648137178985650, -4.622313124798832717 ) ) ;
#19086 = CARTESIAN_POINT ( 'NONE',  ( -42.48288769728824121, 203.5309553116391612, -1.857196546604028775 ) ) ;
#19087 = CARTESIAN_POINT ( 'NONE',  ( -54.95163769728822700, 217.4189793300686233, -4.149950860017907139 ) ) ;
#19088 = CARTESIAN_POINT ( 'NONE',  ( 26.75643035624999655, 7.049594010296217766E-16, -2.278124999385483740 ) ) ;
#19089 = CARTESIAN_POINT ( 'NONE',  ( -27.24356964375000345, 195.3031250006145285, 0.000000000000000000 ) ) ;
#19090 = CARTESIAN_POINT ( 'NONE',  ( -15.46528703574811736, 89.00231371789853085, 3.257655550456946436 ) ) ;
#19091 = CARTESIAN_POINT ( 'NONE',  ( -41.09002896937850124, 204.4285982733020433, 3.350049139982171020 ) ) ;
#19092 = VERTEX_POINT ( 'NONE', #33530 ) ;
#19093 = VECTOR ( 'NONE', #18262, 1000.000000000000000 ) ;
#19094 = FACE_OUTER_BOUND ( 'NONE', #32004, .T. ) ;
#19095 = CARTESIAN_POINT ( 'NONE',  ( 2.311890736173175753, 120.5226862821014606, 12.53471296425194836 ) ) ;
#19096 = EDGE_CURVE ( 'NONE', #3136, #26034, #4532, .T. ) ;
#19097 = CARTESIAN_POINT ( 'NONE',  ( -8.927990412390661490, 84.87268628210145494, 13.04141134922759804 ) ) ;
#19098 = AXIS2_PLACEMENT_3D ( 'NONE', #34610, #17193, #2589 ) ;
#19099 = DIRECTION ( 'NONE',  ( 0.9925324990730152175, -0.1219804832088933616, 0.000000000000000000 ) ) ;
#19100 = CARTESIAN_POINT ( 'NONE',  ( 37.29201885929546023, 3.604726614523243278, 164.5816999575734201 ) ) ;
#19101 = CARTESIAN_POINT ( 'NONE',  ( -5.770363421893818234, 78.83518628210146062, -14.38691631536207005 ) ) ;
#19102 = CARTESIAN_POINT ( 'NONE',  ( -56.13913769728823411, 206.8500491399821044, -5.686928522499717253 ) ) ;
#19103 = CARTESIAN_POINT ( 'NONE',  ( 10.31873187879411269, -3.604726614523240613, -4.603124999385506122 ) ) ;
#19104 = CARTESIAN_POINT ( 'NONE',  ( -3.474262827703337830, 32.83518628210143930, -8.843639120294326972 ) ) ;
#19105 = CARTESIAN_POINT ( 'NONE',  ( 10.56230152254443055, -3.464101615137944457, -7.612500000000054001 ) ) ;
#19106 = CARTESIAN_POINT ( 'NONE',  ( -34.56622103062156981, 212.1620413398628671, 8.530955311639223382 ) ) ;
#19107 = CARTESIAN_POINT ( 'NONE',  ( 22.56230152254410370, 7.347880794884117764E-16, -6.862499998771004250 ) ) ;
#19108 = CARTESIAN_POINT ( 'NONE',  ( -0.1745138560725500443, 65.61018628210145209, 12.50000000000000355 ) ) ;
#19109 = CARTESIAN_POINT ( 'NONE',  ( -27.00000000000000355, 199.9625000000000341, -15.58845726811989429 ) ) ;
#19110 = DIRECTION ( 'NONE',  ( 0.000000000000000000, 0.000000000000000000, 1.000000000000000000 ) ) ;
#19112 = CARTESIAN_POINT ( 'NONE',  ( 22.80587116629412492, 3.604726614523243278, -1.284374999385501814 ) ) ;
#19111 = CARTESIAN_POINT ( 'NONE',  ( -0.1745138560725182642, 47.21018628210144641, 9.500000000000005329 ) ) ;
#19113 = LINE ( 'NONE', #16262, #24010 ) ;
#19114 = ORIENTED_EDGE ( 'NONE', *, *, #29804, .T. ) ;
#19115 = CARTESIAN_POINT ( 'NONE',  ( 15.00000000000000000, 3.464101615137752166, -1.387499999999984190 ) ) ;
#19116 = CARTESIAN_POINT ( 'NONE',  ( 30.90225418466721763, -7.209453229046482114, 163.1832832459922713 ) ) ;
#19117 = CARTESIAN_POINT ( 'NONE',  ( 27.73146011565660984, -5.196152422706638241, 161.3620809329249539 ) ) ;
#19118 = CARTESIAN_POINT ( 'NONE',  ( 23.99999999999999645, 245.7999999999999829, -5.196152422706631135 ) ) ;
#19119 = CARTESIAN_POINT ( 'NONE',  ( 29.48995970988985604, 6.148715791637016537, 159.4803054849043917 ) ) ;
#19120 = EDGE_CURVE ( 'NONE', #11418, #18743, #31066, .T. ) ;
#19121 = CARTESIAN_POINT ( 'NONE',  ( 10.49813415416005213, 93.02731371789856496, -7.228626920338837358 ) ) ;
#19122 = CARTESIAN_POINT ( 'NONE',  ( -6.932735513423968321, 87.74768628210144072, -10.69584247140445221 ) ) ;
#19123 = ORIENTED_EDGE ( 'NONE', *, *, #30952, .T. ) ;
#19124 = ORIENTED_EDGE ( 'NONE', *, *, #30266, .T. ) ;
#19125 = VECTOR ( 'NONE', #21620, 1000.000000000000000 ) ;
#19126 = CARTESIAN_POINT ( 'NONE',  ( -27.00000000000000355, 197.3750000012290400, -15.58845726811989429 ) ) ;
#19127 = DIRECTION ( 'NONE',  ( 1.000000000000000000, 0.000000000000000000, 0.000000000000000000 ) ) ;
#19128 = CARTESIAN_POINT ( 'NONE',  ( 15.50000000000000533, 66.28981371789855359, -0.1745138560722452326 ) ) ;
#19129 = CARTESIAN_POINT ( 'NONE',  ( 26.75643035624999655, -3.323476615752267715, -5.915624999385464378 ) ) ;
#19130 = EDGE_CURVE ( 'NONE', #21667, #25349, #5081, .T. ) ;
#19131 = AXIS2_PLACEMENT_3D ( 'NONE', #8430, #14116, #25299 ) ;
#19132 = CARTESIAN_POINT ( 'NONE',  ( 15.24356964374999990, 244.9093750006145171, 0.000000000000000000 ) ) ;
#19133 = CARTESIAN_POINT ( 'NONE',  ( -54.95163769728822700, 213.9548777149308592, -2.149950860017830756 ) ) ;
#19134 = CARTESIAN_POINT ( 'NONE',  ( 37.41624727615045742, 7.347880794884125653E-16, 168.7962855074530069 ) ) ;
#19135 = CARTESIAN_POINT ( 'NONE',  ( 8.843639120294245259, 39.26481371789855501, 3.474262827703527901 ) ) ;
#19136 = CARTESIAN_POINT ( 'NONE',  ( 19.68408634441910721, -5.407089921784855591, -7.190624999385525129 ) ) ;
#19137 = CARTESIAN_POINT ( 'NONE',  ( 5.233372021372610483, 92.45231371789854791, -8.152565276336593669 ) ) ;
#19138 = CARTESIAN_POINT ( 'NONE',  ( -13.62178482187498396, 198.1343750006145399, 23.59362340125808188 ) ) ;
#19139 = CARTESIAN_POINT ( 'NONE',  ( -4.622313124798826500, 23.16481371789855359, 11.61527771782809637 ) ) ;
#19140 = CARTESIAN_POINT ( 'NONE',  ( -2.660918448318275509, 75.09768628210143504, 12.46528703574805874 ) ) ;
#19141 = CARTESIAN_POINT ( 'NONE',  ( 16.56230152254411081, -6.928203230275506996, -8.324999998771001941 ) ) ;
#19142 = CARTESIAN_POINT ( 'NONE',  ( 27.00000000000001421, 196.1375000000000171, 15.58845726811988897 ) ) ;
#19143 = CARTESIAN_POINT ( 'NONE',  ( 36.93740393099094632, -3.604726614523235284, 160.5284327797126025 ) ) ;
#19144 = CARTESIAN_POINT ( 'NONE',  ( 15.00000000000000000, 0.000000000000000000, -0.3937499987709536242 ) ) ;
#19145 = CARTESIAN_POINT ( 'NONE',  ( 10.31873187879410736, -3.604726614523244610, -6.459374999385468996 ) ) ;
#19146 = CARTESIAN_POINT ( 'NONE',  ( 30.88019288723065259, -6.928203230275514990, 162.9311214624255797 ) ) ;
#19147 = EDGE_CURVE ( 'NONE', #37366, #13899, #16108, .T. ) ;
#19148 = CARTESIAN_POINT ( 'NONE',  ( 3.796722387233379514, 98.38518628210145778, -8.710071997420127943 ) ) ;
#19149 = FACE_OUTER_BOUND ( 'NONE', #31266, .T. ) ;
#19150 = CIRCLE ( 'NONE', #25190, 8.000000000000000000 ) ;
#19151 = CARTESIAN_POINT ( 'NONE',  ( -11.61527771782819940, 122.5351862821014635, 4.622313124798574258 ) ) ;
#19152 = CARTESIAN_POINT ( 'NONE',  ( 16.56230152254411436, 6.928203230275514990, -4.612500000000012257 ) ) ;
#19153 = CARTESIAN_POINT ( 'NONE',  ( 15.24356964374999990, 240.2968750006145342, 0.000000000000000000 ) ) ;
#19154 = ORIENTED_EDGE ( 'NONE', *, *, #24982, .T. ) ;
#19155 = CARTESIAN_POINT ( 'NONE',  ( 31.10325711637897683, -7.209453229046475009, 165.4807572684663342 ) ) ;
#19156 = CARTESIAN_POINT ( 'NONE',  ( 18.12178482187499640, 4.985214923628404904, -6.065624999385454963 ) ) ;
#19158 = EDGE_CURVE ( 'NONE', #28452, #21721, #33068, .T. ) ;
#19157 = CARTESIAN_POINT ( 'NONE',  ( 27.24356964375000345, 198.7343750006145626, -3.336375036156643733E-15 ) ) ;
#19159 = CARTESIAN_POINT ( 'NONE',  ( 17.99789842368819848, 4.964426654962620589, -7.999999999999996447 ) ) ;
#19160 = CARTESIAN_POINT ( 'NONE',  ( 25.40308077269482112, 0.000000000000000000, 169.1697229992128939 ) ) ;
#19161 = DIRECTION ( 'NONE',  ( -0.000000000000000000, -1.000000000000000000, -0.000000000000000000 ) ) ;
#19162 = CARTESIAN_POINT ( 'NONE',  ( 26.75643035624999655, 243.2968750006145342, 3.323476615752267715 ) ) ;
#19163 = CARTESIAN_POINT ( 'NONE',  ( 1.715153634034445762, 9.077313717898549683, -9.534712964251895073 ) ) ;
#19164 = CARTESIAN_POINT ( 'NONE',  ( -27.24356964374999279, 195.3968750006145285, 15.72908226750539384 ) ) ;
#19166 = ORIENTED_EDGE ( 'NONE', *, *, #34621, .T. ) ;
#19165 = VERTEX_POINT ( 'NONE', #1872 ) ;
#19167 = CARTESIAN_POINT ( 'NONE',  ( 21.00000000000000000, 244.9093750006145456, 6.646953231504538984 ) ) ;
#19168 = AXIS2_PLACEMENT_3D ( 'NONE', #4573, #1540, #16149 ) ;
#19169 = EDGE_CURVE ( 'NONE', #9189, #19165, #4229, .T. ) ;
#19170 = CARTESIAN_POINT ( 'NONE',  ( -0.1745138560722763466, 8.789813717898553591, -12.50000000000000355 ) ) ;
#19171 = CARTESIAN_POINT ( 'NONE',  ( 18.12178482187500350, -4.985214923628407568, -3.215624999385463312 ) ) ;
#19172 = CARTESIAN_POINT ( 'NONE',  ( 11.08355503943118769, 104.2398137178985706, 10.83675517735179028 ) ) ;
#19173 = CARTESIAN_POINT ( 'NONE',  ( 15.00000000000000000, 0.000000000000000000, -8.943749998770956111 ) ) ;
#19174 = CARTESIAN_POINT ( 'NONE',  ( 13.44051670066910731, 5.407089921784862696, -7.921874999385513760 ) ) ;
#19175 = VERTEX_POINT ( 'NONE', #22171 ) ;
#19176 = CARTESIAN_POINT ( 'NONE',  ( -13.50000000000000533, 198.2375000012290229, -23.38268590217984411 ) ) ;
#19177 = CARTESIAN_POINT ( 'NONE',  ( -10.69584247140444866, 122.2476862821014549, 6.932735513423972762 ) ) ;
#19178 = PLANE ( 'NONE',  #25676 ) ;
#19179 = AXIS2_PLACEMENT_3D ( 'NONE', #7774, #13271, #2076 ) ;
#19180 = EDGE_CURVE ( 'NONE', #590, #22708, #13443, .T. ) ;
#19181 = CARTESIAN_POINT ( 'NONE',  ( -54.15252896937849414, 205.6499508600178103, -7.303452534266820173 ) ) ;
#19182 = CARTESIAN_POINT ( 'NONE',  ( 15.24356964374999990, 245.2468750006145228, 0.000000000000000000 ) ) ;
#19183 = SHAPE_REPRESENTATION_RELATIONSHIP ( 'NONE' , 'NONE' ,  #201, #20554 ) ;
#19184 = CARTESIAN_POINT ( 'NONE',  ( -32.77752896937849414, 212.3500491399821613, 3.839350919129088435 ) ) ;
#19185 = CARTESIAN_POINT ( 'NONE',  ( 25.22662187717753568, 0.000000000000000000, 169.9474368419002985 ) ) ;
#19186 = CARTESIAN_POINT ( 'NONE',  ( 22.56230152254410370, 7.347880794884117764E-16, -2.362499998771028231 ) ) ;
#19187 = ORIENTED_EDGE ( 'NONE', *, *, #8048, .F. ) ;
#19188 = DIRECTION ( 'NONE',  ( 0.08715574274765143514, 0.000000000000000000, 0.9961946980917462113 ) ) ;
#19189 = CARTESIAN_POINT ( 'NONE',  ( 36.68087069682425039, 7.347880794884117764E-16, 160.3908927435282692 ) ) ;
#19190 = CARTESIAN_POINT ( 'NONE',  ( 5.770363421893814682, 120.2351862821014521, 14.38691631536207183 ) ) ;
#19191 = VECTOR ( 'NONE', #17445, 1000.000000000000000 ) ;
#19192 = ADVANCED_FACE ( 'NONE', ( #7757 ), #24811, .T. ) ;
#19193 = CARTESIAN_POINT ( 'NONE',  ( -77.00000000000002842, 210.0000000000000000, 5.000000000000000888 ) ) ;
#19194 = CARTESIAN_POINT ( 'NONE',  ( 4.622313124798573369, 9.835186282101449962, 11.61527771782819940 ) ) ;
#19195 = CARTESIAN_POINT ( 'NONE',  ( 22.56230152254412147, 7.347880794884125653E-16, -9.225000000000010303 ) ) ;
#19196 = ORIENTED_EDGE ( 'NONE', *, *, #1070, .F. ) ;
#19197 = CARTESIAN_POINT ( 'NONE',  ( 0.000000000000000000, 200.0000000000000000, -27.00000000000000355 ) ) ;
#19198 = CARTESIAN_POINT ( 'NONE',  ( 5.233372021372432847, 83.14768628210143220, 8.152565276336710909 ) ) ;
#19199 = CYLINDRICAL_SURFACE ( 'NONE', #36346, 5.999999999999998224 ) ;
#19200 = CARTESIAN_POINT ( 'NONE',  ( -3.474262827703527901, 124.3648137178985849, 8.843639120294245259 ) ) ;
#19201 = CARTESIAN_POINT ( 'NONE',  ( -13.62178482187498396, 197.1781250006145569, 23.59362340125808188 ) ) ;
#19202 = CARTESIAN_POINT ( 'NONE',  ( 18.00000000000000000, 244.9749999999999943, -5.196152422706630247 ) ) ;
#19203 = CARTESIAN_POINT ( 'NONE',  ( 13.62178482187499640, 198.3593750006145342, -23.59362340125807123 ) ) ;
#19204 = CARTESIAN_POINT ( 'NONE',  ( 20.99999999999999289, 249.8874999999999886, -5.999999999999997335 ) ) ;
#19205 = CARTESIAN_POINT ( 'NONE',  ( 20.99999999999999645, 0.000000000000000000, -8.000000000000000000 ) ) ;
#19206 = CARTESIAN_POINT ( 'NONE',  ( -9.465287035748106703, 52.20231371789854080, 2.064181346179061460 ) ) ;
#19207 = CARTESIAN_POINT ( 'NONE',  ( 18.00000000000000000, 5.196152422706630247, -9.074999999999999289 ) ) ;
#19208 = VERTEX_POINT ( 'NONE', #19338 ) ;
#19209 = EDGE_CURVE ( 'NONE', #28635, #24921, #4728, .T. ) ;
#19210 = AXIS2_PLACEMENT_3D ( 'NONE', #22811, #16937, #14791 ) ;
#19211 = CARTESIAN_POINT ( 'NONE',  ( 26.99999999999999645, 242.1437500012290513, 3.464101615137751278 ) ) ;
#19212 = CARTESIAN_POINT ( 'NONE',  ( 4.944772684328420986, 58.81481371789855217, 11.48171059495408208 ) ) ;
#19213 = CARTESIAN_POINT ( 'NONE',  ( 13.44051670066911441, -5.407089921784865361, -7.321874999385524774 ) ) ;
#19214 = CARTESIAN_POINT ( 'NONE',  ( -1.926257025242585782E-15, 199.2406250006145285, -31.45816453501075927 ) ) ;
#19215 = CARTESIAN_POINT ( 'NONE',  ( 23.87821517812500005, -4.985214923628404016, -6.403124999385473082 ) ) ;
#19216 = CARTESIAN_POINT ( 'NONE',  ( -11.48171059495408208, 33.51481371789854791, 4.944772684328421875 ) ) ;
#19217 = ORIENTED_EDGE ( 'NONE', *, *, #13142, .T. ) ;
#19218 = UNCERTAINTY_MEASURE_WITH_UNIT (LENGTH_MEASURE( 1.000000000000000082E-05 ), #17902, 'distance_accuracy_value', 'NONE');
#19219 = CARTESIAN_POINT ( 'NONE',  ( 31.00765816110621031, -6.928203230275506996, 164.3880562096091467 ) ) ;
#19220 = AXIS2_PLACEMENT_3D ( 'NONE', #36119, #2686, #28834 ) ;
#19221 = CARTESIAN_POINT ( 'NONE',  ( 3.253724281355069334E-15, 199.8875000000000455, -27.00000000000000000 ) ) ;
#19222 = CARTESIAN_POINT ( 'NONE',  ( 37.63846293671737442, -3.604726614523238837, 168.5415738824881373 ) ) ;
#19223 = CARTESIAN_POINT ( 'NONE',  ( -53.55877896937850124, 211.6261429550004607, -6.530955311639245586 ) ) ;
#19224 = ADVANCED_BREP_SHAPE_REPRESENTATION ( '', ( #8321, #17215 ), #2050 ) ;
#19225 = CARTESIAN_POINT ( 'NONE',  ( 10.56230152254357968, 3.464101615137450185, -9.487500000000061107 ) ) ;
#19226 = CARTESIAN_POINT ( 'NONE',  ( -2.311890736173448424, 68.87731371789855928, 12.53471296425189330 ) ) ;
#19227 = CARTESIAN_POINT ( 'NONE',  ( -33.57663769728823411, 206.0451222850691408, 2.149950860017832532 ) ) ;
#19228 = CARTESIAN_POINT ( 'NONE',  ( -62.47247103062156981, 206.6499508600178672, 5.571401726697986057 ) ) ;
#19229 = CARTESIAN_POINT ( 'NONE',  ( 1.069080835302379631E-14, 197.9750000012290343, 27.00000000000000000 ) ) ;
#19230 = CARTESIAN_POINT ( 'NONE',  ( -70.80918835584510873, 215.2843023367891249, -5.000000000000000888 ) ) ;
#19231 = CARTESIAN_POINT ( 'NONE',  ( 15.50000000000000533, 47.88981371789855501, -0.1745138560722452326 ) ) ;
#19232 = CARTESIAN_POINT ( 'NONE',  ( -32.18377896937850124, 207.8379586601372750, 8.530955311639258909 ) ) ;
#19233 = CARTESIAN_POINT ( 'NONE',  ( 11.61527771782819940, 25.93518628210143717, -4.622313124798573369 ) ) ;
#19234 = CARTESIAN_POINT ( 'NONE',  ( 15.02283181144952628, 7.347880794884122694E-16, 50.52293445648592751 ) ) ;
#19235 = CARTESIAN_POINT ( 'NONE',  ( -12.53471296425194836, 67.62268628210145494, 2.311890736173176641 ) ) ;
#19236 = EDGE_CURVE ( 'NONE', #23945, #7924, #13706, .T. ) ;
#19237 = CARTESIAN_POINT ( 'NONE',  ( 13.04141134922759804, 8.972686282101431487, 8.927990412390657937 ) ) ;
#19238 = CARTESIAN_POINT ( 'NONE',  ( 16.56230152254411436, 6.928203230275514990, -2.362500000000001155 ) ) ;
#19239 = CARTESIAN_POINT ( 'NONE',  ( -28.94388556517004929, 202.2057090852030399, -1.821689022226129051 ) ) ;
#19240 = ORIENTED_EDGE ( 'NONE', *, *, #22220, .T. ) ;
#19241 = CARTESIAN_POINT ( 'NONE',  ( 13.23911966647218996, 25.64768628210144286, -8.632099005475504683 ) ) ;
#19242 = CIRCLE ( 'NONE', #35557, 3.500000000000002665 ) ;
#19243 = CARTESIAN_POINT ( 'NONE',  ( 27.24356964374999279, 196.0156250006145342, -15.72908226750539207 ) ) ;
#19244 = CARTESIAN_POINT ( 'NONE',  ( -27.24356964375000345, 197.6093750006145342, 0.000000000000000000 ) ) ;
#19245 = CARTESIAN_POINT ( 'NONE',  ( 26.99999999999999645, 247.5625000000000000, -3.464101615137755275 ) ) ;
#19246 = CARTESIAN_POINT ( 'NONE',  ( 20.99999999999999645, 185.0294372515228645, -5.999999999999999112 ) ) ;
#19247 = CARTESIAN_POINT ( 'NONE',  ( 7.234628195640322446, 195.6325961894323484, 26.99999999999999645 ) ) ;
#19248 = CARTESIAN_POINT ( 'NONE',  ( -12.50000000000000355, 3.510186282101451560, -0.1745138560725492671 ) ) ;
#19249 = APPLICATION_CONTEXT ( 'automotive_design' ) ;
#19250 = CARTESIAN_POINT ( 'NONE',  ( 18.12178482187499640, 247.0843750006145285, -4.985214923628404904 ) ) ;
#19251 = CARTESIAN_POINT ( 'NONE',  ( 7.954856959092311719, 120.6273137178985451, -5.529263428287300108 ) ) ;
#19252 = CARTESIAN_POINT ( 'NONE',  ( 15.24356964375000167, 243.1468750006145285, 3.323476615752272600 ) ) ;
#19253 = ORIENTED_EDGE ( 'NONE', *, *, #15680, .T. ) ;
#19254 = CARTESIAN_POINT ( 'NONE',  ( 20.99999999999999289, 249.4937500012290457, -5.999999999999998224 ) ) ;
#19255 = CARTESIAN_POINT ( 'NONE',  ( 18.00000000000000000, 249.5312500012290684, -5.196152422706630247 ) ) ;
#19256 = CARTESIAN_POINT ( 'NONE',  ( -8.962234695871565293, 108.8398137178985507, -8.715434833792128799 ) ) ;
#19257 = CARTESIAN_POINT ( 'NONE',  ( 22.80587116629411071, 3.604726614523238837, -9.328124999385510208 ) ) ;
#19258 = CARTESIAN_POINT ( 'NONE',  ( 34.07262396933355575, 5.407089921784857367, 163.6023118429445162 ) ) ;
#19259 =( BOUNDED_CURVE ( )  B_SPLINE_CURVE ( 2, ( #21286, #6675, #12553, #18059, #24307, #15402, #3639, #30174, #26567 ),
 .UNSPECIFIED., .F., .F. ) 
 B_SPLINE_CURVE_WITH_KNOTS ( ( 3, 2, 2, 2, 3 ),
 ( 0.03260869565217391908, 0.03623188405797101580, 0.04347826086956521618, 0.05072463768115942351, 0.05434782608695652717 ),
 .UNSPECIFIED. ) 
 CURVE ( )  GEOMETRIC_REPRESENTATION_ITEM ( )  RATIONAL_B_SPLINE_CURVE ( ( 0.9330127018922192983, 0.9330127018922194093, 1.000000000000000000, 0.8660254037844387076, 1.000000000000000000, 0.8660254037844387076, 1.000000000000000000, 0.9330127018922192983, 0.9330127018922194093 ) ) 
 REPRESENTATION_ITEM ( '' )  );
#19260 = CARTESIAN_POINT ( 'NONE',  ( 26.99999999999999645, 197.5624999999999716, -15.58845726811990495 ) ) ;
#19261 = ORIENTED_EDGE ( 'NONE', *, *, #13347, .F. ) ;
#19262 = CARTESIAN_POINT ( 'NONE',  ( 11.61527771782819940, 35.13518628210143646, -4.622313124798573369 ) ) ;
#19263 = ORIENTED_EDGE ( 'NONE', *, *, #15354, .F. ) ;
#19264 = ORIENTED_EDGE ( 'NONE', *, *, #3349, .F. ) ;
#19265 = CARTESIAN_POINT ( 'NONE',  ( 26.99999999999999645, -3.464101615137751278, -3.806249998770967480 ) ) ;
#19266 = CARTESIAN_POINT ( 'NONE',  ( 22.56230152254410370, 0.000000000000000000, 0.000000000000000000 ) ) ;
#19267 = CARTESIAN_POINT ( 'NONE',  ( 24.00000000000000000, -5.196152422706629359, -1.200000000000006617 ) ) ;
#19268 = LINE ( 'NONE', #7501, #37163 ) ;
#19269 = CARTESIAN_POINT ( 'NONE',  ( 26.75643035624999655, 249.1093750006145058, -3.323476615752271712 ) ) ;
#19270 = CARTESIAN_POINT ( 'NONE',  ( -12.46528703574805697, 68.19768628210144357, -2.660918448318280838 ) ) ;
#19271 = CARTESIAN_POINT ( 'NONE',  ( 8.632099005475504683, 138.3476862821014208, 13.23911966647218996 ) ) ;
#19272 = CARTESIAN_POINT ( 'NONE',  ( -59.49627896937850124, 203.4690446883607535, -1.626142955000504209 ) ) ;
#19273 = CARTESIAN_POINT ( 'NONE',  ( 14.20575797956217734, 216.7942420204455232, -0.4629122958956893297 ) ) ;
#19274 = CARTESIAN_POINT ( 'NONE',  ( -53.36086230271183695, 212.1499508600178387, -3.954877714930852495 ) ) ;
#19275 = VECTOR ( 'NONE', #35701, 1000.000000000000000 ) ;
#19276 = CARTESIAN_POINT ( 'NONE',  ( 25.13507686385291251, 3.464101615137752166, 166.1064243038051131 ) ) ;
#19277 = CARTESIAN_POINT ( 'NONE',  ( 11.61527771782809637, 131.2648137178985621, 4.622313124798827388 ) ) ;
#19278 = CARTESIAN_POINT ( 'NONE',  ( -33.97247103062156270, 206.6499508600178672, 5.571401726697986057 ) ) ;
#19279 = CARTESIAN_POINT ( 'NONE',  ( -61.87872103062156981, 201.4690446883607819, 2.162041339862843525 ) ) ;
#19280 =( BOUNDED_CURVE ( )  B_SPLINE_CURVE ( 2, ( #6165, #35151, #3133, #31574, #15075, #34971, #5597, #17739, #23420 ),
 .UNSPECIFIED., .F., .F. ) 
 B_SPLINE_CURVE_WITH_KNOTS ( ( 3, 2, 2, 2, 3 ),
 ( 0.9456521739130434590, 0.9492753623188405765, 0.9565217391304348116, 0.9637681159420289356, 0.9662082973083874204 ),
 .UNSPECIFIED. ) 
 CURVE ( )  GEOMETRIC_REPRESENTATION_ITEM ( )  RATIONAL_B_SPLINE_CURVE ( ( 0.9330127018922194093, 0.9330127018922194093, 1.000000000000000000, 0.8660254037844387076, 1.000000000000000000, 0.8660254037844387076, 1.000000000000000000, 0.9548847207714155072, 0.9401541335272467492 ) ) 
 REPRESENTATION_ITEM ( '' )  );
#19281 = CONTEXT_DEPENDENT_SHAPE_REPRESENTATION ( #15864, #2273 ) ;
#19282 = CARTESIAN_POINT ( 'NONE',  ( 15.24356964374999990, 3.323476615752268604, -1.190624999385493377 ) ) ;
#19283 = CARTESIAN_POINT ( 'NONE',  ( 27.24356964375000345, 197.3281250006145342, -3.336375036156643733E-15 ) ) ;
#19284 = AXIS2_PLACEMENT_3D ( 'NONE', #13127, #7999, #7442 ) ;
#19285 = CARTESIAN_POINT ( 'NONE',  ( 5.770363421894130873, 101.3648137178985706, -14.38691631536193860 ) ) ;
#19286 = CARTESIAN_POINT ( 'NONE',  ( -40.29836230271182984, 204.3130714775002446, -3.149950860017828091 ) ) ;
#19287 = VERTEX_POINT ( 'NONE', #10780 ) ;
#19288 = CARTESIAN_POINT ( 'NONE',  ( 25.25927379726847022, -3.464101615137840984, 167.5260017485858555 ) ) ;
#19289 = CARTESIAN_POINT ( 'NONE',  ( -12.53471296425194836, 122.8226862821014720, 2.311890736173176641 ) ) ;
#19290 = CARTESIAN_POINT ( 'NONE',  ( -13.04141134922759804, 59.57268628210145067, -8.927990412390657937 ) ) ;
#19291 = DIRECTION ( 'NONE',  ( 0.000000000000000000, 0.000000000000000000, 1.000000000000000000 ) ) ;
#19292 = CARTESIAN_POINT ( 'NONE',  ( 37.16782192588006239, -3.604726614523238837, 163.1621225127927062 ) ) ;
#19293 = CARTESIAN_POINT ( 'NONE',  ( -8.632099005475501130, 87.74768628210144072, -13.23911966647218996 ) ) ;
#19294 = CARTESIAN_POINT ( 'NONE',  ( -57.72247103062156270, 206.6499508600178672, 5.571401726697986057 ) ) ;
#19295 = CARTESIAN_POINT ( 'NONE',  ( 22.80587116629410716, 7.646167579472015790E-16, -6.215624999385549465 ) ) ;
#19296 = CARTESIAN_POINT ( 'NONE',  ( 8.152565276336714462, 34.84768628210143504, -5.233372021372432847 ) ) ;
#19297 = CARTESIAN_POINT ( 'NONE',  ( 23.99999999999999645, 5.196152422706631135, -2.793749998770966858 ) ) ;
#19298 = CARTESIAN_POINT ( 'NONE',  ( -59.10788769728823411, 216.4690446883607535, 1.857196546604031662 ) ) ;
#19299 = SURFACE_SIDE_STYLE ('',( #16442 ) ) ;
#19300 = EDGE_CURVE ( 'NONE', #16385, #10052, #15922, .T. ) ;
#19301 = CARTESIAN_POINT ( 'NONE',  ( 12.46528703574805874, 63.59768628210145636, 2.660918448318279950 ) ) ;
#19302 = CARTESIAN_POINT ( 'NONE',  ( -26.99999999999998934, 198.6875000000000284, 15.58845726811991561 ) ) ;
#19303 = CLOSED_SHELL ( 'NONE', ( #28817, #22699, #9125, #24105, #28247, #34689, #10527, #27897, #13114, #14120, #11063, #29122, #25455, #4128, #32530, #3585, #8016, #37211, #146, #4996, #33343, #22387, #27643, #11086, #20374, #22614, #7295, #34734, #21533, #36905, #15385, #6421, #7326, #6118, #17813, #25126, #31041, #8663, #24699, #120, #4844, #31412, #4674, #9035, #22476, #31826, #9248, #20240, #15065, #4761, #35498, #1579, #9711, #37428, #819, #16096, #2461, #13398, #30087, #2903, #3790, #24728, #35808, #13528, #13657, #1621, #21654, #20052, #35650, #35085, #25784, #10813, #37420, #24696, #29392, #18025, #21406, #35302, #29589, #26345, #21939, #13878, #32121, #24880, #37049, #28443, #9501, #36928, #16842, #36959, #6324, #14804, #29648, #24271, #25105, #31425, #6589, #16792, #557, #23698, #33034, #2183, #6455, #32343, #32858, #35641 ) ) ;
#19305 = CARTESIAN_POINT ( 'NONE',  ( 13.44051670066911264, -5.407089921784865361, -2.371874999385514826 ) ) ;
#19304 = CARTESIAN_POINT ( 'NONE',  ( 9.500000000000005329, 26.51018628210144001, 0.1745138560725188748 ) ) ;
#19306 = CARTESIAN_POINT ( 'NONE',  ( 15.00000000000000178, 241.9375000000000000, 3.464101615137757051 ) ) ;
#19307 = ORIENTED_EDGE ( 'NONE', *, *, #16918, .T. ) ;
#19308 = CARTESIAN_POINT ( 'NONE',  ( 24.00000000000000000, -5.196152422706629359, -2.549999999999996714 ) ) ;
#19309 = CARTESIAN_POINT ( 'NONE',  ( 20.99999999999999645, 247.4687500012290400, 5.999999999999998224 ) ) ;
#19310 = CARTESIAN_POINT ( 'NONE',  ( 30.94147426890365793, -7.209453229046482114, 163.6315708601335643 ) ) ;
#19311 = CARTESIAN_POINT ( 'NONE',  ( 24.85726793373765631, -3.464101615137761048, 162.9310537024133509 ) ) ;
#19312 = CARTESIAN_POINT ( 'NONE',  ( 18.00000000000000000, 243.1750000000000114, -5.196152422706630247 ) ) ;
#19313 = LINE ( 'NONE', #30851, #15454 ) ;
#19314 = CARTESIAN_POINT ( 'NONE',  ( -0.1745138560722763466, 91.58981371789856496, -12.50000000000000355 ) ) ;
#19315 = CARTESIAN_POINT ( 'NONE',  ( 4.944772684328679446, 89.18518628210145494, -11.48171059495397373 ) ) ;
#19316 = ORIENTED_EDGE ( 'NONE', *, *, #10646, .F. ) ;
#19317 = ORIENTED_EDGE ( 'NONE', *, *, #23727, .T. ) ;
#19318 = CARTESIAN_POINT ( 'NONE',  ( -13.50000000000000533, 198.2375000012290229, -23.38268590217984411 ) ) ;
#19319 = LINE ( 'NONE', #2221, #16273 ) ;
#19320 = CARTESIAN_POINT ( 'NONE',  ( 8.632099005475788900, 64.85231371789855359, -13.23911966647199812 ) ) ;
#19321 = EDGE_CURVE ( 'NONE', #32085, #16548, #19520, .T. ) ;
#19322 = CARTESIAN_POINT ( 'NONE',  ( 15.24356964374999990, 0.000000000000000000, -9.703124999385471128 ) ) ;
#19323 = CARTESIAN_POINT ( 'NONE',  ( 15.24356964374999990, 242.6593750006145171, 0.000000000000000000 ) ) ;
#19324 = CARTESIAN_POINT ( 'NONE',  ( -58.31622103062156981, 211.0902445701382533, 4.530955311639240257 ) ) ;
#19325 = DIRECTION ( 'NONE',  ( -0.000000000000000000, 1.000000000000000000, -0.000000000000000000 ) ) ;
#19326 = CARTESIAN_POINT ( 'NONE',  ( 3.796722387233182339, 40.41481371789855359, 8.710071997420207879 ) ) ;
#19327 = CARTESIAN_POINT ( 'NONE',  ( 10.31873187879411446, 3.604726614523236616, -6.928124999385510741 ) ) ;
#19328 = CARTESIAN_POINT ( 'NONE',  ( -5.529263428287297444, 99.92731371789854222, -7.954856959092311719 ) ) ;
#19329 = CARTESIAN_POINT ( 'NONE',  ( -1.926257025242585782E-15, 197.9468750006145399, -31.45816453501075927 ) ) ;
#19330 = CARTESIAN_POINT ( 'NONE',  ( 10.49813415416005213, 19.42731371789854933, -7.228626920338837358 ) ) ;
#19331 = CARTESIAN_POINT ( 'NONE',  ( 2.311890736173175753, 56.12268628210144072, 12.53471296425194836 ) ) ;
#19332 = CARTESIAN_POINT ( 'NONE',  ( 10.56230152254411259, 3.464101615137752166, -9.374999998770983112 ) ) ;
#19333 = CARTESIAN_POINT ( 'NONE',  ( 20.99999999999997513, 245.3875000000000455, -5.999999999999999112 ) ) ;
#19334 = CARTESIAN_POINT ( 'NONE',  ( 37.02238078016989675, 3.604726614523238837, 161.4997226103520802 ) ) ;
#19335 = CARTESIAN_POINT ( 'NONE',  ( 21.00000000000000000, 6.928203230275506996, -0.9562499987709413007 ) ) ;
#19336 = CARTESIAN_POINT ( 'NONE',  ( 19.68408634441911431, -5.407089921784861808, -5.446874999385537208 ) ) ;
#19337 = CARTESIAN_POINT ( 'NONE',  ( 22.56230152254446253, -3.464101615137556767, -1.612500000000025357 ) ) ;
#19338 = CARTESIAN_POINT ( 'NONE',  ( -70.80918835584509452, 215.2843023367891249, 5.000000000000000000 ) ) ;
#19339 = CARTESIAN_POINT ( 'NONE',  ( 6.840914352312096547, 89.76018628210145778, -6.594114490232313663 ) ) ;
#19340 = DIRECTION ( 'NONE',  ( 0.08715574274765150453, 0.000000000000000000, 0.9961946980917461003 ) ) ;
#19341 = CARTESIAN_POINT ( 'NONE',  ( 6.932735513423970097, 110.7476862821014549, 10.69584247140445044 ) ) ;
#19342 = CARTESIAN_POINT ( 'NONE',  ( -6.397436014819822603, 142.9999999999999432, 10.66666770903068162 ) ) ;
#19343 = CARTESIAN_POINT ( 'NONE',  ( 16.56230152254410726, 0.000000000000000000, -10.00000000000000000 ) ) ;
#19344 = ORIENTED_EDGE ( 'NONE', *, *, #35882, .F. ) ;
#19345 = CARTESIAN_POINT ( 'NONE',  ( 27.82012958953286130, 5.407089921784856479, 163.7729017808578362 ) ) ;
#19346 = CARTESIAN_POINT ( 'NONE',  ( 26.75643035624999655, 3.323476615752271712, -6.178124999385475213 ) ) ;
#19347 = CARTESIAN_POINT ( 'NONE',  ( -13.62178482187500528, 198.4343750006145228, -23.59362340125807123 ) ) ;
#19348 = FACE_OUTER_BOUND ( 'NONE', #30284, .T. ) ;
#19349 = CARTESIAN_POINT ( 'NONE',  ( 31.42927406654086298, -6.928203230275514990, 169.2071480604036253 ) ) ;
#19350 = DIRECTION ( 'NONE',  ( 0.000000000000000000, 0.000000000000000000, -1.000000000000000000 ) ) ;
#19351 = CARTESIAN_POINT ( 'NONE',  ( 20.00041297495047843, 239.8598985277378972, -5.668978411116867733 ) ) ;
#19352 = CARTESIAN_POINT ( 'NONE',  ( 19.56230152254411792, -5.196152422706629359, -6.937499998771023968 ) ) ;
#19353 = CARTESIAN_POINT ( 'NONE',  ( 11.61527771782809637, 140.4648137178985792, 4.622313124798827388 ) ) ;
#19354 = CARTESIAN_POINT ( 'NONE',  ( 27.24356964375000700, 195.5468750006145342, 15.72908226750537075 ) ) ;
#19356 = ORIENTED_EDGE ( 'NONE', *, *, #13571, .F. ) ;
#19355 = ORIENTED_EDGE ( 'NONE', *, *, #33739, .T. ) ;
#19357 = CARTESIAN_POINT ( 'NONE',  ( 18.12178482187499640, 245.1718750006145058, -4.985214923628404904 ) ) ;
#19358 = CARTESIAN_POINT ( 'NONE',  ( 12.53471296425189330, 11.37731371789854684, 2.311890736173451533 ) ) ;
#19359 = CARTESIAN_POINT ( 'NONE',  ( 26.75643035624999655, 3.323476615752271712, -3.028124999385441107 ) ) ;
#19360 = CARTESIAN_POINT ( 'NONE',  ( -13.23911966647199812, 117.7523137178985735, -8.632099005475788900 ) ) ;
#19361 = DIRECTION ( 'NONE',  ( -0.5887012860850802110, 0.8083506638593008775, 0.000000000000000000 ) ) ;
#19362 = EDGE_CURVE ( 'NONE', #11014, #32427, #21796, .T. ) ;
#19363 = CARTESIAN_POINT ( 'NONE',  ( 23.87821517812500005, -4.985214923628404016, -2.803124999385481431 ) ) ;
#19364 = CARTESIAN_POINT ( 'NONE',  ( 10.31873187879410558, 0.000000000000000000, -9.196874999385512339 ) ) ;
#19365 = ORIENTED_EDGE ( 'NONE', *, *, #5231, .F. ) ;
#19366 = CARTESIAN_POINT ( 'NONE',  ( -13.49999999999998401, 197.9375000012290400, 23.38268590217985476 ) ) ;
#19367 = CARTESIAN_POINT ( 'NONE',  ( 6.932735513423970097, 110.7476862821014549, 10.69584247140445044 ) ) ;
#19368 = CARTESIAN_POINT ( 'NONE',  ( 10.31873187879411269, -3.604726614523240613, -1.003124999385540450 ) ) ;
#19369 = CARTESIAN_POINT ( 'NONE',  ( -42.47544563604517265, 216.3070033484980854, 6.137860380172893926 ) ) ;
#19370 = CARTESIAN_POINT ( 'NONE',  ( 18.12178482187499640, 245.1718750006145058, -4.985214923628404904 ) ) ;
#19371 = CYLINDRICAL_SURFACE ( 'NONE', #7930, 10.00000000000000000 ) ;
#19372 = CARTESIAN_POINT ( 'NONE',  ( -67.61086230271183695, 213.1499508600178387, -5.686928522499747451 ) ) ;
#19373 = CARTESIAN_POINT ( 'NONE',  ( -10.49813415415989581, 114.7726862821014606, -7.228626920339068285 ) ) ;
#19374 = CARTESIAN_POINT ( 'NONE',  ( 19.56230152254410370, 5.196152422706631135, -0.9374999987709908833 ) ) ;
#19375 = ORIENTED_EDGE ( 'NONE', *, *, #27762, .T. ) ;
#19376 = CARTESIAN_POINT ( 'NONE',  ( -37.93080436395489841, 203.5000000000000000, -0.1155267958017335561 ) ) ;
#19377 = DIRECTION ( 'NONE',  ( 0.9961946980917462113, 0.000000000000000000, -0.08715574274765178209 ) ) ;
#19378 = FACE_OUTER_BOUND ( 'NONE', #11972, .T. ) ;
#19379 = CARTESIAN_POINT ( 'NONE',  ( 13.23911966647218996, 117.6476862821014322, -8.632099005475504683 ) ) ;
#19380 = EDGE_CURVE ( 'NONE', #28622, #4455, #31936, .T. ) ;
#19381 = CARTESIAN_POINT ( 'NONE',  ( 19.95811093400027403, 239.6067736145540152, -5.908846518073574750 ) ) ;
#19382 = CARTESIAN_POINT ( 'NONE',  ( -9.534712964251941258, 141.2226862821014493, 1.715153634034234154 ) ) ;
#19383 = CARTESIAN_POINT ( 'NONE',  ( 13.56230152254410548, 5.196152422706636465, -9.075000000000027711 ) ) ;
#19385 = ORIENTED_EDGE ( 'NONE', *, *, #27451, .T. ) ;
#19384 = AXIS2_PLACEMENT_3D ( 'NONE', #22583, #4762, #16711 ) ;
#19386 = CARTESIAN_POINT ( 'NONE',  ( 0.000000000000000000, 148.0000000000000000, 0.000000000000000000 ) ) ;
#19387 = CARTESIAN_POINT ( 'NONE',  ( 7.954856959092191815, 82.57268628210144357, 5.529263428287477744 ) ) ;
#19388 = CARTESIAN_POINT ( 'NONE',  ( 5.233372021372610483, 129.2523137178985451, -8.152565276336593669 ) ) ;
#19389 = CARTESIAN_POINT ( 'NONE',  ( -13.62178482187500528, 195.2281250006145399, -23.59362340125807123 ) ) ;
#19390 = DIRECTION ( 'NONE',  ( 0.000000000000000000, -0.000000000000000000, -1.000000000000000000 ) ) ;
#19391 = CARTESIAN_POINT ( 'NONE',  ( 13.62178482187501416, 199.1093750006145342, 23.59362340125806767 ) ) ;
#19392 = CARTESIAN_POINT ( 'NONE',  ( 16.56230152254410726, 0.000000000000000000, -10.00000000000000000 ) ) ;
#19393 = LINE ( 'NONE', #4775, #10304 ) ;
#19394 = CARTESIAN_POINT ( 'NONE',  ( -9.500000000000005329, 52.48981371789855643, 0.1745138560723101806 ) ) ;
#19395 = CARTESIAN_POINT ( 'NONE',  ( 18.91622499444735084, 5.725135169889072451, -9.986452812430625769 ) ) ;
#19396 = ORIENTED_EDGE ( 'NONE', *, *, #21864, .T. ) ;
#19397 = CARTESIAN_POINT ( 'NONE',  ( 26.99999999999999645, 242.1812500012290457, -7.347880794884117764E-16 ) ) ;
#19398 = CARTESIAN_POINT ( 'NONE',  ( 10.69584247140429589, 57.95231371789854791, 6.932735513424201024 ) ) ;
#19399 = CARTESIAN_POINT ( 'NONE',  ( 10.31873187879410736, 0.000000000000000000, -6.046874999385526195 ) ) ;
#19400 = CARTESIAN_POINT ( 'NONE',  ( 13.62178482187501416, 197.7031250006145342, 23.59362340125806767 ) ) ;
#19401 = CARTESIAN_POINT ( 'NONE',  ( 26.75643035624999655, -3.323476615752267715, -7.265624999385483562 ) ) ;
#19402 = CARTESIAN_POINT ( 'NONE',  ( 6.932735513424201024, 37.25231371789855217, -10.69584247140429412 ) ) ;
#19403 = ORIENTED_EDGE ( 'NONE', *, *, #5674, .F. ) ;
#19404 = CARTESIAN_POINT ( 'NONE',  ( 22.80587116629412492, 3.604726614523243278, -1.734374999385497551 ) ) ;
#19405 = CARTESIAN_POINT ( 'NONE',  ( -0.1745138560725500443, 10.41018628210144215, 12.50000000000000355 ) ) ;
#19406 = CARTESIAN_POINT ( 'NONE',  ( -44.05877896937847993, 211.6261429550004607, -6.530955311639245586 ) ) ;
#19407 = CARTESIAN_POINT ( 'NONE',  ( -0.1745138560722763466, 63.98981371789854933, -12.50000000000000355 ) ) ;
#19408 = CARTESIAN_POINT ( 'NONE',  ( -67.80877896937849414, 211.0902445701383101, -4.530955311639234040 ) ) ;
#19409 = CARTESIAN_POINT ( 'NONE',  ( -53.17038769728823411, 208.1428034533959703, 6.469044688360770401 ) ) ;
#19410 = CYLINDRICAL_SURFACE ( 'NONE', #34879, 5.999999999999998224 ) ;
#19411 = CARTESIAN_POINT ( 'NONE',  ( 22.56230152254411792, 7.347880794884125653E-16, -6.075000000000052580 ) ) ;
#19412 = CARTESIAN_POINT ( 'NONE',  ( -8.632099005475794229, 41.85231371789854649, 13.23911966647199812 ) ) ;
#19413 = CARTESIAN_POINT ( 'NONE',  ( -32.97544563604516554, 216.3070033484980854, 6.137860380172893926 ) ) ;
#19415 = CARTESIAN_POINT ( 'NONE',  ( 12.50000000000000355, 26.51018628210144357, 0.1745138560725507937 ) ) ;
#19414 = CIRCLE ( 'NONE', #9719, 4.000000000000001776 ) ;
#19416 = CYLINDRICAL_SURFACE ( 'NONE', #33381, 6.000000000000001776 ) ;
#19417 = CARTESIAN_POINT ( 'NONE',  ( -8.962234695871760692, 75.96018628210144641, 8.715434833791933400 ) ) ;
#19418 = CARTESIAN_POINT ( 'NONE',  ( 8.927990412390657937, 6.672686282101436106, -13.04141134922759804 ) ) ;
#19419 = CARTESIAN_POINT ( 'NONE',  ( 22.56230152254411792, 7.347880794884125653E-16, -1.125000000000042633 ) ) ;
#19420 = CARTESIAN_POINT ( 'NONE',  ( 21.00000000000000355, 0.000000000000000000, 50.00000000000001421 ) ) ;
#19421 = ORIENTED_EDGE ( 'NONE', *, *, #12862, .T. ) ;
#19422 = CARTESIAN_POINT ( 'NONE',  ( 15.46528703574804986, 35.99768628210143362, 3.257655550457285720 ) ) ;
#19423 = CARTESIAN_POINT ( 'NONE',  ( -27.24356964375000345, 195.3031250006145285, 0.000000000000000000 ) ) ;
#19424 = CARTESIAN_POINT ( 'NONE',  ( 13.62178482187501416, 199.1093750006145342, 23.59362340125806767 ) ) ;
#19425 = DIRECTION ( 'NONE',  ( 1.000000000000000000, 0.000000000000000000, 0.000000000000000000 ) ) ;
#19426 = CARTESIAN_POINT ( 'NONE',  ( 5.000000000000127010, 225.9999999999999432, -7.999999999999940492 ) ) ;
#19427 = CARTESIAN_POINT ( 'NONE',  ( 20.99999999999999645, 245.6125000000000114, 5.999999999999998224 ) ) ;
#19428 = CARTESIAN_POINT ( 'NONE',  ( 12.46528703574805874, 8.397686282101442856, 2.660918448318279950 ) ) ;
#19429 = CARTESIAN_POINT ( 'NONE',  ( 21.00000000000000000, 247.9468750006145399, -6.646953231504538984 ) ) ;
#19430 = CARTESIAN_POINT ( 'NONE',  ( 3.474262827703532341, 110.5648137178985593, -8.843639120294245259 ) ) ;
#19431 = CARTESIAN_POINT ( 'NONE',  ( 15.24356964374999990, 242.6218750006145228, -3.323476615752268604 ) ) ;
#19432 = VECTOR ( 'NONE', #3524, 1000.000000000000000 ) ;
#19433 = ORIENTED_EDGE ( 'NONE', *, *, #17548, .T. ) ;
#19434 = CARTESIAN_POINT ( 'NONE',  ( -68.80580436395490551, 216.5000000000000000, 0.1155267958017343610 ) ) ;
#19435 = SURFACE_STYLE_FILL_AREA ( #10882 ) ;
#19436 = CARTESIAN_POINT ( 'NONE',  ( 26.99999999999999645, 248.4437500012290343, 3.464101615137751278 ) ) ;
#19437 = CARTESIAN_POINT ( 'NONE',  ( -12.50000000000000355, 116.8898137178985621, 0.1745138560722786503 ) ) ;
#19438 = CARTESIAN_POINT ( 'NONE',  ( 22.80587116629410716, 7.646167579472015790E-16, -8.465624999385523708 ) ) ;
#19439 = CARTESIAN_POINT ( 'NONE',  ( 24.64158895398392701, -3.604726614523240613, 163.2604799309594910 ) ) ;
#19440 = CARTESIAN_POINT ( 'NONE',  ( 15.24356964374999990, 0.000000000000000000, -0.2531249993854844949 ) ) ;
#19441 = CARTESIAN_POINT ( 'NONE',  ( 13.50000000000001421, 196.5500000000000114, 23.38268590217984055 ) ) ;
#19442 = ORIENTED_EDGE ( 'NONE', *, *, #27777, .F. ) ;
#19443 = CARTESIAN_POINT ( 'NONE',  ( 6.932735513423970097, 37.14768628210143930, 10.69584247140445044 ) ) ;
#19444 = ORIENTED_EDGE ( 'NONE', *, *, #35164, .T. ) ;
#19445 = ORIENTED_EDGE ( 'NONE', *, *, #10047, .F. ) ;
#19446 = CARTESIAN_POINT ( 'NONE',  ( 15.00000000000000178, -3.464101615137757051, -4.406249998770951137 ) ) ;
#19447 = CARTESIAN_POINT ( 'NONE',  ( 15.24356964374999990, 3.323476615752268604, -2.878124999385485161 ) ) ;
#19448 = CARTESIAN_POINT ( 'NONE',  ( 16.56230152254411436, -6.928203230275514990, -4.387500000000030376 ) ) ;
#19449 = CARTESIAN_POINT ( 'NONE',  ( 7.234628195640269155, 195.1825961894323598, 27.00000000000003197 ) ) ;
#19450 = CARTESIAN_POINT ( 'NONE',  ( 18.12178482187500350, 248.4718750006145171, 4.985214923628407568 ) ) ;
#19451 = CARTESIAN_POINT ( 'NONE',  ( 4.944772684328679446, 52.38518628210145067, -11.48171059495397373 ) ) ;
#19452 = ADVANCED_FACE ( 'NONE', ( #11844 ), #26430, .F. ) ;
#19453 = EDGE_CURVE ( 'NONE', #27573, #11818, #23600, .T. ) ;
#19454 = FACE_BOUND ( 'NONE', #31295, .T. ) ;
#19455 = CARTESIAN_POINT ( 'NONE',  ( 15.61591388112560530, 224.3575629836672931, 2.655215585728335714 ) ) ;
#19456 = CARTESIAN_POINT ( 'NONE',  ( -60.28794563604517975, 206.7903428501025758, 3.378800118222471838 ) ) ;
#19457 = CARTESIAN_POINT ( 'NONE',  ( 27.96351228082934171, 5.196152422706630247, 164.0144493178186167 ) ) ;
#19458 = CARTESIAN_POINT ( 'NONE',  ( 0.1745138560722779009, 114.5898137178985650, 12.50000000000000355 ) ) ;
#19459 = CARTESIAN_POINT ( 'NONE',  ( -32.19122103062156981, 208.3738570449993404, -6.530955311639226935 ) ) ;
#19460 = CARTESIAN_POINT ( 'NONE',  ( -56.13913769728823411, 205.8500491399820760, -7.418979330068584233 ) ) ;
#19461 = EDGE_CURVE ( 'NONE', #11819, #14431, #37152, .T. ) ;
#19462 = AXIS2_PLACEMENT_3D ( 'NONE', #20853, #32771, #12497 ) ;
#19463 = CARTESIAN_POINT ( 'NONE',  ( 15.24356964374999990, 0.000000000000000000, -2.503124999385486493 ) ) ;
#19464 = CARTESIAN_POINT ( 'NONE',  ( -13.62178482187498396, 196.2781250006145228, 23.59362340125808188 ) ) ;
#19465 = CARTESIAN_POINT ( 'NONE',  ( 8.927990412390371944, 95.32731371789854791, 13.04141134922778811 ) ) ;
#19466 = CARTESIAN_POINT ( 'NONE',  ( -67.01711230271185116, 218.4690446883607535, -2.393094931466363651 ) ) ;
#19467 = ORIENTED_EDGE ( 'NONE', *, *, #1357, .T. ) ;
#19468 = CARTESIAN_POINT ( 'NONE',  ( 24.00000000000000000, -5.196152422706629359, -6.599999999999994316 ) ) ;
#19469 = CARTESIAN_POINT ( 'NONE',  ( 10.69584247140445221, 126.8476862821014635, -6.932735513423970097 ) ) ;
#19470 = CARTESIAN_POINT ( 'NONE',  ( 0.1745138560725837118, 70.21018628210144641, -15.50000000000000533 ) ) ;
#19471 = DIRECTION ( 'NONE',  ( 0.000000000000000000, -0.000000000000000000, 1.000000000000000000 ) ) ;
#19472 = CARTESIAN_POINT ( 'NONE',  ( 34.18538171151332961, 5.407089921784862696, 164.8911387336007408 ) ) ;
#19473 = CARTESIAN_POINT ( 'NONE',  ( 14.25334919248782661, 91.48518628210145209, 6.092822981423971385 ) ) ;
#19474 = CARTESIAN_POINT ( 'NONE',  ( -45.05580436395489841, 216.5000000000000000, 0.1155267958017343610 ) ) ;
#19475 = CARTESIAN_POINT ( 'NONE',  ( 19.68408634441910721, 5.407089921784857367, -7.040624999385541649 ) ) ;
#19476 =( BOUNDED_CURVE ( )  B_SPLINE_CURVE ( 2, ( #28449, #2853, #11767, #11, #11577, #20500, #17464 ),
 .UNSPECIFIED., .F., .F. ) 
 B_SPLINE_CURVE_WITH_KNOTS ( ( 3, 2, 2, 3 ),
 ( 0.2173913043478258034, 0.2246376811594198442, 0.2318840579710139127, 0.2391304347826079535 ),
 .UNSPECIFIED. ) 
 CURVE ( )  GEOMETRIC_REPRESENTATION_ITEM ( )  RATIONAL_B_SPLINE_CURVE ( ( 1.000000000000005107, 0.8660254037844334896, 1.000000000000000000, 0.8660254037844387076, 1.000000000000000000, 0.8660254037844525854, 0.9999999999999861222 ) ) 
 REPRESENTATION_ITEM ( '' )  );
#19477 = CARTESIAN_POINT ( 'NONE',  ( -8.710071997420127943, 13.28518628210143149, -3.796722387233380402 ) ) ;
#19478 = CARTESIAN_POINT ( 'NONE',  ( -64.25372103062154849, 216.5309553116391612, -1.626142955000564383 ) ) ;
#19479 = DIRECTION ( 'NONE',  ( 0.000000000000000000, 0.000000000000000000, 1.000000000000000000 ) ) ;
#19480 = CARTESIAN_POINT ( 'NONE',  ( -7.228626920339069173, 57.27268628210144641, 10.49813415415989581 ) ) ;
#19481 = CARTESIAN_POINT ( 'NONE',  ( -26.99999999999998934, 196.8875000000000171, 15.58845726811991561 ) ) ;
#19482 = FACE_OUTER_BOUND ( 'NONE', #16311, .T. ) ;
#19484 = CARTESIAN_POINT ( 'NONE',  ( 16.56230152254411436, 7.209453229046482114, -2.109374999385531080 ) ) ;
#19483 = CARTESIAN_POINT ( 'NONE',  ( -5.233372021372430183, 23.34768628210144570, -8.152565276336710909 ) ) ;
#19485 = CARTESIAN_POINT ( 'NONE',  ( 5.649999999999987921, 244.5000000000000000, 2.500000000000000000 ) ) ;
#19486 = ORIENTED_EDGE ( 'NONE', *, *, #23681, .F. ) ;
#19487 = CARTESIAN_POINT ( 'NONE',  ( 26.99999999999999645, -3.464101615137751278, -2.962500000000017675 ) ) ;
#19488 = CARTESIAN_POINT ( 'NONE',  ( 31.01746318205820785, 6.928203230275514990, 164.5001281119201053 ) ) ;
#19489 = VECTOR ( 'NONE', #1783, 1000.000000000000000 ) ;
#19490 = CARTESIAN_POINT ( 'NONE',  ( 27.46224632087531958, 5.407089921784862696, 159.6822773018186297 ) ) ;
#19491 = CARTESIAN_POINT ( 'NONE',  ( 19.68408634441910721, 5.407089921784857367, -1.640624999385525973 ) ) ;
#19492 = CARTESIAN_POINT ( 'NONE',  ( 27.63994658577156827, 5.196152422706636465, 160.3160764999286698 ) ) ;
#19493 = CARTESIAN_POINT ( 'NONE',  ( 26.99999999999999645, 243.8875000000000171, 3.464101615137751278 ) ) ;
#19494 = FACE_OUTER_BOUND ( 'NONE', #13614, .T. ) ;
#19495 = CARTESIAN_POINT ( 'NONE',  ( -10.69584247140429412, 80.95231371789856212, -6.932735513424201024 ) ) ;
#19496 = CARTESIAN_POINT ( 'NONE',  ( -11.61527771782819940, 94.93518628210145494, 4.622313124798574258 ) ) ;
#19497 = ORIENTED_EDGE ( 'NONE', *, *, #16324, .F. ) ;
#19498 = VERTEX_POINT ( 'NONE', #278 ) ;
#19499 = CARTESIAN_POINT ( 'NONE',  ( -27.00000000000000355, 198.2750000012290741, -15.58845726811989429 ) ) ;
#19500 = CARTESIAN_POINT ( 'NONE',  ( 34.22502607998692525, -5.196152422706635576, 166.7416000626326422 ) ) ;
#19501 = CARTESIAN_POINT ( 'NONE',  ( -15.53471296425188442, 52.77731371789855785, -2.908627838312459080 ) ) ;
#19502 = CARTESIAN_POINT ( 'NONE',  ( 21.00000000000000000, -6.646953231504538984, -10.04062499938548392 ) ) ;
#19503 = CARTESIAN_POINT ( 'NONE',  ( 18.12178482187499640, 243.4843750006145342, -4.985214923628404904 ) ) ;
#19504 =( BOUNDED_CURVE ( )  B_SPLINE_CURVE ( 2, ( #15813, #26799, #9559, #26610, #639, #3680, #15248 ),
 .UNSPECIFIED., .F., .F. ) 
 B_SPLINE_CURVE_WITH_KNOTS ( ( 3, 2, 2, 3 ),
 ( 0.04347826086956579905, 0.05072463768115918065, 0.05797101449275256224, 0.06521739130434593690 ),
 .UNSPECIFIED. ) 
 CURVE ( )  GEOMETRIC_REPRESENTATION_ITEM ( )  RATIONAL_B_SPLINE_CURVE ( ( 0.9999999999999892308, 0.8660254037844494768, 1.000000000000000000, 0.8660254037844387076, 1.000000000000000000, 0.8660254037844735686, 0.9999999999999651390 ) ) 
 REPRESENTATION_ITEM ( '' )  );
#19505 = CARTESIAN_POINT ( 'NONE',  ( -54.35788769728822700, 214.4690446883608104, 1.321298161741840893 ) ) ;
#19506 = CARTESIAN_POINT ( 'NONE',  ( 15.00000000000000000, 0.000000000000000000, -6.243749998770947940 ) ) ;
#19507 = CARTESIAN_POINT ( 'NONE',  ( -5.529263428287297444, 44.72731371789853938, -7.954856959092311719 ) ) ;
#19508 = CARTESIAN_POINT ( 'NONE',  ( -67.61830436395489130, 209.8844732041982581, 6.500000000000000888 ) ) ;
#19509 = CARTESIAN_POINT ( 'NONE',  ( -9.465287035748106703, 89.00231371789853085, 2.064181346179061460 ) ) ;
#19510 = CARTESIAN_POINT ( 'NONE',  ( 27.24356964375000700, 199.5968750006145456, 15.72908226750537075 ) ) ;
#19511 = CARTESIAN_POINT ( 'NONE',  ( -12.50000000000000355, 15.68981371789854329, 0.1745138560722786503 ) ) ;
#19512 = VECTOR ( 'NONE', #4344, 1000.000000000000114 ) ;
#19513 = CARTESIAN_POINT ( 'NONE',  ( 6.932735513423970097, 55.54768628210144499, 10.69584247140445044 ) ) ;
#19514 = CARTESIAN_POINT ( 'NONE',  ( 13.56230152254411436, -5.196152422706632912, -7.912499998771055587 ) ) ;
#19515 = CARTESIAN_POINT ( 'NONE',  ( 26.99999999999999645, 245.3125000000000000, -3.464101615137755275 ) ) ;
#19516 = CARTESIAN_POINT ( 'NONE',  ( 33.78501001826630556, -5.407089921784855591, 160.3148693392417670 ) ) ;
#19517 = CARTESIAN_POINT ( 'NONE',  ( 10.31873187879410558, 3.604726614523240613, -10.13437499938549280 ) ) ;
#19518 = CARTESIAN_POINT ( 'NONE',  ( 13.44051670066910908, 5.407089921784862696, -7.021874999385530280 ) ) ;
#19519 = DIRECTION ( 'NONE',  ( 1.000000000000000000, 0.000000000000000000, 0.000000000000000000 ) ) ;
#19520 = LINE ( 'NONE', #27472, #6669 ) ;
#19521 = CARTESIAN_POINT ( 'NONE',  ( 9.500000000000005329, 72.51018628210145778, 0.1745138560725188748 ) ) ;
#19522 = DIRECTION ( 'NONE',  ( -0.5887012860850800999, 0.8083506638593009885, 0.000000000000000000 ) ) ;
#19523 = CARTESIAN_POINT ( 'NONE',  ( -4.622313124798576922, 115.6351862821014578, -11.61527771782819762 ) ) ;
#19524 = CARTESIAN_POINT ( 'NONE',  ( 17.54540804174073187, 195.0000000000000000, -20.52215039046394907 ) ) ;
#19525 = DIRECTION ( 'NONE',  ( 0.000000000000000000, 0.000000000000000000, 1.000000000000000000 ) ) ;
#19526 = VERTEX_POINT ( 'NONE', #20764 ) ;
#19527 = CARTESIAN_POINT ( 'NONE',  ( 37.21194452064604974, -3.604726614523235284, 163.6664460787016253 ) ) ;
#19528 = CARTESIAN_POINT ( 'NONE',  ( 23.87821517812500005, -4.985214923628404016, -6.290624999385458160 ) ) ;
#19529 = CARTESIAN_POINT ( 'NONE',  ( -27.24356964375000345, 197.1218750006145513, -15.72908226750537786 ) ) ;
#19530 = CARTESIAN_POINT ( 'NONE',  ( 37.52080268400804641, -3.604726614523238837, 167.1967110400642866 ) ) ;
#19531 = CARTESIAN_POINT ( 'NONE',  ( 28.24132121073036927, -5.196152422706638241, 167.1898199167616781 ) ) ;
#19532 = CARTESIAN_POINT ( 'NONE',  ( 23.87821517812499650, 241.1593750006145171, -4.985214923628404904 ) ) ;
#19533 = DIRECTION ( 'NONE',  ( -0.1219804832088933616, -0.9925324990730152175, 0.000000000000000000 ) ) ;
#19534 = CARTESIAN_POINT ( 'NONE',  ( -12.53471296425189152, 135.5773137178985621, -2.311890736173453753 ) ) ;
#19535 = CARTESIAN_POINT ( 'NONE',  ( 4.622313124798573369, 138.6351862821014720, 11.61527771782819940 ) ) ;
#19537 = ORIENTED_EDGE ( 'NONE', *, *, #20756, .T. ) ;
#19536 = ORIENTED_EDGE ( 'NONE', *, *, #7794, .T. ) ;
#19538 =( BOUNDED_CURVE ( )  B_SPLINE_CURVE ( 2, ( #31529, #5554, #8596, #17139, #5742, #2899, #14471 ),
 .UNSPECIFIED., .F., .F. ) 
 B_SPLINE_CURVE_WITH_KNOTS ( ( 3, 2, 2, 3 ),
 ( 0.3043478260869560414, 0.3115942028985501655, 0.3188405797101442340, 0.3260869565217384136 ),
 .UNSPECIFIED. ) 
 CURVE ( )  GEOMETRIC_REPRESENTATION_ITEM ( )  RATIONAL_B_SPLINE_CURVE ( ( 1.000000000000009326, 0.8660254037844296038, 1.000000000000000000, 0.8660254037844387076, 1.000000000000000000, 0.8660254037844520303, 0.9999999999999866773 ) ) 
 REPRESENTATION_ITEM ( '' )  );
#19539 = CARTESIAN_POINT ( 'NONE',  ( 23.87821517812499650, 244.6468750006145285, -4.985214923628404904 ) ) ;
#19540 = CARTESIAN_POINT ( 'NONE',  ( 8.962234695871567070, 12.23981371789853512, 8.715434833792127023 ) ) ;
#19541 = CARTESIAN_POINT ( 'NONE',  ( 15.24356964374999990, 3.323476615752268604, -3.328124999385480898 ) ) ;
#19542 = CARTESIAN_POINT ( 'NONE',  ( 13.23911966647199812, 113.1523137178985650, 8.632099005475788900 ) ) ;
#19543 = CARTESIAN_POINT ( 'NONE',  ( 22.56230152254454424, -3.464101615137510137, -9.712500000000012790 ) ) ;
#19544 = CARTESIAN_POINT ( 'NONE',  ( 18.12178482187499640, 4.985214923628404904, -0.7781249993854821856 ) ) ;
#19545 = CARTESIAN_POINT ( 'NONE',  ( 19.68408634441910721, 5.407089921784862696, -9.346874999385523353 ) ) ;
#19546 = PRODUCT_DEFINITION_SHAPE ( 'NONE', 'NONE',  #28710 ) ;
#19547 = CARTESIAN_POINT ( 'NONE',  ( 13.49999999999999645, 199.0625000012290400, -23.38268590217984766 ) ) ;
#19548 = CARTESIAN_POINT ( 'NONE',  ( -4.622313124798576922, 115.6351862821014578, -11.61527771782819762 ) ) ;
#19549 = CARTESIAN_POINT ( 'NONE',  ( 22.80587116629410360, 3.604726614523238837, -3.478124999385532767 ) ) ;
#19550 = CARTESIAN_POINT ( 'NONE',  ( -46.03794563604517975, 203.8621396198271043, 6.307003348498029460 ) ) ;
#19551 = CARTESIAN_POINT ( 'NONE',  ( 26.75643035624999655, 244.1593750006145171, -3.323476615752271268 ) ) ;
#19552 = CARTESIAN_POINT ( 'NONE',  ( 0.000000000000000000, 200.0000000000000000, -27.00000000000000355 ) ) ;
#19553 = CARTESIAN_POINT ( 'NONE',  ( -36.34002896937849414, 206.1606490808709111, 2.350049139982143931 ) ) ;
#19554 = CARTESIAN_POINT ( 'NONE',  ( -4.622313124798576922, 124.8351862821014748, -11.61527771782819762 ) ) ;
#19555 = CARTESIAN_POINT ( 'NONE',  ( 19.56230152254410370, 5.196152422706631135, -1.837499998771002785 ) ) ;
#19556 = CARTESIAN_POINT ( 'NONE',  ( -45.45163769728822700, 215.6869285224996986, -3.149950860017881382 ) ) ;
#19557 = DIRECTION ( 'NONE',  ( 0.000000000000000000, 0.000000000000000000, 1.000000000000000000 ) ) ;
#19558 = CARTESIAN_POINT ( 'NONE',  ( -15.50000000000000533, 113.9101862821014493, -0.1745138560725808530 ) ) ;
#19559 = CARTESIAN_POINT ( 'NONE',  ( 15.00000000000000000, 0.000000000000000000, -7.143749998770959841 ) ) ;
#19560 = CARTESIAN_POINT ( 'NONE',  ( -8.962234695871760692, 11.56018628210145316, 8.715434833791933400 ) ) ;
#19561 = VECTOR ( 'NONE', #15537, 1000.000000000000000 ) ;
#19562 = EDGE_CURVE ( 'NONE', #4918, #9681, #23414, .T. ) ;
#19563 = CARTESIAN_POINT ( 'NONE',  ( 13.44051670066911086, 5.407089921784856479, -0.2156249993855441360 ) ) ;
#19564 = CARTESIAN_POINT ( 'NONE',  ( 18.00000000000000000, 5.196152422706630247, -4.518749998770942966 ) ) ;
#19565 = VERTEX_POINT ( 'NONE', #9383 ) ;
#19566 = CYLINDRICAL_SURFACE ( 'NONE', #34279, 5.999999999999999112 ) ;
#19567 = CARTESIAN_POINT ( 'NONE',  ( 5.233372021372432847, 73.94768628210142936, 8.152565276336710909 ) ) ;
#19568 = CARTESIAN_POINT ( 'NONE',  ( 27.24356964374999635, 196.9156250006145399, -15.72908226750539029 ) ) ;
#19569 = DIRECTION ( 'NONE',  ( 0.000000000000000000, -1.000000000000000000, 0.000000000000000000 ) ) ;
#19570 = CARTESIAN_POINT ( 'NONE',  ( 27.24356964375000345, 196.9343750006145228, -3.336375036156643733E-15 ) ) ;
#19571 = CARTESIAN_POINT ( 'NONE',  ( 37.11229162342512211, 7.347880794884117764E-16, 165.3220564990824073 ) ) ;
#19572 = CARTESIAN_POINT ( 'NONE',  ( 26.99999999999999645, 242.1250000000000000, -7.347880794884117764E-16 ) ) ;
#19573 = EDGE_CURVE ( 'NONE', #4926, #10170, #16145, .T. ) ;
#19574 = CARTESIAN_POINT ( 'NONE',  ( -3.796722387233185003, 54.21481371789855785, -8.710071997420207879 ) ) ;
#19575 = CARTESIAN_POINT ( 'NONE',  ( 15.00000000000000178, -3.464101615137757051, -8.962500000000012790 ) ) ;
#19576 = ORIENTED_EDGE ( 'NONE', *, *, #19844, .T. ) ;
#19577 = CARTESIAN_POINT ( 'NONE',  ( 24.00000000000000000, 242.1062500012290286, 5.196152422706629359 ) ) ;
#19578 = CARTESIAN_POINT ( 'NONE',  ( -0.1745138560722763466, 54.78981371789855359, -12.50000000000000355 ) ) ;
#19579 = CARTESIAN_POINT ( 'NONE',  ( 13.44051670066911264, -5.407089921784865361, -5.971874999385562433 ) ) ;
#19580 = CARTESIAN_POINT ( 'NONE',  ( 18.12178482187500350, -4.985214923628407568, -7.378124999385477167 ) ) ;
#19581 = CARTESIAN_POINT ( 'NONE',  ( -10.49813415416004858, 33.22731371789855359, 7.228626920338839135 ) ) ;
#19582 = AXIS2_PLACEMENT_3D ( 'NONE', #4850, #2006, #4294 ) ;
#19583 = EDGE_CURVE ( 'NONE', #32564, #15189, #26749, .T. ) ;
#19584 = ORIENTED_EDGE ( 'NONE', *, *, #12859, .F. ) ;
#19585 = CARTESIAN_POINT ( 'NONE',  ( 10.31873187879410736, -3.604726614523244610, -2.409374999385539340 ) ) ;
#19586 = EDGE_CURVE ( 'NONE', #12999, #31898, #11241, .T. ) ;
#19587 = LINE ( 'NONE', #31136, #37313 ) ;
#19588 = CARTESIAN_POINT ( 'NONE',  ( 31.33367511126808935, -7.209453229046482114, 168.1144470015464378 ) ) ;
#19589 = EDGE_CURVE ( 'NONE', #14162, #31631, #4807, .T. ) ;
#19590 = CARTESIAN_POINT ( 'NONE',  ( -40.10044563604517265, 205.1570982666397072, -4.673758765035155527 ) ) ;
#19591 = DIRECTION ( 'NONE',  ( 0.000000000000000000, 0.000000000000000000, 1.000000000000000000 ) ) ;
#19592 = CARTESIAN_POINT ( 'NONE',  ( 18.00000000000000355, -5.196152422706632912, -7.574999999999998401 ) ) ;
#19593 = CARTESIAN_POINT ( 'NONE',  ( 12.50000000000000355, 66.28981371789855359, -0.1745138560722771515 ) ) ;
#19594 = CARTESIAN_POINT ( 'NONE',  ( -31.99330436395490196, 210.1155267958017703, -4.499999999999996447 ) ) ;
#19595 = CARTESIAN_POINT ( 'NONE',  ( -49.21205436395490551, 214.6737587650352168, 4.842901733360204908 ) ) ;
#19596 = ORIENTED_EDGE ( 'NONE', *, *, #15622, .F. ) ;
#19597 = FACE_OUTER_BOUND ( 'NONE', #18927, .T. ) ;
#19598 = CARTESIAN_POINT ( 'NONE',  ( -11.08355503943118592, 44.43981371789855928, -10.83675517735179383 ) ) ;
#19599 = CARTESIAN_POINT ( 'NONE',  ( -35.94419563604516554, 201.5000000000000000, 0.1155267958018195706 ) ) ;
#19600 = MECHANICAL_DESIGN_GEOMETRIC_PRESENTATION_REPRESENTATION (  '', ( #14744 ), #7500 ) ;
#19601 = CARTESIAN_POINT ( 'NONE',  ( 10.49813415415989581, 18.17268628210144854, 7.228626920339068285 ) ) ;
#19602 = CARTESIAN_POINT ( 'NONE',  ( 12.50000000000000355, 63.31018628210144072, 0.1745138560725507937 ) ) ;
#19603 = VECTOR ( 'NONE', #15839, 1000.000000000000000 ) ;
#19604 = CARTESIAN_POINT ( 'NONE',  ( -12.50000000000000355, 141.5101862821014720, -0.1745138560725492671 ) ) ;
#19605 = CARTESIAN_POINT ( 'NONE',  ( 13.56230152254411614, -5.196152422706638241, -2.175000000000065548 ) ) ;
#19606 = CARTESIAN_POINT ( 'NONE',  ( 27.00000000000000355, 198.9875000012290229, -3.306546357697854128E-15 ) ) ;
#19607 = ORIENTED_EDGE ( 'NONE', *, *, #20933, .T. ) ;
#19608 = CARTESIAN_POINT ( 'NONE',  ( 15.53471296425195369, 35.42268628210144499, -2.908627838312120684 ) ) ;
#19609 = CARTESIAN_POINT ( 'NONE',  ( 13.62178482187499640, 195.1531250006145513, -23.59362340125807123 ) ) ;
#19610 = EDGE_CURVE ( 'NONE', #4369, #762, #31334, .T. ) ;
#19611 = CARTESIAN_POINT ( 'NONE',  ( -13.62178482187498396, 198.1343750006145399, 23.59362340125808188 ) ) ;
#19612 = CARTESIAN_POINT ( 'NONE',  ( 17.01522120763301871, 4.898587196589416773E-16, 50.34862297099062545 ) ) ;
#19613 = DIRECTION ( 'NONE',  ( 0.000000000000000000, 0.000000000000000000, 1.000000000000000000 ) ) ;
#19614 = DIRECTION ( 'NONE',  ( 0.000000000000000000, 0.000000000000000000, 1.000000000000000000 ) ) ;
#19615 = LINE ( 'NONE', #16759, #26644 ) ;
#19616 = EDGE_CURVE ( 'NONE', #29947, #16114, #2, .T. ) ;
#19617 = CARTESIAN_POINT ( 'NONE',  ( 26.75643035624999655, 247.3468750006145171, 3.323476615752267715 ) ) ;
#19618 = CARTESIAN_POINT ( 'NONE',  ( 6.594114490232462877, 120.3398137178985507, -6.840914352311949109 ) ) ;
#19619 = CARTESIAN_POINT ( 'NONE',  ( 23.87821517812500005, 241.4593750006145285, 4.985214923628404016 ) ) ;
#19620 = ORIENTED_EDGE ( 'NONE', *, *, #17390, .T. ) ;
#19621 = CARTESIAN_POINT ( 'NONE',  ( -63.85788769728821279, 216.4690446883607535, 1.857196546604031662 ) ) ;
#19622 = LINE ( 'NONE', #5191, #8709 ) ;
#19623 = CARTESIAN_POINT ( 'NONE',  ( -13.50000000000000533, 199.9250000000000114, -23.38268590217984411 ) ) ;
#19624 = CARTESIAN_POINT ( 'NONE',  ( 12.50000000000000355, 112.2898137178985678, -0.1745138560722771515 ) ) ;
#19625 = EDGE_CURVE ( 'NONE', #21259, #32891, #2072, .T. ) ;
#19626 = CARTESIAN_POINT ( 'NONE',  ( 13.44051670066911086, 5.407089921784856479, -9.665624999385530103 ) ) ;
#19627 = CARTESIAN_POINT ( 'NONE',  ( 30.88754665307854097, 7.209453229046475009, 163.0151753906892793 ) ) ;
#19628 = DIRECTION ( 'NONE',  ( 0.000000000000000000, -0.9932091452657081376, -0.1163425707149433747 ) ) ;
#19629 = CARTESIAN_POINT ( 'NONE',  ( 13.50000000000001421, 195.2000000000000171, 23.38268590217984055 ) ) ;
#19630 = ORIENTED_EDGE ( 'NONE', *, *, #534, .F. ) ;
#19631 = ORIENTED_EDGE ( 'NONE', *, *, #27204, .T. ) ;
#19632 = ORIENTED_EDGE ( 'NONE', *, *, #25391, .F. ) ;
#19633 = CARTESIAN_POINT ( 'NONE',  ( 21.00000000000000000, 6.928203230275506996, -5.006249998770934795 ) ) ;
#19635 =( GEOMETRIC_REPRESENTATION_CONTEXT ( 3 ) GLOBAL_UNCERTAINTY_ASSIGNED_CONTEXT ( ( #33763 ) ) GLOBAL_UNIT_ASSIGNED_CONTEXT ( ( #28256, #21837, #34125 ) ) REPRESENTATION_CONTEXT ( 'NONE', 'WORKASPACE' ) );
#19634 = CARTESIAN_POINT ( 'NONE',  ( 23.87821517812499650, 4.985214923628404904, -2.540624999385482141 ) ) ;
#19636 = CARTESIAN_POINT ( 'NONE',  ( 19.56230152254411792, -5.196152422706629359, -2.887499998771053455 ) ) ;
#19637 = CARTESIAN_POINT ( 'NONE',  ( 16.56230152254411436, -6.928203230275514990, -1.237499999999996270 ) ) ;
#19638 = CARTESIAN_POINT ( 'NONE',  ( 15.24356964374999990, 247.9093750006145171, -3.323476615752268604 ) ) ;
#19639 = EDGE_CURVE ( 'NONE', #19072, #15380, #34500, .T. ) ;
#19640 = CARTESIAN_POINT ( 'NONE',  ( 11.48171059495397728, 54.68518628210144783, 4.944772684328674117 ) ) ;
#19641 = VECTOR ( 'NONE', #3716, 1000.000000000000000 ) ;
#19642 = CARTESIAN_POINT ( 'NONE',  ( -59.29836230271183695, 204.3130714775002446, -3.149950860017828091 ) ) ;
#19643 = CARTESIAN_POINT ( 'NONE',  ( 5.128366027876307243, 215.9518627395465273, 0.7835069059936695668 ) ) ;
#19644 = CARTESIAN_POINT ( 'NONE',  ( -47.42336230271184405, 213.9548777149308023, 2.149950860017852960 ) ) ;
#19645 = DIRECTION ( 'NONE',  ( 1.000000000000000000, 0.000000000000000000, 0.000000000000000000 ) ) ;
#19646 = CARTESIAN_POINT ( 'NONE',  ( 28.01580572647793943, -5.196152422706632912, 164.6121661366736078 ) ) ;
#19647 = CARTESIAN_POINT ( 'NONE',  ( 12.46528703574811558, 130.4023137178985792, -2.660918448318005503 ) ) ;
#19648 = CARTESIAN_POINT ( 'NONE',  ( -39.71205436395490551, 214.6737587650352168, 4.842901733360204908 ) ) ;
#19649 = CARTESIAN_POINT ( 'NONE',  ( -42.87872103062157692, 201.4690446883607819, 2.162041339862843525 ) ) ;
#19650 = CARTESIAN_POINT ( 'NONE',  ( 15.24356964374999990, 0.000000000000000000, -2.053124999385480542 ) ) ;
#19651 = CARTESIAN_POINT ( 'NONE',  ( 5.778771075727756162E-15, 197.2156250006145513, 31.45816453501075927 ) ) ;
#19652 = CARTESIAN_POINT ( 'NONE',  ( 8.632099005475788900, 92.45231371789854791, -13.23911966647199812 ) ) ;
#19653 = CARTESIAN_POINT ( 'NONE',  ( -31.19419563604516910, 203.5000000000000000, 0.1155267958017914542 ) ) ;
#19654 = ORIENTED_EDGE ( 'NONE', *, *, #33451, .F. ) ;
#19655 = CARTESIAN_POINT ( 'NONE',  ( 26.99999999999999645, 242.2187500012290684, -3.464101615137755275 ) ) ;
#19656 = CARTESIAN_POINT ( 'NONE',  ( 8.962234695871762469, 117.3601862821014521, -8.715434833791931624 ) ) ;
#19657 = CARTESIAN_POINT ( 'NONE',  ( -2.908627838312119351, 69.92268628210143788, -15.53471296425195369 ) ) ;
#19658 = LINE ( 'NONE', #11293, #17467 ) ;
#19659 = CARTESIAN_POINT ( 'NONE',  ( 37.01420992928731835, 7.646167579472024665E-16, 161.4063293574060083 ) ) ;
#19660 = CARTESIAN_POINT ( 'NONE',  ( 15.53471296425195369, 81.42268628210145209, -2.908627838312120684 ) ) ;
#19661 = CARTESIAN_POINT ( 'NONE',  ( -40.10788769728823411, 216.4690446883607535, 1.857196546604031662 ) ) ;
#19662 = EDGE_CURVE ( 'NONE', #26963, #36019, #602, .T. ) ;
#19663 = CARTESIAN_POINT ( 'NONE',  ( 22.80587116629410716, 3.604726614523238837, -7.528124999385559235 ) ) ;
#19664 = CARTESIAN_POINT ( 'NONE',  ( -3.796722387233375073, 20.18518628210144783, 8.710071997420127943 ) ) ;
#19665 = CARTESIAN_POINT ( 'NONE',  ( 13.56230152254411614, -5.196152422706638241, -7.575000000000054357 ) ) ;
#19666 = CARTESIAN_POINT ( 'NONE',  ( -66.62872103062152007, 203.4690446883607535, 1.626142955000567936 ) ) ;
#19667 = CARTESIAN_POINT ( 'NONE',  ( 18.00000000000000355, 249.1750000000000114, 5.196152422706632912 ) ) ;
#19668 = CARTESIAN_POINT ( 'NONE',  ( 12.50000000000000355, 63.31018628210144072, 0.1745138560725507937 ) ) ;
#19669 = CARTESIAN_POINT ( 'NONE',  ( -1.909035429704832693E-15, 197.1875000000000284, -31.17691453623979214 ) ) ;
#19670 = FACE_OUTER_BOUND ( 'NONE', #10126, .T. ) ;
#19672 = CARTESIAN_POINT ( 'NONE',  ( 10.31873187879411091, 3.604726614523240613, -0.6843749993854860714 ) ) ;
#19671 = CARTESIAN_POINT ( 'NONE',  ( -9.500000000000005329, 21.91018628210143859, -0.1745138560725176813 ) ) ;
#19673 = CARTESIAN_POINT ( 'NONE',  ( 26.75643035624999655, 249.5968750006145171, 3.323476615752267271 ) ) ;
#19674 = VERTEX_POINT ( 'NONE', #11797 ) ;
#19675 = CARTESIAN_POINT ( 'NONE',  ( 23.99999999999999645, 5.196152422706631135, -4.649999999999987921 ) ) ;
#19676 = CARTESIAN_POINT ( 'NONE',  ( 25.40019891165470511, -3.899351167896716319, -7.999999999999994671 ) ) ;
#19677 = CARTESIAN_POINT ( 'NONE',  ( 36.86059793269458140, 3.604726614523243278, 159.6505362020193104 ) ) ;
#19678 = CARTESIAN_POINT ( 'NONE',  ( 10.31873187879410914, 0.000000000000000000, -1.040624999385536542 ) ) ;
#19679 = CARTESIAN_POINT ( 'NONE',  ( 36.58935716683210870, -3.464101615137755275, 159.3448883093075779 ) ) ;
#19680 = CARTESIAN_POINT ( 'NONE',  ( 15.00000000000000000, 244.1500000000000057, 0.000000000000000000 ) ) ;
#19681 = CARTESIAN_POINT ( 'NONE',  ( -14.50000000000000000, 215.7563705986615901, 5.555555555555558023 ) ) ;
#19682 = CARTESIAN_POINT ( 'NONE',  ( -12.53471296425194659, 95.22268628210144925, 2.311890736173176641 ) ) ;
#19683 = EDGE_LOOP ( 'NONE', ( #18649, #26215, #7495, #9907, #21164, #31659, #3850, #32620 ) ) ;
#19684 = ORIENTED_EDGE ( 'NONE', *, *, #34158, .T. ) ;
#19686 = CARTESIAN_POINT ( 'NONE',  ( -13.49999999999998401, 194.7875000012290343, 23.38268590217985476 ) ) ;
#19685 = B_SPLINE_CURVE_WITH_KNOTS ( 'NONE', 3,
 ( #21551, #17953, #29684, #35178, #15100, #9414, #6378, #27403 ),
 .UNSPECIFIED., .F., .F.,
 ( 4, 2, 2, 4 ),
 ( 0.000000000000000000, 0.002521202642312846305, 0.003781803963469229125, 0.005042405284625611946 ),
 .UNSPECIFIED. ) ;
#19687 = DIRECTION ( 'NONE',  ( 0.9961946980917462113, 0.000000000000000000, -0.08715574274765118534 ) ) ;
#19688 = CARTESIAN_POINT ( 'NONE',  ( 6.092822981423662299, 40.41481371789855359, 14.25334919248795096 ) ) ;
#19689 = CARTESIAN_POINT ( 'NONE',  ( 18.12178482187500350, -4.985214923628407568, -8.278124999385488181 ) ) ;
#19690 = CARTESIAN_POINT ( 'NONE',  ( 23.87821517812500005, 242.3593750006145342, 4.985214923628404016 ) ) ;
#19691 = CARTESIAN_POINT ( 'NONE',  ( -46.24330436395489841, 210.1155267958017703, -4.499999999999996447 ) ) ;
#19692 = CARTESIAN_POINT ( 'NONE',  ( 28.36878648460592700, -5.196152422706632912, 168.6467546639452166 ) ) ;
#19693 = CARTESIAN_POINT ( 'NONE',  ( 37.05669835387680422, 3.604726614523243278, 161.8919742727257187 ) ) ;
#19694 = CARTESIAN_POINT ( 'NONE',  ( -6.594114490232462877, 42.13981371789854791, 6.840914352311949109 ) ) ;
#19695 = CARTESIAN_POINT ( 'NONE',  ( 22.80587116629411071, -3.604726614523235284, -9.403124999385534366 ) ) ;
#19696 = CARTESIAN_POINT ( 'NONE',  ( -9.500000000000005329, 98.48981371789855643, 0.1745138560723101806 ) ) ;
#19697 = CARTESIAN_POINT ( 'NONE',  ( 27.24356964375000700, 197.7968750006145342, 15.72908226750537075 ) ) ;
#19698 = CARTESIAN_POINT ( 'NONE',  ( -10.83675517735179028, 143.3398137178985507, 11.08355503943118947 ) ) ;
#19699 =( BOUNDED_CURVE ( )  B_SPLINE_CURVE ( 3, ( #23255, #17385, #25902, #35168 ),
 .UNSPECIFIED., .F., .F. ) 
 B_SPLINE_CURVE_WITH_KNOTS ( ( 4, 4 ),
 ( 3.141592653589793116, 4.712388980384647930 ),
 .UNSPECIFIED. ) 
 CURVE ( )  GEOMETRIC_REPRESENTATION_ITEM ( )  RATIONAL_B_SPLINE_CURVE ( ( 1.000000000000000000, 0.8047378541243747074, 0.8047378541243747074, 1.000000000000000000 ) ) 
 REPRESENTATION_ITEM ( '' )  );
#19700 = EDGE_CURVE ( 'NONE', #28686, #11014, #17558, .T. ) ;
#19701 = CARTESIAN_POINT ( 'NONE',  ( 4.622313124798573369, 65.03518628210144925, 11.61527771782819940 ) ) ;
#19702 = DIRECTION ( 'NONE',  ( -1.000000000000000000, -0.000000000000000000, -0.000000000000000000 ) ) ;
#19703 = CARTESIAN_POINT ( 'NONE',  ( 33.91574363238778034, 5.407089921784857367, 161.8091613863793725 ) ) ;
#19704 = EDGE_CURVE ( 'NONE', #32439, #2357, #11984, .T. ) ;
#19705 = CARTESIAN_POINT ( 'NONE',  ( 18.00000000000000000, 5.196152422706630247, -0.4687499987709453642 ) ) ;
#19706 = CARTESIAN_POINT ( 'NONE',  ( 19.68408634441911431, 5.407089921784862696, -5.746874999385531702 ) ) ;
#19707 = FACE_OUTER_BOUND ( 'NONE', #3995, .T. ) ;
#19708 = CARTESIAN_POINT ( 'NONE',  ( -27.00000000000000355, 194.7125000012290172, 0.000000000000000000 ) ) ;
#19709 = CARTESIAN_POINT ( 'NONE',  ( -2.064181346179269738, 84.29768628210146630, 9.465287035748067623 ) ) ;
#19710 = DIRECTION ( 'NONE',  ( 1.000000000000000000, 0.000000000000000000, 0.000000000000000000 ) ) ;
#19711 = EDGE_CURVE ( 'NONE', #36421, #8730, #11262, .T. ) ;
#19712 = CARTESIAN_POINT ( 'NONE',  ( 10.69584247140445221, 108.4476862821014578, -6.932735513423970097 ) ) ;
#19713 = CARTESIAN_POINT ( 'NONE',  ( 24.74614436184151955, 0.000000000000000000, 161.6609054635707423 ) ) ;
#19714 = CARTESIAN_POINT ( 'NONE',  ( 23.99999999999999645, 240.4562500012290513, -5.196152422706631135 ) ) ;
#19715 = ORIENTED_EDGE ( 'NONE', *, *, #23847, .T. ) ;
#19716 = CARTESIAN_POINT ( 'NONE',  ( 33.99418380086066804, 5.407089921784857367, 162.7057366146619586 ) ) ;
#19717 = CARTESIAN_POINT ( 'NONE',  ( 15.24356964374999990, 3.323476615752268604, -6.478124999385451055 ) ) ;
#19718 = CARTESIAN_POINT ( 'NONE',  ( 13.62178482187501416, 195.9593750006145569, 23.59362340125806767 ) ) ;
#19719 = CARTESIAN_POINT ( 'NONE',  ( 31.19640481644053764, 7.209453229046482114, 166.5454403520519122 ) ) ;
#19720 = CARTESIAN_POINT ( 'NONE',  ( 37.13843834614232264, -3.464101615137755275, 165.6209149072855666 ) ) ;
#19721 = CARTESIAN_POINT ( 'NONE',  ( 22.56230152254412147, 7.347880794884125653E-16, -4.275000000000028777 ) ) ;
#19722 = CARTESIAN_POINT ( 'NONE',  ( 23.87821517812499650, 241.6093750006145342, -4.985214923628404904 ) ) ;
#19723 = DIRECTION ( 'NONE',  ( -0.000000000000000000, -1.000000000000000000, -0.000000000000000000 ) ) ;
#19724 = VECTOR ( 'NONE', #10226, 1000.000000000000114 ) ;
#19725 =( BOUNDED_CURVE ( )  B_SPLINE_CURVE ( 2, ( #18148, #18334, #15486, #17960, #27040, #1066, #12637, #27227, #20805 ),
 .UNSPECIFIED., .F., .F. ) 
 B_SPLINE_CURVE_WITH_KNOTS ( ( 3, 2, 2, 2, 3 ),
 ( 0.2717391304347825942, 0.2753623188405797118, 0.2826086956521738913, 0.2898550724637681264, 0.2934782608695652439 ),
 .UNSPECIFIED. ) 
 CURVE ( )  GEOMETRIC_REPRESENTATION_ITEM ( )  RATIONAL_B_SPLINE_CURVE ( ( 0.9330127018922191873, 0.9330127018922187432, 1.000000000000000000, 0.8660254037844387076, 1.000000000000000000, 0.8660254037844387076, 1.000000000000000000, 0.9330127018922188542, 0.9330127018922194093 ) ) 
 REPRESENTATION_ITEM ( '' )  );
#19726 = CARTESIAN_POINT ( 'NONE',  ( -2.660918448318004614, 118.9023137178985507, -12.46528703574811558 ) ) ;
#19727 = CARTESIAN_POINT ( 'NONE',  ( -11.61527771782819940, 140.9351862821014834, 4.622313124798574258 ) ) ;
#19728 = B_SPLINE_CURVE_WITH_KNOTS ( 'NONE', 3,
 ( #13988, #25357, #4887, #2229 ),
 .UNSPECIFIED., .F., .F.,
 ( 4, 4 ),
 ( 0.000000000000000000, 1.000000000000000000 ),
 .UNSPECIFIED. ) ;
#19730 = ORIENTED_EDGE ( 'NONE', *, *, #18990, .T. ) ;
#19729 = ORIENTED_EDGE ( 'NONE', *, *, #29819, .F. ) ;
#19731 = CARTESIAN_POINT ( 'NONE',  ( 26.75643035624999655, 243.7093750006145285, -3.323476615752271712 ) ) ;
#19732 = CARTESIAN_POINT ( 'NONE',  ( -12.53471296425189152, 6.777313717898553413, -2.311890736173453309 ) ) ;
#19733 = CARTESIAN_POINT ( 'NONE',  ( 21.00000000000000000, -6.646953231504538984, -6.778124999385457983 ) ) ;
#19734 = CARTESIAN_POINT ( 'NONE',  ( -8.927990412390371944, 109.1273137178985451, -13.04141134922778988 ) ) ;
#19735 = CARTESIAN_POINT ( 'NONE',  ( -72.05441616160760532, 219.4495263357960368, -2.499999999999991118 ) ) ;
#19736 = CARTESIAN_POINT ( 'NONE',  ( 21.00000000000000000, 6.646953231504538984, -1.265624999385487115 ) ) ;
#19737 = CARTESIAN_POINT ( 'NONE',  ( 22.80587116629412492, 3.604726614523243278, -8.484374999385497773 ) ) ;
#19738 = CARTESIAN_POINT ( 'NONE',  ( -27.00000000000000355, 199.6250000012290684, -15.58845726811989429 ) ) ;
#19739 = CARTESIAN_POINT ( 'NONE',  ( 2.660918448318279950, 116.4976862821014549, -12.46528703574805697 ) ) ;
#19740 = CARTESIAN_POINT ( 'NONE',  ( 10.31873187879410914, 0.000000000000000000, -3.290624999385538541 ) ) ;
#19741 = CARTESIAN_POINT ( 'NONE',  ( -46.63169563604517265, 210.1155267958018271, 8.500000000000003553 ) ) ;
#19742 = CARTESIAN_POINT ( 'NONE',  ( 15.24356964374999990, 243.8593750006145342, -3.323476615752268604 ) ) ;
#19743 = VECTOR ( 'NONE', #23898, 1000.000000000000000 ) ;
#19744 = CARTESIAN_POINT ( 'NONE',  ( 16.56230152254411081, -6.928203230275506996, -2.924999998770990928 ) ) ;
#19745 = CARTESIAN_POINT ( 'NONE',  ( -68.00669563604516554, 209.8844732041982013, -6.500000000000000888 ) ) ;
#19746 = CARTESIAN_POINT ( 'NONE',  ( 11.48171059495397728, 119.0851862821014606, 4.944772684328674117 ) ) ;
#19747 = CARTESIAN_POINT ( 'NONE',  ( 22.56230152254412147, -3.464101615137751278, -3.749999998771020415 ) ) ;
#19748 = CARTESIAN_POINT ( 'NONE',  ( -45.05580436395489841, 216.5000000000000000, 0.1155267958017343610 ) ) ;
#19749 = CARTESIAN_POINT ( 'NONE',  ( 26.99999999999999289, 0.000000000000000000, -8.000000000000000000 ) ) ;
#19750 = CARTESIAN_POINT ( 'NONE',  ( -26.99999999999999645, 199.5875000000000341, 15.58845726811991561 ) ) ;
#19751 = CARTESIAN_POINT ( 'NONE',  ( -10.83675517735155047, 96.66018628210144925, -11.08355503943142750 ) ) ;
#19752 = CARTESIAN_POINT ( 'NONE',  ( -12.46528703574805874, 22.19768628210144712, -2.660918448318280838 ) ) ;
#19753 = CARTESIAN_POINT ( 'NONE',  ( 2.064181346179272847, 134.8976862821014606, -9.465287035748065847 ) ) ;
#19754 = CARTESIAN_POINT ( 'NONE',  ( 19.68408634441910365, -5.407089921784855591, -0.8906249993855530622 ) ) ;
#19755 = CARTESIAN_POINT ( 'NONE',  ( 10.49999999999999822, 252.0000000000000000, -2.499999999999986677 ) ) ;
#19756 = ORIENTED_EDGE ( 'NONE', *, *, #32646, .T. ) ;
#19757 = CARTESIAN_POINT ( 'NONE',  ( 10.56230152254411081, 0.000000000000000000, -4.837499998771033205 ) ) ;
#19758 = CARTESIAN_POINT ( 'NONE',  ( -8.843639120294326972, 58.13518628210145067, 3.474262827703335166 ) ) ;
#19759 =( BOUNDED_CURVE ( )  B_SPLINE_CURVE ( 2, ( #23149, #13875, #34691, #36789, #2299, #13690, #25238 ),
 .UNSPECIFIED., .F., .F. ) 
 B_SPLINE_CURVE_WITH_KNOTS ( ( 3, 2, 2, 3 ),
 ( 0.2608695652173921298, 0.2681159420289864759, 0.2753623188405807110, 0.2826086956521750015 ),
 .UNSPECIFIED. ) 
 CURVE ( )  GEOMETRIC_REPRESENTATION_ITEM ( )  RATIONAL_B_SPLINE_CURVE ( ( 0.9999999999999845679, 0.8660254037844541397, 1.000000000000000000, 0.8660254037844387076, 1.000000000000000000, 0.8660254037844181685, 1.000000000000020428 ) ) 
 REPRESENTATION_ITEM ( '' )  );
#19760 =( LENGTH_UNIT ( ) NAMED_UNIT ( * ) SI_UNIT ( .MILLI., .METRE. ) );
#19761 = CARTESIAN_POINT ( 'NONE',  ( 13.62178482187501416, 195.4531250006145342, 23.59362340125806767 ) ) ;
#19762 = FACE_OUTER_BOUND ( 'NONE', #11863, .T. ) ;
#19763 = CARTESIAN_POINT ( 'NONE',  ( -13.62178482187500528, 196.1843750006145228, -23.59362340125807123 ) ) ;
#19764 = CARTESIAN_POINT ( 'NONE',  ( -38.47274018782781013, 246.3803829651731121, -0.4999999999999995559 ) ) ;
#19765 = EDGE_CURVE ( 'NONE', #25296, #19526, #31475, .T. ) ;
#19766 = CARTESIAN_POINT ( 'NONE',  ( 8.152565276336593669, 48.75231371789854506, 5.233372021372610483 ) ) ;
#19767 = CARTESIAN_POINT ( 'NONE',  ( 21.00000000000000000, 6.928203230275506996, -9.112500000000002487 ) ) ;
#19768 = ORIENTED_EDGE ( 'NONE', *, *, #28427, .F. ) ;
#19769 = B_SPLINE_CURVE_WITH_KNOTS ( 'NONE', 3,
 ( #36049, #15413, #7257, #606, #12175, #9345, #988, #23749, #18645, #9902, #10094, #12564, #35287, #21486, #26768, #9724, #33217, #9532, #20915, #32454, #6498, #18071, #21297, #32833 ),
 .UNSPECIFIED., .F., .F.,
 ( 4, 2, 2, 2, 2, 2, 2, 2, 2, 2, 2, 4 ),
 ( 0.000000000000000000, 0.001514496631480036389, 0.002271744947220054583, 0.003028993262960072777, 0.004543489894440108298, 0.005300738210180123457, 0.006057986525920138615, 0.007572483157400161126, 0.008329731473140176284, 0.009086979788880192310, 0.01060147642036021222, 0.01211597305184023213 ),
 .UNSPECIFIED. ) ;
#19770 = CARTESIAN_POINT ( 'NONE',  ( 26.99999999999999645, 241.7312500012290570, -7.347880794884117764E-16 ) ) ;
#19771 = CARTESIAN_POINT ( 'NONE',  ( -0.1745138560722763466, 63.98981371789854933, -12.50000000000000355 ) ) ;
#19772 = CARTESIAN_POINT ( 'NONE',  ( 22.80587116629411426, 7.646167579472024665E-16, -7.171874999385541294 ) ) ;
#19773 = CARTESIAN_POINT ( 'NONE',  ( 26.75643035624999655, 7.049594010296217766E-16, -7.228124999385493687 ) ) ;
#19774 = CARTESIAN_POINT ( 'NONE',  ( 6.932735513424201024, 28.05231371789855643, -10.69584247140429412 ) ) ;
#19775 = AXIS2_PLACEMENT_3D ( 'NONE', #4945, #16158, #27707 ) ;
#19776 = VERTEX_POINT ( 'NONE', #26384 ) ;
#19777 = CARTESIAN_POINT ( 'NONE',  ( 10.31873187879410203, 3.604726614523240613, -0.2343749993854903624 ) ) ;
#19778 = CARTESIAN_POINT ( 'NONE',  ( 18.00000000000000355, 246.0812500012290513, 5.196152422706632912 ) ) ;
#19779 = EDGE_CURVE ( 'NONE', #2436, #15581, #20014, .T. ) ;
#19780 = CARTESIAN_POINT ( 'NONE',  ( 34.53836246964132073, 5.407089921784862696, 168.9257272608723213 ) ) ;
#19781 = CARTESIAN_POINT ( 'NONE',  ( -44.85044563604515133, 205.1570982666397072, -4.673758765035155527 ) ) ;
#19782 = CARTESIAN_POINT ( 'NONE',  ( 36.64491895294136015, 3.464101615137448409, 159.9799624305653936 ) ) ;
#19783 = CARTESIAN_POINT ( 'NONE',  ( 10.31873187879411091, 0.000000000000000000, -0.1687499993855423597 ) ) ;
#19784 = CARTESIAN_POINT ( 'NONE',  ( -38.92038769728823411, 208.6787018382581778, 4.469044688360752637 ) ) ;
#19785 = CARTESIAN_POINT ( 'NONE',  ( -49.60788769728823411, 216.4690446883607535, 1.857196546604031662 ) ) ;
#19786 = ORIENTED_EDGE ( 'NONE', *, *, #37261, .T. ) ;
#19787 = DIRECTION ( 'NONE',  ( -0.000000000000000000, 0.000000000000000000, 1.000000000000000000 ) ) ;
#19788 = CARTESIAN_POINT ( 'NONE',  ( 22.56230152254411792, 7.347880794884125653E-16, -1.575000000000048583 ) ) ;
#19789 = CARTESIAN_POINT ( 'NONE',  ( -13.04141134922778456, 33.22731371789855359, 8.927990412390377273 ) ) ;
#19790 = CARTESIAN_POINT ( 'NONE',  ( -69.79538769728823411, 212.3930949314662371, -8.469044688360781947 ) ) ;
#19791 = CARTESIAN_POINT ( 'NONE',  ( -6.840914352312096547, 140.3601862821014663, 6.594114490232313663 ) ) ;
#19792 = CARTESIAN_POINT ( 'NONE',  ( -4.944772684328673229, 47.78518628210144925, 11.48171059495397728 ) ) ;
#19793 = ADVANCED_FACE ( 'NONE', ( #20716 ), #35283, .F. ) ;
#19794 = CARTESIAN_POINT ( 'NONE',  ( 10.56230152254411436, -3.464101615137761048, -3.112500000000005596 ) ) ;
#19795 = FACE_OUTER_BOUND ( 'NONE', #37196, .T. ) ;
#19796 = ORIENTED_EDGE ( 'NONE', *, *, #352, .T. ) ;
#19797 = CARTESIAN_POINT ( 'NONE',  ( -8.632099005475501130, 14.14768628210144286, -13.23911966647218996 ) ) ;
#19798 = DIRECTION ( 'NONE',  ( 0.000000000000000000, 0.000000000000000000, 1.000000000000000000 ) ) ;
#19799 = CARTESIAN_POINT ( 'NONE',  ( 27.24356964374999635, 198.7718750006145569, -15.72908226750539029 ) ) ;
#19800 = FACE_OUTER_BOUND ( 'NONE', #26486, .T. ) ;
#19801 = CARTESIAN_POINT ( 'NONE',  ( 0.000000000000000000, 210.0000000000000284, 0.000000000000000000 ) ) ;
#19802 = CARTESIAN_POINT ( 'NONE',  ( 18.00000000000000000, 5.196152422706630247, -5.418749998770955756 ) ) ;
#19803 = EDGE_CURVE ( 'NONE', #4030, #20323, #30645, .T. ) ;
#19804 = CARTESIAN_POINT ( 'NONE',  ( 28.09424589495082714, -5.196152422706632912, 165.5087413649561938 ) ) ;
#19805 = CARTESIAN_POINT ( 'NONE',  ( 15.24356964374999990, 247.5718750006145399, -3.323476615752268604 ) ) ;
#19806 = CARTESIAN_POINT ( 'NONE',  ( 6.840914352311949109, 104.2398137178985706, 6.594114490232462877 ) ) ;
#19807 = CARTESIAN_POINT ( 'NONE',  ( 18.12178482187500350, 242.7343750006145342, 4.985214923628407568 ) ) ;
#19808 = VERTEX_POINT ( 'NONE', #15023 ) ;
#19809 = DIRECTION ( 'NONE',  ( -0.000000000000000000, 1.000000000000000000, -0.000000000000000000 ) ) ;
#19810 = CARTESIAN_POINT ( 'NONE',  ( -1.045839947578415010E-13, 196.0625000000000284, 27.00000000000000355 ) ) ;
#19811 = CIRCLE ( 'NONE', #30681, 4.000000000000001776 ) ;
#19812 = CARTESIAN_POINT ( 'NONE',  ( 23.99999999999999645, 249.4562500012290229, -5.196152422706631135 ) ) ;
#19813 = CARTESIAN_POINT ( 'NONE',  ( 7.228626920338837358, 122.9273137178985564, 10.49813415416005036 ) ) ;
#19814 = CARTESIAN_POINT ( 'NONE',  ( 24.19849202207518246, 7.686353184319896670, -10.24485366105522743 ) ) ;
#19815 = CARTESIAN_POINT ( 'NONE',  ( 30.82871652672388052, -7.209453229046475009, 162.3427439694773398 ) ) ;
#19816 = CARTESIAN_POINT ( 'NONE',  ( 27.24356964375000345, 199.6343750006145399, -3.336375036156643733E-15 ) ) ;
#19817 = ORIENTED_EDGE ( 'NONE', *, *, #29984, .T. ) ;
#19818 = ORIENTED_EDGE ( 'NONE', *, *, #6200, .F. ) ;
#19819 = EDGE_LOOP ( 'NONE', ( #1514, #19630, #7108, #3087 ) ) ;
#19820 = CARTESIAN_POINT ( 'NONE',  ( 24.00000000000000000, -5.196152422706629359, -5.643749998770958065 ) ) ;
#19821 = CARTESIAN_POINT ( 'NONE',  ( 18.12178482187500350, -4.985214923628407568, -3.215624999385463312 ) ) ;
#19822 = CARTESIAN_POINT ( 'NONE',  ( 0.000000000000000000, 143.0000000000000000, 0.000000000000000000 ) ) ;
#19823 = LINE ( 'NONE', #25300, #5615 ) ;
#19824 = CARTESIAN_POINT ( 'NONE',  ( 23.87821517812500005, 248.5468750006145058, 4.985214923628404016 ) ) ;
#19825 = CARTESIAN_POINT ( 'NONE',  ( 12.46528703574805874, 54.39768628210146062, 2.660918448318279950 ) ) ;
#19826 = CARTESIAN_POINT ( 'NONE',  ( -56.92336230271182984, 215.6869285224997270, 3.149950860017831200 ) ) ;
#19827 = CARTESIAN_POINT ( 'NONE',  ( 15.53186252112510779, 224.5816999436668766, -2.477503916096131409 ) ) ;
#19828 = CARTESIAN_POINT ( 'NONE',  ( -42.07961230271182984, 211.3212981617417938, 4.469044688360757966 ) ) ;
#19829 = CARTESIAN_POINT ( 'NONE',  ( 34.09102412561951212, 5.196152422706631135, 165.2099507155409412 ) ) ;
#19830 = CARTESIAN_POINT ( 'NONE',  ( 11.48171059495408208, 102.5148137178985621, -4.944772684328420986 ) ) ;
#19831 = CARTESIAN_POINT ( 'NONE',  ( -68.60788769728823411, 214.4690446883608104, 1.321298161741840893 ) ) ;
#19832 = CARTESIAN_POINT ( 'NONE',  ( -45.84747103062156981, 214.3500491399821044, -7.303452534266878793 ) ) ;
#19833 = ITEM_DEFINED_TRANSFORMATION ( 'NONE', 'NONE', #15399,  #17215 ) ;
#19834 = CARTESIAN_POINT ( 'NONE',  ( 20.99999999999999645, -6.646953231504538984, -3.290624999385483918 ) ) ;
#19835 = CARTESIAN_POINT ( 'NONE',  ( 20.99999999999999645, 243.3624999999999829, 5.999999999999998224 ) ) ;
#19836 = CARTESIAN_POINT ( 'NONE',  ( 15.50000000000000533, 103.0898137178985792, -0.1745138560722452326 ) ) ;
#19837 = CARTESIAN_POINT ( 'NONE',  ( -35.15252896937850124, 206.6499508600178387, -5.571401726697954970 ) ) ;
#19838 = ORIENTED_EDGE ( 'NONE', *, *, #18725, .T. ) ;
#19839 = CARTESIAN_POINT ( 'NONE',  ( -11.61527771782819940, 113.3351862821014606, 4.622313124798574258 ) ) ;
#19840 = CARTESIAN_POINT ( 'NONE',  ( 8.632099005475504683, 55.54768628210144499, 13.23911966647218996 ) ) ;
#19841 = CARTESIAN_POINT ( 'NONE',  ( 10.56230152254410726, 0.000000000000000000, -0.9000000000000396572 ) ) ;
#19842 = CARTESIAN_POINT ( 'NONE',  ( 30.86303410043077022, -7.209453229046482114, 162.7349956318509783 ) ) ;
#19843 = CARTESIAN_POINT ( 'NONE',  ( 8.927990412390657937, 61.87268628210144783, -13.04141134922759804 ) ) ;
#19844 = EDGE_CURVE ( 'NONE', #19526, #7363, #26036, .T. ) ;
#19845 = CARTESIAN_POINT ( 'NONE',  ( 10.31873187879411091, -3.604726614523240613, -7.303124999385512517 ) ) ;
#19846 = CARTESIAN_POINT ( 'NONE',  ( -7.954856959092191815, 22.77268628210143220, -5.529263428287477744 ) ) ;
#19847 = CARTESIAN_POINT ( 'NONE',  ( 20.99999999999999645, 0.000000000000000000, -8.000000000000000000 ) ) ;
#19848 = CARTESIAN_POINT ( 'NONE',  ( -64.84747103062156270, 213.3500491399821328, -5.571401726697985168 ) ) ;
#19849 = CARTESIAN_POINT ( 'NONE',  ( -69.83334449017395684, 223.2245623293732706, -7.500000000000000000 ) ) ;
#19850 = CARTESIAN_POINT ( 'NONE',  ( 8.715434833791931624, 55.26018628210144357, 8.962234695871760692 ) ) ;
#19851 = CARTESIAN_POINT ( 'NONE',  ( -13.50000000000000533, 198.1250000000000284, -23.38268590217984411 ) ) ;
#19852 = DIRECTION ( 'NONE',  ( 0.000000000000000000, 0.000000000000000000, 1.000000000000000000 ) ) ;
#19854 = CARTESIAN_POINT ( 'NONE',  ( 16.56230152254411436, -7.209453229046482114, -2.784374999385508698 ) ) ;
#19853 = CARTESIAN_POINT ( 'NONE',  ( -3.796722387233375073, 20.18518628210144783, 8.710071997420127943 ) ) ;
#19855 = CARTESIAN_POINT ( 'NONE',  ( 20.99999999999999645, 248.6218750006145228, 6.646953231504538984 ) ) ;
#19856 = ORIENTED_EDGE ( 'NONE', *, *, #23504, .T. ) ;
#19857 = CARTESIAN_POINT ( 'NONE',  ( 15.00000000000000178, -3.464101615137757051, -3.562500000000000888 ) ) ;
#19858 = DIRECTION ( 'NONE',  ( -0.000000000000000000, -1.000000000000000000, -0.000000000000000000 ) ) ;
#19859 = CARTESIAN_POINT ( 'NONE',  ( 24.47980610650860100, -3.604726614523244610, 161.4112935226266359 ) ) ;
#19860 = CARTESIAN_POINT ( 'NONE',  ( 22.80587116629410716, -3.604726614523235284, -0.8531249993855525293 ) ) ;
#19861 = CARTESIAN_POINT ( 'NONE',  ( 37.57146195948011069, 3.604726614523238837, 167.7757492083300690 ) ) ;
#19862 = CARTESIAN_POINT ( 'NONE',  ( 18.00000000000000000, 243.6250000000000000, -5.196152422706630247 ) ) ;
#19863 = DIRECTION ( 'NONE',  ( 0.000000000000000000, 0.000000000000000000, 1.000000000000000000 ) ) ;
#19864 = CARTESIAN_POINT ( 'NONE',  ( -12.46528703574805874, 68.19768628210144357, -2.660918448318280838 ) ) ;
#19865 = VERTEX_POINT ( 'NONE', #31888 ) ;
#19866 = ORIENTED_EDGE ( 'NONE', *, *, #25829, .T. ) ;
#19867 = CARTESIAN_POINT ( 'NONE',  ( 13.50000000000001421, 196.6625000012290343, 23.38268590217984055 ) ) ;
#19868 = CARTESIAN_POINT ( 'NONE',  ( -7.234628195640302017, 196.6049038117967029, 27.00000000000000711 ) ) ;
#19869 = CARTESIAN_POINT ( 'NONE',  ( 13.23911966647199812, 39.55231371789854933, 8.632099005475788900 ) ) ;
#19870 = CARTESIAN_POINT ( 'NONE',  ( 15.24356964375000167, -3.323476615752272600, -8.765624999385490668 ) ) ;
#19871 = CARTESIAN_POINT ( 'NONE',  ( 15.24356964374999990, 243.0718750006145115, -3.323476615752268604 ) ) ;
#19872 = AXIS2_PLACEMENT_3D ( 'NONE', #15980, #12941, #1370 ) ;
#19873 = CARTESIAN_POINT ( 'NONE',  ( -49.60788769728823411, 214.4690446883608104, 1.321298161741840893 ) ) ;
#19874 = DIRECTION ( 'NONE',  ( 0.08715574274765150453, 0.000000000000000000, 0.9961946980917461003 ) ) ;
#19875 = EDGE_CURVE ( 'NONE', #25619, #29586, #43, .T. ) ;
#19876 = CARTESIAN_POINT ( 'NONE',  ( 37.09265009776020605, 7.646167579472024665E-16, 162.3029045856885659 ) ) ;
#19877 = CARTESIAN_POINT ( 'NONE',  ( 5.529263428287300108, 30.92731371789853867, 7.954856959092309943 ) ) ;
#19878 = CARTESIAN_POINT ( 'NONE',  ( -69.79538769728823411, 211.8571965466039444, -6.469044688360768625 ) ) ;
#19879 = FILL_AREA_STYLE_COLOUR ( '', #37161 ) ;
#19880 = CARTESIAN_POINT ( 'NONE',  ( 25.01286569224582834, 195.0000000000000000, -10.34054035972909169 ) ) ;
#19881 = CARTESIAN_POINT ( 'NONE',  ( 27.24356964375000345, 197.3843750006145399, -3.336375036156643733E-15 ) ) ;
#19882 = CARTESIAN_POINT ( 'NONE',  ( -7.228626920338836470, 17.12731371789854862, -10.49813415416005213 ) ) ;
#19883 = CARTESIAN_POINT ( 'NONE',  ( 6.932735513423970097, 64.74768628210145494, 10.69584247140445044 ) ) ;
#19884 = CARTESIAN_POINT ( 'NONE',  ( -0.5000000000000047740, 244.5000000000000000, 1.000000000000000000 ) ) ;
#19885 = DIRECTION ( 'NONE',  ( 0.000000000000000000, 1.000000000000000000, 0.000000000000000000 ) ) ;
#19886 = VECTOR ( 'NONE', #4059, 1000.000000000000000 ) ;
#19887 = CARTESIAN_POINT ( 'NONE',  ( 36.81974367828161121, -3.604726614523235284, 159.1835699372887802 ) ) ;
#19888 = CARTESIAN_POINT ( 'NONE',  ( 26.99999999999999645, -3.464101615137751278, -0.6562499987709655702 ) ) ;
#19889 = CARTESIAN_POINT ( 'NONE',  ( 16.56230152254411081, -7.209453229046482114, -9.084374999385513405 ) ) ;
#19890 = CARTESIAN_POINT ( 'NONE',  ( -4.694659320240884604E-14, 197.0750000012290570, 27.00000000000000000 ) ) ;
#19891 = CARTESIAN_POINT ( 'NONE',  ( -5.233372021372430183, 78.54768628210145209, -8.152565276336710909 ) ) ;
#19892 = DIRECTION ( 'NONE',  ( -0.000000000000000000, 1.000000000000000000, -0.000000000000000000 ) ) ;
#19893 = CARTESIAN_POINT ( 'NONE',  ( -10.49813415415989581, 114.7726862821014606, -7.228626920339068285 ) ) ;
#19894 = DIRECTION ( 'NONE',  ( 4.130293990420971239E-17, -1.000000000000000000, 0.000000000000000000 ) ) ;
#19895 = CARTESIAN_POINT ( 'NONE',  ( 10.56230152254410903, 0.000000000000000000, -3.487499998771015353 ) ) ;
#19896 = ORIENTED_EDGE ( 'NONE', *, *, #12423, .F. ) ;
#19897 = CARTESIAN_POINT ( 'NONE',  ( 33.95496371662422064, 5.407089921784857367, 162.2574490005206655 ) ) ;
#19898 = VECTOR ( 'NONE', #5845, 1000.000000000000000 ) ;
#19899 = CARTESIAN_POINT ( 'NONE',  ( 15.24356964374999990, 0.000000000000000000, -8.690624999385471838 ) ) ;
#19900 = CARTESIAN_POINT ( 'NONE',  ( -1.926257025242585782E-15, 195.6968750006145683, -31.45816453501076637 ) ) ;
#19901 = CARTESIAN_POINT ( 'NONE',  ( 28.10284103007056089, -5.407089921784865361, 167.0043083327929878 ) ) ;
#19902 = CARTESIAN_POINT ( 'NONE',  ( 25.21024869186565098, -3.464101615137761048, 166.9656422296849314 ) ) ;
#19903 = PLANE ( 'NONE',  #8384 ) ;
#19904 = CARTESIAN_POINT ( 'NONE',  ( 26.75643035624999655, 241.1218750006145228, -3.323476615752271712 ) ) ;
#19905 = CARTESIAN_POINT ( 'NONE',  ( 5.778771075727756162E-15, 198.1156250006145285, 31.45816453501076637 ) ) ;
#19906 = CARTESIAN_POINT ( 'NONE',  ( 11.48171059495408208, 120.9148137178985536, -4.944772684328420986 ) ) ;
#19907 = CARTESIAN_POINT ( 'NONE',  ( -7.228626920339070061, 130.8726862821014834, 10.49813415415989404 ) ) ;
#19909 = VERTEX_POINT ( 'NONE', #24125 ) ;
#19908 = VERTEX_POINT ( 'NONE', #21292 ) ;
#19910 = CARTESIAN_POINT ( 'NONE',  ( 26.75643035624999655, 241.9093750006145171, -3.323476615752271712 ) ) ;
#19911 = EDGE_CURVE ( 'NONE', #4550, #13097, #3645, .T. ) ;
#19912 = CARTESIAN_POINT ( 'NONE',  ( -3.257655550456946880, 100.5023137178985451, -15.46528703574811736 ) ) ;
#19913 = EDGE_CURVE ( 'NONE', #3827, #15181, #27334, .T. ) ;
#19914 = CARTESIAN_POINT ( 'NONE',  ( -12.46528703574805697, 95.79768628210143788, -2.660918448318280838 ) ) ;
#19915 = CARTESIAN_POINT ( 'NONE',  ( 21.00000000000000000, 6.646953231504538984, -0.8156249993854914893 ) ) ;
#19916 = AXIS2_PLACEMENT_3D ( 'NONE', #31790, #28946, #3168 ) ;
#19917 = CARTESIAN_POINT ( 'NONE',  ( -13.50000000000000533, 198.6875000012290400, -23.38268590217984411 ) ) ;
#19918 = EDGE_CURVE ( 'NONE', #16035, #25296, #7252, .T. ) ;
#19919 = CARTESIAN_POINT ( 'NONE',  ( -8.962234695871760692, 121.9601862821014464, 8.715434833791933400 ) ) ;
#19920 = CARTESIAN_POINT ( 'NONE',  ( 22.80587116629411781, -3.604726614523235284, -3.553124999385526728 ) ) ;
#19921 =( BOUNDED_CURVE ( )  B_SPLINE_CURVE ( 2, ( #11352, #3182, #22923, #28771, #14758, #37116, #26301, #23471, #2439 ),
 .UNSPECIFIED., .F., .F. ) 
 B_SPLINE_CURVE_WITH_KNOTS ( ( 3, 2, 2, 2, 3 ),
 ( 0.6875000000000000000, 0.6944444444444444198, 0.7083333333333333703, 0.7222222222222222099, 0.7291666666666667407 ),
 .UNSPECIFIED. ) 
 CURVE ( )  GEOMETRIC_REPRESENTATION_ITEM ( )  RATIONAL_B_SPLINE_CURVE ( ( 0.9330127018922194093, 0.9330127018922194093, 1.000000000000000000, 0.8660254037844387076, 1.000000000000000000, 0.8660254037844387076, 1.000000000000000000, 0.9330127018922187432, 0.9330127018922192983 ) ) 
 REPRESENTATION_ITEM ( '' )  );
#19922 = ADVANCED_FACE ( 'NONE', ( #15974 ), #30371, .F. ) ;
#19923 = CARTESIAN_POINT ( 'NONE',  ( 18.12178482187500350, 245.3218750006145115, 4.985214923628407568 ) ) ;
#19924 = DIRECTION ( 'NONE',  ( 0.000000000000000000, 0.000000000000000000, 1.000000000000000000 ) ) ;
#19925 = CARTESIAN_POINT ( 'NONE',  ( -59.29836230271183695, 204.3130714775002446, -3.149950860017828091 ) ) ;
#19926 = CARTESIAN_POINT ( 'NONE',  ( 7.228626920339068285, 117.0726862821014720, -10.49813415415989581 ) ) ;
#19927 = CARTESIAN_POINT ( 'NONE',  ( 22.56230152254410370, -3.464101615137751278, -4.199999998771048126 ) ) ;
#19928 = CARTESIAN_POINT ( 'NONE',  ( -41.09747103062156981, 213.3500491399821328, -5.571401726697985168 ) ) ;
#19929 = CYLINDRICAL_SURFACE ( 'NONE', #4012, 27.00000000000000000 ) ;
#19930 = CARTESIAN_POINT ( 'NONE',  ( 19.39230484541324273, 241.1486538117967200, 5.999999999999987566 ) ) ;
#19931 = CARTESIAN_POINT ( 'NONE',  ( 0.1745138560725837118, 107.0101862821014578, -15.50000000000000533 ) ) ;
#19932 = CARTESIAN_POINT ( 'NONE',  ( 8.715434833791931624, 9.260186282101429356, 8.962234695871760692 ) ) ;
#19933 = CARTESIAN_POINT ( 'NONE',  ( -3.796722387233375073, 139.7851862821014493, 8.710071997420127943 ) ) ;
#19934 = CARTESIAN_POINT ( 'NONE',  ( 22.80587116629411071, 3.604726614523238837, -2.128124999385546001 ) ) ;
#19935 =( BOUNDED_CURVE ( )  B_SPLINE_CURVE ( 2, ( #36442, #33424, #22062, #24893, #33613, #10117, #25076 ),
 .UNSPECIFIED., .F., .F. ) 
 B_SPLINE_CURVE_WITH_KNOTS ( ( 3, 2, 2, 3 ),
 ( 0.1304347826086973972, 0.1376811594202916600, 0.1449275362318859506, 0.1521739130434802134 ),
 .UNSPECIFIED. ) 
 CURVE ( )  GEOMETRIC_REPRESENTATION_ITEM ( )  RATIONAL_B_SPLINE_CURVE ( ( 0.9999999999999676925, 0.8660254037844710151, 1.000000000000000000, 0.8660254037844387076, 1.000000000000000000, 0.8660254037844028474, 1.000000000000035971 ) ) 
 REPRESENTATION_ITEM ( '' )  );
#19936 = CARTESIAN_POINT ( 'NONE',  ( 23.99999999999999645, 5.196152422706631135, -4.593749998770962684 ) ) ;
#19937 = ORIENTED_EDGE ( 'NONE', *, *, #22077, .T. ) ;
#19938 = CARTESIAN_POINT ( 'NONE',  ( 10.56230152254259735, -3.464101615136883527, -4.799999998771018461 ) ) ;
#19939 = CARTESIAN_POINT ( 'NONE',  ( -8.152565276336710909, 57.84768628210144925, 5.233372021372435512 ) ) ;
#19940 = CARTESIAN_POINT ( 'NONE',  ( 15.24356964374999990, 0.000000000000000000, -0.5906249993854750802 ) ) ;
#19941 = CARTESIAN_POINT ( 'NONE',  ( -20.86978560514296532, 194.8213513911397570, -17.51182845191284798 ) ) ;
#19942 = CARTESIAN_POINT ( 'NONE',  ( 15.00000000000000000, 242.4062500012290400, 0.000000000000000000 ) ) ;
#19943 = CARTESIAN_POINT ( 'NONE',  ( 27.24356964374999635, 195.6218750006145228, -15.72908226750539029 ) ) ;
#19944 = CARTESIAN_POINT ( 'NONE',  ( 5.903039156993664882, 194.9999999999999716, 26.61078777808395657 ) ) ;
#19945 = CARTESIAN_POINT ( 'NONE',  ( 19.56230152254411081, -5.196152422706629359, -5.587499998771034093 ) ) ;
#19946 = CARTESIAN_POINT ( 'NONE',  ( 2.064181346179061460, 31.50231371789854862, 9.465287035748106703 ) ) ;
#19947 = CARTESIAN_POINT ( 'NONE',  ( 24.00000000000000000, -5.196152422706629359, -9.750000000000008882 ) ) ;
#19948 = ORIENTED_EDGE ( 'NONE', *, *, #11558, .T. ) ;
#19949 = CARTESIAN_POINT ( 'NONE',  ( 21.00000000000000000, 248.9593750006145285, 6.646953231504538984 ) ) ;
#19950 = CARTESIAN_POINT ( 'NONE',  ( 4.622313124798831829, 55.36481371789855643, -11.61527771782809282 ) ) ;
#19951 = CARTESIAN_POINT ( 'NONE',  ( 19.68408634441910721, 5.407089921784862696, -9.346874999385523353 ) ) ;
#19952 = CARTESIAN_POINT ( 'NONE',  ( 15.24356964374999990, 3.323476615752268604, -10.19062499938547184 ) ) ;
#19953 = CARTESIAN_POINT ( 'NONE',  ( -15.46528703574811736, 144.2023137178985905, 3.257655550456946436 ) ) ;
#19954 = ORIENTED_EDGE ( 'NONE', *, *, #8299, .T. ) ;
#19955 = CARTESIAN_POINT ( 'NONE',  ( 16.56230152254411436, -7.209453229046482114, -1.434374999385489735 ) ) ;
#19956 = CARTESIAN_POINT ( 'NONE',  ( 0.1745138560725515708, 5.810186282101447830, -12.50000000000000355 ) ) ;
#19957 = CARTESIAN_POINT ( 'NONE',  ( 34.22460179574976991, 5.407089921784862696, 165.3394263477420054 ) ) ;
#19958 = CARTESIAN_POINT ( 'NONE',  ( -46.43377896937850835, 208.3738570449995109, 6.530955311639247363 ) ) ;
#19959 = CARTESIAN_POINT ( 'NONE',  ( 0.000000000000000000, 150.0000000000000000, 7.500000000000000000 ) ) ;
#19960 = CARTESIAN_POINT ( 'NONE',  ( -25.28513278367194772, 195.0000000000000284, -9.605453057530283445 ) ) ;
#19961 = CARTESIAN_POINT ( 'NONE',  ( -38.52455436395490551, 206.6211998817774997, 3.209657149897401585 ) ) ;
#19962 = CARTESIAN_POINT ( 'NONE',  ( -47.03497103062156981, 204.4285982733020148, -3.350049139982115509 ) ) ;
#19963 = CARTESIAN_POINT ( 'NONE',  ( 34.42560472746153977, 5.407089921784857367, 167.6369003702161251 ) ) ;
#19964 = ORIENTED_EDGE ( 'NONE', *, *, #19026, .T. ) ;
#19965 = CARTESIAN_POINT ( 'NONE',  ( -28.98530087525818999, 202.0528329772414224, 1.056834216689858774 ) ) ;
#19966 = CARTESIAN_POINT ( 'NONE',  ( 4.999999999999998224, 216.0000000000000000, -3.514718625761428239 ) ) ;
#19967 = CARTESIAN_POINT ( 'NONE',  ( -5.770363421894122880, 13.96481371789853831, 14.38691631536194393 ) ) ;
#19968 = CARTESIAN_POINT ( 'NONE',  ( -33.37127896937850124, 218.5309553116392465, 2.162041339862725842 ) ) ;
#19969 = CARTESIAN_POINT ( 'NONE',  ( -12.50000000000000355, 3.510186282101451560, -0.1745138560725492671 ) ) ;
#19970 = CARTESIAN_POINT ( 'NONE',  ( 8.962234695871762469, 52.96018628210144641, -8.715434833791931624 ) ) ;
#19971 = CARTESIAN_POINT ( 'NONE',  ( 13.56230152254410726, 5.196152422706636465, -3.675000000000067324 ) ) ;
#19972 = ORIENTED_EDGE ( 'NONE', *, *, #30346, .F. ) ;
#19973 = CARTESIAN_POINT ( 'NONE',  ( 5.770363421893814682, 19.03518628210144570, 14.38691631536207183 ) ) ;
#19974 = CARTESIAN_POINT ( 'NONE',  ( 27.24356964375000345, 195.5281250006145228, -3.336375036156643733E-15 ) ) ;
#19975 = AXIS2_PLACEMENT_3D ( 'NONE', #33028, #1179, #15029 ) ;
#19976 = CARTESIAN_POINT ( 'NONE',  ( -27.24356964375000345, 199.8031250006145285, 0.000000000000000000 ) ) ;
#19977 = CARTESIAN_POINT ( 'NONE',  ( 19.56230152254412502, 5.196152422706637353, -6.450000000000039257 ) ) ;
#19978 = CARTESIAN_POINT ( 'NONE',  ( 18.00000000000000000, 5.196152422706630247, -4.068749998770964993 ) ) ;
#19979 = CYLINDRICAL_SURFACE ( 'NONE', #18438, 5.999999999999998224 ) ;
#19980 = CARTESIAN_POINT ( 'NONE',  ( 21.00000000000000000, 246.1187500012290457, 5.999999999999998224 ) ) ;
#19981 = CARTESIAN_POINT ( 'NONE',  ( 23.87821517812500005, 244.1593750006145171, 4.985214923628404016 ) ) ;
#19982 = CARTESIAN_POINT ( 'NONE',  ( -5.233372021372612259, 97.05231371789855643, 8.152565276336593669 ) ) ;
#19983 = CARTESIAN_POINT ( 'NONE',  ( 23.87821517812499650, 241.6093750006145342, -4.985214923628404904 ) ) ;
#19984 = ORIENTED_EDGE ( 'NONE', *, *, #23790, .F. ) ;
#19985 = CARTESIAN_POINT ( 'NONE',  ( -63.65997103062156981, 215.5714017266979852, 3.350049139982118618 ) ) ;
#19986 = CARTESIAN_POINT ( 'NONE',  ( 26.99999999999999645, 248.5187500012290798, -3.464101615137755275 ) ) ;
#19987 = ORIENTED_EDGE ( 'NONE', *, *, #23373, .T. ) ;
#19988 = CARTESIAN_POINT ( 'NONE',  ( 12.46528703574811558, 112.0023137178985593, -2.660918448318005947 ) ) ;
#19989 = CARTESIAN_POINT ( 'NONE',  ( 10.31873187879410736, 0.000000000000000000, -0.6468749993855105185 ) ) ;
#19990 = CARTESIAN_POINT ( 'NONE',  ( 33.82423010250274586, -5.407089921784855591, 160.7631569533830600 ) ) ;
#19991 = CARTESIAN_POINT ( 'NONE',  ( 15.24356964374999990, 3.323476615752268604, -1.640624999385488891 ) ) ;
#19992 = CARTESIAN_POINT ( 'NONE',  ( -13.62178482187500528, 199.3343750006145569, -23.59362340125807123 ) ) ;
#19993 = VERTEX_POINT ( 'NONE', #36045 ) ;
#19994 = ORIENTED_EDGE ( 'NONE', *, *, #36236, .F. ) ;
#19995 = VECTOR ( 'NONE', #9897, 1000.000000000000114 ) ;
#19996 = VERTEX_POINT ( 'NONE', #4208 ) ;
#19997 = CARTESIAN_POINT ( 'NONE',  ( 18.00000000000000355, -5.196152422706632912, -7.068749998770940124 ) ) ;
#19998 = CARTESIAN_POINT ( 'NONE',  ( 18.12178482187499640, 4.985214923628404904, -2.465624999385462868 ) ) ;
#19999 = CARTESIAN_POINT ( 'NONE',  ( 36.56647878446842981, 3.464101615137479495, 159.0833872022827791 ) ) ;
#20000 = CARTESIAN_POINT ( 'NONE',  ( 24.99999999999999289, 0.000000000000000000, -8.000000000000000000 ) ) ;
#20001 = CARTESIAN_POINT ( 'NONE',  ( -4.622313124798576922, 60.43518628210145494, -11.61527771782819762 ) ) ;
#20002 = CARTESIAN_POINT ( 'NONE',  ( -44.25669563604516554, 209.8844732041982013, -6.500000000000000888 ) ) ;
#20003 = CARTESIAN_POINT ( 'NONE',  ( 5.205286459874319149, 215.9230175775472276, 0.9779651927393356869 ) ) ;
#20004 = CARTESIAN_POINT ( 'NONE',  ( -42.67336230271183695, 213.9548777149308023, 2.149950860017852960 ) ) ;
#20005 = CARTESIAN_POINT ( 'NONE',  ( 33.93414378867374381, 5.196152422706631135, 163.4168002589758260 ) ) ;
#20006 = CARTESIAN_POINT ( 'NONE',  ( 4.944772684328420986, 104.8148137178985593, 11.48171059495408208 ) ) ;
#20007 = CARTESIAN_POINT ( 'NONE',  ( -67.81622103062157692, 211.0902445701382533, 4.530955311639240257 ) ) ;
#20008 = CARTESIAN_POINT ( 'NONE',  ( -43.86830436395490551, 209.8844732041983150, 8.500000000000003553 ) ) ;
#20009 = CARTESIAN_POINT ( 'NONE',  ( 18.12178482187499640, 4.985214923628404904, -4.378124999385474503 ) ) ;
#20010 = CARTESIAN_POINT ( 'NONE',  ( 20.99999999999999645, -6.928203230275506996, -1.687500000000023981 ) ) ;
#20011 = CARTESIAN_POINT ( 'NONE',  ( 6.092822981423662299, 68.01481371789854791, 14.25334919248795096 ) ) ;
#20012 = CARTESIAN_POINT ( 'NONE',  ( -32.77752896937850124, 213.3500491399821613, 5.571401726697954970 ) ) ;
#20013 = ORIENTED_EDGE ( 'NONE', *, *, #5504, .F. ) ;
#20014 =( BOUNDED_CURVE ( )  B_SPLINE_CURVE ( 2, ( #23745, #418, #23556, #34916, #35100, #9149, #34545 ),
 .UNSPECIFIED., .F., .F. ) 
 B_SPLINE_CURVE_WITH_KNOTS ( ( 3, 2, 2, 3 ),
 ( 0.4782608695652184050, 0.4855072463768126401, 0.4927536231884069862, 0.5000000000000012212 ),
 .UNSPECIFIED. ) 
 CURVE ( )  GEOMETRIC_REPRESENTATION_ITEM ( )  RATIONAL_B_SPLINE_CURVE ( ( 0.9999999999999815703, 0.8660254037844571373, 1.000000000000000000, 0.8660254037844387076, 1.000000000000000000, 0.8660254037844161701, 1.000000000000022649 ) ) 
 REPRESENTATION_ITEM ( '' )  );
#20015 = CARTESIAN_POINT ( 'NONE',  ( 22.60769515458672885, 242.2736538117966916, -5.999999999999998224 ) ) ;
#20016 = CARTESIAN_POINT ( 'NONE',  ( -11.48171059495397373, 96.08518628210146062, -4.944772684328680334 ) ) ;
#20017 = CARTESIAN_POINT ( 'NONE',  ( -13.04141134922759804, 68.77268628210143220, -8.927990412390657937 ) ) ;
#20018 = CARTESIAN_POINT ( 'NONE',  ( 20.99999999999995026, 243.1375000000000455, -5.999999999999998224 ) ) ;
#20019 = CARTESIAN_POINT ( 'NONE',  ( 30.76498388983966237, 7.209453229046482114, 161.6142765964977741 ) ) ;
#20020 = AXIS2_PLACEMENT_3D ( 'NONE', #12936, #18068, #21103 ) ;
#20021 = CARTESIAN_POINT ( 'NONE',  ( -10.83675517735155047, 59.86018628210145209, -11.08355503943142750 ) ) ;
#20022 = CARTESIAN_POINT ( 'NONE',  ( 10.31873187879411091, -3.604726614523240613, -6.853124999385484806 ) ) ;
#20023 = DIRECTION ( 'NONE',  ( 0.000000000000000000, 0.000000000000000000, -1.000000000000000000 ) ) ;
#20024 = CARTESIAN_POINT ( 'NONE',  ( -64.05580436395490551, 216.5000000000000000, 0.1155267958017343610 ) ) ;
#20025 = EDGE_CURVE ( 'NONE', #25851, #28581, #3831, .T. ) ;
#20026 = CARTESIAN_POINT ( 'NONE',  ( 19.39230484541326760, 243.3986538117966916, 5.999999999999999112 ) ) ;
#20027 = CARTESIAN_POINT ( 'NONE',  ( -2.311890736173176641, 42.32268628210145067, -12.53471296425194836 ) ) ;
#20028 = CARTESIAN_POINT ( 'NONE',  ( 13.49999999999999645, 198.0500000000000114, -23.38268590217984766 ) ) ;
#20029 = CARTESIAN_POINT ( 'NONE',  ( 26.99999999999999645, 7.347880794884117764E-16, -1.574999999999993072 ) ) ;
#20030 = CARTESIAN_POINT ( 'NONE',  ( -6.840914352312096547, 29.96018628210143575, 6.594114490232313663 ) ) ;
#20031 = CARTESIAN_POINT ( 'NONE',  ( 23.87821517812500005, 248.2093750006145285, 4.985214923628404016 ) ) ;
#20032 = VERTEX_POINT ( 'NONE', #21481 ) ;
#20033 = CARTESIAN_POINT ( 'NONE',  ( 26.99999999999999645, 3.464101615137755275, -4.687500000000006217 ) ) ;
#20034 = LINE ( 'NONE', #28541, #31224 ) ;
#20035 = CARTESIAN_POINT ( 'NONE',  ( 33.71474070067601048, 5.407089921784862696, 159.5116873639053097 ) ) ;
#20036 = CARTESIAN_POINT ( 'NONE',  ( 22.80587116629410716, 7.646167579472015790E-16, -3.065624999385535787 ) ) ;
#20037 = CARTESIAN_POINT ( 'NONE',  ( 25.10569328411516921, 3.604726614523236616, 168.5652166982980305 ) ) ;
#20038 = CARTESIAN_POINT ( 'NONE',  ( 15.00000000000000178, 244.1875000000000000, 3.464101615137757051 ) ) ;
#20039 = CARTESIAN_POINT ( 'NONE',  ( -27.00000000000000355, 198.6125000000000114, -15.58845726811989429 ) ) ;
#20040 = EDGE_CURVE ( 'NONE', #4550, #10335, #24676, .T. ) ;
#20041 =( BOUNDED_CURVE ( )  B_SPLINE_CURVE ( 2, ( #23814, #15472, #488, #35550, #6748, #9032, #32333, #30056, #3711 ),
 .UNSPECIFIED., .F., .F. ) 
 B_SPLINE_CURVE_WITH_KNOTS ( ( 3, 2, 2, 2, 3 ),
 ( 0.6630434782608695121, 0.6666666666666666297, 0.6739130434782608647, 0.6811594202898550998, 0.6847826086956522174 ),
 .UNSPECIFIED. ) 
 CURVE ( )  GEOMETRIC_REPRESENTATION_ITEM ( )  RATIONAL_B_SPLINE_CURVE ( ( 0.9330127018922192983, 0.9330127018922182991, 1.000000000000000000, 0.8660254037844387076, 1.000000000000000000, 0.8660254037844387076, 1.000000000000000000, 0.9330127018922182991, 0.9330127018922192983 ) ) 
 REPRESENTATION_ITEM ( '' )  );
#20042 = CARTESIAN_POINT ( 'NONE',  ( 0.1745138560725515708, 61.01018628210145067, -12.50000000000000355 ) ) ;
#20043 = EDGE_LOOP ( 'NONE', ( #13889, #18489, #18319, #28300 ) ) ;
#20044 = VERTEX_POINT ( 'NONE', #983 ) ;
#20045 = DIRECTION ( 'NONE',  ( -0.000000000000000000, 1.000000000000000000, -0.000000000000000000 ) ) ;
#20046 = CARTESIAN_POINT ( 'NONE',  ( 26.99999999999999645, 196.3250000012290570, -15.58845726811990495 ) ) ;
#20047 = CARTESIAN_POINT ( 'NONE',  ( -2.908627838312453306, 41.27731371789855075, 15.53471296425188797 ) ) ;
#20048 = CARTESIAN_POINT ( 'NONE',  ( 15.24356964374999990, 3.323476615752268604, -8.840624999385484628 ) ) ;
#20049 = CARTESIAN_POINT ( 'NONE',  ( 21.00000000000000000, 242.7718750006145854, 6.646953231504538984 ) ) ;
#20050 = AXIS2_PLACEMENT_3D ( 'NONE', #37360, #29209, #14824 ) ;
#20051 = CARTESIAN_POINT ( 'NONE',  ( -42.08705436395490551, 206.7903428501026042, -3.378800118222489157 ) ) ;
#20052 = ADVANCED_FACE ( 'NONE', ( #15593 ), #4021, .F. ) ;
#20053 = FACE_OUTER_BOUND ( 'NONE', #24464, .T. ) ;
#20054 = CARTESIAN_POINT ( 'NONE',  ( 24.63014976274829593, 3.604726614523240613, 163.1297293768349164 ) ) ;
#20055 = CARTESIAN_POINT ( 'NONE',  ( 7.954856959092311719, 28.62731371789854506, -5.529263428287300108 ) ) ;
#20056 = CARTESIAN_POINT ( 'NONE',  ( -68.80580436395490551, 216.5000000000000000, 0.1155267958017343610 ) ) ;
#20057 = CARTESIAN_POINT ( 'NONE',  ( 14.95941216476289526, 420.9868634618175065, 0.000000000000000000 ) ) ;
#20058 = CARTESIAN_POINT ( 'NONE',  ( 25.58178997548098366, 194.9999999999998863, 9.109611009433765005 ) ) ;
#20059 = CARTESIAN_POINT ( 'NONE',  ( -1.926257025242585782E-15, 195.2468750006145513, -31.45816453501075927 ) ) ;
#20060 = CARTESIAN_POINT ( 'NONE',  ( 11.61527771782809637, 11.66481371789854293, 4.622313124798827388 ) ) ;
#20061 = ORIENTED_EDGE ( 'NONE', *, *, #1566, .F. ) ;
#20062 = CARTESIAN_POINT ( 'NONE',  ( -4.622313124798576922, 60.43518628210145494, -11.61527771782819762 ) ) ;
#20063 = CARTESIAN_POINT ( 'NONE',  ( 34.28712454680172783, 5.196152422706631135, 167.4513887862474064 ) ) ;
#20064 = CARTESIAN_POINT ( 'NONE',  ( 0.000000000000000000, 200.0000000000000000, 0.000000000000000000 ) ) ;
#20065 = CARTESIAN_POINT ( 'NONE',  ( 33.83389300460937932, 6.917534487978453051, 159.1041492265317174 ) ) ;
#20066 = CARTESIAN_POINT ( 'NONE',  ( 23.99999999999999645, 5.196152422706631135, -1.893749998770954956 ) ) ;
#20067 = CARTESIAN_POINT ( 'NONE',  ( 22.80587116629411781, -3.604726614523238837, -8.559374999385489957 ) ) ;
#20068 = CARTESIAN_POINT ( 'NONE',  ( -27.00000000000000355, 196.9625000012290172, 0.000000000000000000 ) ) ;
#20069 = CARTESIAN_POINT ( 'NONE',  ( -6.840914352312096547, 75.96018628210144641, 6.594114490232313663 ) ) ;
#20070 = LINE ( 'NONE', #5456, #17087 ) ;
#20071 = CARTESIAN_POINT ( 'NONE',  ( 12.53471296425194836, 109.0226862821014606, -2.311890736173178418 ) ) ;
#20072 = CARTESIAN_POINT ( 'NONE',  ( 26.99999999999999645, 248.8374999999999773, 3.464101615137751278 ) ) ;
#20073 = CARTESIAN_POINT ( 'NONE',  ( 26.99999999999999645, 240.3812500012290343, -7.347880794884117764E-16 ) ) ;
#20074 = EDGE_LOOP ( 'NONE', ( #24941, #18367 ) ) ;
#20075 = CARTESIAN_POINT ( 'NONE',  ( 24.67427235751429748, 3.604726614523236616, 163.6340529427438639 ) ) ;
#20076 = CARTESIAN_POINT ( 'NONE',  ( 21.00000000000000000, 6.646953231504538984, -6.553124999385445903 ) ) ;
#20078 = EDGE_CURVE ( 'NONE', #12845, #17150, #796, .T. ) ;
#20077 = CARTESIAN_POINT ( 'NONE',  ( 27.24356964374999279, 196.0718750006145399, -15.72908226750539207 ) ) ;
#20079 = CARTESIAN_POINT ( 'NONE',  ( 37.52733936471412335, 3.604726614523243278, 167.2714256424211499 ) ) ;
#20080 = CARTESIAN_POINT ( 'NONE',  ( 25.13180852339276683, -3.464101615137761048, 166.0690670014023453 ) ) ;
#20081 = LINE ( 'NONE', #3001, #19898 ) ;
#20082 = CARTESIAN_POINT ( 'NONE',  ( 21.00000000000000000, 240.7468750006145228, -6.646953231504538984 ) ) ;
#20083 = CARTESIAN_POINT ( 'NONE',  ( 27.24356964375000345, 199.1281250006145171, -3.336375036156643733E-15 ) ) ;
#20084 = CARTESIAN_POINT ( 'NONE',  ( -10.49813415416004858, 125.2273137178985820, 7.228626920338839135 ) ) ;
#20085 = CARTESIAN_POINT ( 'NONE',  ( -10.69584247140444866, 122.2476862821014549, 6.932735513423972762 ) ) ;
#20087 = ORIENTED_EDGE ( 'NONE', *, *, #1288, .T. ) ;
#20086 = ORIENTED_EDGE ( 'NONE', *, *, #14124, .F. ) ;
#20088 = CARTESIAN_POINT ( 'NONE',  ( -13.62178482187498396, 198.0781250006145342, 23.59362340125808188 ) ) ;
#20089 = CARTESIAN_POINT ( 'NONE',  ( 26.75643035624999655, 241.4593750006145285, -3.323476615752271712 ) ) ;
#20090 = LINE ( 'NONE', #6746, #2576 ) ;
#20091 = CARTESIAN_POINT ( 'NONE',  ( -3.257655550456946880, 91.30231371789854222, -15.46528703574811736 ) ) ;
#20092 = CARTESIAN_POINT ( 'NONE',  ( 0.1745138560725515708, 88.61018628210146630, -12.50000000000000355 ) ) ;
#20093 = CARTESIAN_POINT ( 'NONE',  ( 15.24356964374999990, 0.000000000000000000, -0.7031249993854904456 ) ) ;
#20094 = CARTESIAN_POINT ( 'NONE',  ( -1.909035429704832693E-15, 197.3000000012290513, -31.17691453623979214 ) ) ;
#20095 = CARTESIAN_POINT ( 'NONE',  ( -9.465287035748106703, 70.60231371789853938, 2.064181346179061460 ) ) ;
#20096 = CARTESIAN_POINT ( 'NONE',  ( 10.31873187879411091, 0.000000000000000000, -1.940624999385548444 ) ) ;
#20097 = CARTESIAN_POINT ( 'NONE',  ( 20.99999999999999645, 241.3093750006145228, 6.646953231504538984 ) ) ;
#20098 = CARTESIAN_POINT ( 'NONE',  ( 22.56230152254412147, 7.347880794884125653E-16, -8.325000000000027711 ) ) ;
#20099 = CARTESIAN_POINT ( 'NONE',  ( 12.53471296425194836, 127.4226862821014663, -2.311890736173178418 ) ) ;
#20100 = CARTESIAN_POINT ( 'NONE',  ( 13.56230152254411614, -5.196152422706632912, -4.312499998771063048 ) ) ;
#20101 = EDGE_CURVE ( 'NONE', #13088, #11631, #841, .T. ) ;
#20102 = CARTESIAN_POINT ( 'NONE',  ( -47.23288769728823411, 203.5309553116391612, -1.857196546604028775 ) ) ;
#20103 = CARTESIAN_POINT ( 'NONE',  ( 0.000000000000000000, 0.000000000000000000, -5.000000000000000000 ) ) ;
#20104 = CARTESIAN_POINT ( 'NONE',  ( 25.01087993033039325, 0.000000000000000000, 164.6868468578000488 ) ) ;
#20105 = CARTESIAN_POINT ( 'NONE',  ( 13.04141134922759804, 100.9726862821014635, 8.927990412390657937 ) ) ;
#20106 = CARTESIAN_POINT ( 'NONE',  ( 8.962234695871762469, 16.16018628210144570, -8.715434833791931624 ) ) ;
#20107 = CARTESIAN_POINT ( 'NONE',  ( -20.80563922340697403, 195.0000000000000284, -17.20829382900668492 ) ) ;
#20108 = CARTESIAN_POINT ( 'NONE',  ( 18.00000000000000000, 241.4312500012290457, -5.196152422706630247 ) ) ;
#20109 = CARTESIAN_POINT ( 'NONE',  ( -5.233372021372430183, 133.7476862821013981, -8.152565276336710909 ) ) ;
#20110 = CARTESIAN_POINT ( 'NONE',  ( 10.56230152254426891, 3.464101615137844981, -8.924999998771019349 ) ) ;
#20111 = ORIENTED_EDGE ( 'NONE', *, *, #18939, .T. ) ;
#20112 = DIRECTION ( 'NONE',  ( 0.000000000000000000, -1.000000000000000000, 0.000000000000000000 ) ) ;
#20113 = CARTESIAN_POINT ( 'NONE',  ( -0.1745138560725182642, 56.41018628210145636, 9.500000000000005329 ) ) ;
#20114 = CARTESIAN_POINT ( 'NONE',  ( 23.87821517812500005, -4.985214923628404016, -0.8906249993854697955 ) ) ;
#20115 = ADVANCED_FACE ( 'NONE', ( #35479, #15786 ), #6494, .F. ) ;
#20116 = CARTESIAN_POINT ( 'NONE',  ( 22.60769515458672885, 241.1325961894323484, 5.999999999999997335 ) ) ;
#20117 = CARTESIAN_POINT ( 'NONE',  ( 20.99999999999999645, 185.0294372515228645, 0.000000000000000000 ) ) ;
#20118 = CARTESIAN_POINT ( 'NONE',  ( -27.24356964375000345, 194.8857344423842619, -9.915847606754343957 ) ) ;
#20119 = DIRECTION ( 'NONE',  ( 1.000000000000000000, 0.000000000000000000, 0.000000000000000000 ) ) ;
#20120 = CARTESIAN_POINT ( 'NONE',  ( 1.120210788295102201E-13, 196.8500000012290343, -27.00000000000000711 ) ) ;
#20121 = CARTESIAN_POINT ( 'NONE',  ( 9.534712964251900402, 29.77731371789854364, 1.715153634034445540 ) ) ;
#20122 = CARTESIAN_POINT ( 'NONE',  ( -27.24356964375000345, 199.8593750006145342, 0.000000000000000000 ) ) ;
#20123 = EDGE_CURVE ( 'NONE', #28188, #30148, #24499, .T. ) ;
#20124 = EDGE_LOOP ( 'NONE', ( #21656, #21215, #6463, #22464, #20880 ) ) ;
#20125 = VERTEX_POINT ( 'NONE', #35668 ) ;
#20126 = CARTESIAN_POINT ( 'NONE',  ( 26.75643035624999655, 248.5843750006145001, 3.323476615752267715 ) ) ;
#20127 = CARTESIAN_POINT ( 'NONE',  ( 11.48171059495408208, 47.31481371789855928, -4.944772684328420986 ) ) ;
#20128 = CARTESIAN_POINT ( 'NONE',  ( 10.31873187879410736, 0.000000000000000000, -7.846874999385494931 ) ) ;
#20129 = CARTESIAN_POINT ( 'NONE',  ( 23.87821517812499650, 4.985214923628404904, -8.953124999385497773 ) ) ;
#20130 = CARTESIAN_POINT ( 'NONE',  ( 3.257655550456945548, 141.9023137178985507, 15.46528703574811736 ) ) ;
#20131 =( BOUNDED_CURVE ( )  B_SPLINE_CURVE ( 2, ( #35772, #27067, #32185, #30098, #17792, #4130, #9630 ),
 .UNSPECIFIED., .F., .F. ) 
 B_SPLINE_CURVE_WITH_KNOTS ( ( 3, 2, 2, 3 ),
 ( 0.2608695652173909085, 0.2681159420289850326, 0.2753623188405790456, 0.2826086956521731142 ),
 .UNSPECIFIED. ) 
 CURVE ( )  GEOMETRIC_REPRESENTATION_ITEM ( )  RATIONAL_B_SPLINE_CURVE ( ( 1.000000000000007105, 0.8660254037844313801, 1.000000000000000000, 0.8660254037844387076, 1.000000000000000000, 0.8660254037844530295, 0.9999999999999856781 ) ) 
 REPRESENTATION_ITEM ( '' )  );
#20132 = ORIENTED_EDGE ( 'NONE', *, *, #14224, .F. ) ;
#20133 = CARTESIAN_POINT ( 'NONE',  ( 13.44051670066911086, 5.407089921784862696, -3.421874999385537741 ) ) ;
#20134 = CARTESIAN_POINT ( 'NONE',  ( 13.62178482187499640, 199.2031250006145342, -23.59362340125807123 ) ) ;
#20135 = CARTESIAN_POINT ( 'NONE',  ( 27.98518077736123288, -5.407089921784865361, 165.6594454903691087 ) ) ;
#20136 = CARTESIAN_POINT ( 'NONE',  ( -48.21502896937850124, 215.5714017266979567, -3.350049139982168800 ) ) ;
#20137 = DIRECTION ( 'NONE',  ( -1.000000000000000000, 0.000000000000000000, 0.000000000000000000 ) ) ;
#20138 = SURFACE_STYLE_USAGE ( .BOTH. , #5347 ) ;
#20139 = CARTESIAN_POINT ( 'NONE',  ( 21.00000000000000355, 0.000000000000000000, 50.00000000000001421 ) ) ;
#20140 = CARTESIAN_POINT ( 'NONE',  ( -56.72544563604517265, 213.3788001182224718, 3.209657149897419348 ) ) ;
#20141 = CIRCLE ( 'NONE', #9860, 27.00000000000000000 ) ;
#20142 = CARTESIAN_POINT ( 'NONE',  ( -43.27455436395490551, 205.1570982666397356, 4.673758765035198159 ) ) ;
#20143 = CARTESIAN_POINT ( 'NONE',  ( 37.57146195948011069, 3.604726614523238837, 167.7757492083300690 ) ) ;
#20144 = EDGE_LOOP ( 'NONE', ( #15203, #22278, #34251, #4538 ) ) ;
#20145 = CARTESIAN_POINT ( 'NONE',  ( 20.99999999999999645, 185.0294372515228645, 5.999999999999999112 ) ) ;
#20146 = CARTESIAN_POINT ( 'NONE',  ( 24.00000000000000000, -5.196152422706629359, -7.050000000000000711 ) ) ;
#20147 = CARTESIAN_POINT ( 'NONE',  ( -14.38691631536193860, 25.46481371789855075, -5.770363421894132649 ) ) ;
#20148 = CARTESIAN_POINT ( 'NONE',  ( -59.50372103062157692, 218.5309553116391896, -2.162041339862839084 ) ) ;
#20149 = CARTESIAN_POINT ( 'NONE',  ( 2.660918448318279950, 15.29768628210143078, -12.46528703574805697 ) ) ;
#20150 = ADVANCED_FACE ( 'NONE', ( #6682 ), #18640, .T. ) ;
#20151 = CARTESIAN_POINT ( 'NONE',  ( 4.622313124798573369, 55.83518628210144641, 11.61527771782819940 ) ) ;
#20152 = CARTESIAN_POINT ( 'NONE',  ( 22.56230152254411792, 7.347880794884125653E-16, -4.725000000000035172 ) ) ;
#20153 = ORIENTED_EDGE ( 'NONE', *, *, #26807, .F. ) ;
#20154 = CARTESIAN_POINT ( 'NONE',  ( -27.00000000000000355, 198.7625000012290286, 0.000000000000000000 ) ) ;
#20155 = CARTESIAN_POINT ( 'NONE',  ( 13.62178482187501416, 196.4093750006145456, 23.59362340125806767 ) ) ;
#20156 = CARTESIAN_POINT ( 'NONE',  ( 24.93243976185750554, 0.000000000000000000, 163.7902716295174912 ) ) ;
#20157 = MANIFOLD_SOLID_BREP ( 'LPattern2', #4744 ) ;
#20158 = PLANE ( 'NONE',  #23479 ) ;
#20159 = ADVANCED_FACE ( 'NONE', ( #27891, #11202 ), #4393, .F. ) ;
#20160 = DIRECTION ( 'NONE',  ( 1.000000000000000000, 0.000000000000000000, 0.000000000000000000 ) ) ;
#20161 = DIRECTION ( 'NONE',  ( 1.000000000000000000, 6.123233995736766036E-17, -0.000000000000000000 ) ) ;
#20162 = CARTESIAN_POINT ( 'NONE',  ( 26.75643035624999655, 246.4843750006145342, -7.049594010296217766E-16 ) ) ;
#20163 = CARTESIAN_POINT ( 'NONE',  ( 3.474262827703532341, 92.16481371789855359, -8.843639120294245259 ) ) ;
#20164 = CARTESIAN_POINT ( 'NONE',  ( 20.99999999999999645, 240.7468750006145228, -6.646953231504538984 ) ) ;
#20165 = ORIENTED_EDGE ( 'NONE', *, *, #31820, .T. ) ;
#20166 = CARTESIAN_POINT ( 'NONE',  ( -59.10788769728823411, 216.4690446883607535, 1.857196546604031662 ) ) ;
#20167 = DIRECTION ( 'NONE',  ( -0.000000000000000000, 0.000000000000000000, 1.000000000000000000 ) ) ;
#20168 = CARTESIAN_POINT ( 'NONE',  ( 18.00000000000000355, 245.1812500012290457, 5.196152422706632912 ) ) ;
#20169 = ORIENTED_EDGE ( 'NONE', *, *, #15827, .T. ) ;
#20170 = CARTESIAN_POINT ( 'NONE',  ( -11.48171059495408208, 97.91481371789856780, 4.944772684328421875 ) ) ;
#20171 = CARTESIAN_POINT ( 'NONE',  ( 13.44051670066910908, 5.407089921784862696, -2.071874999385547866 ) ) ;
#20172 = CARTESIAN_POINT ( 'NONE',  ( 15.00000000000000000, 246.8125000000000000, -3.464101615137752610 ) ) ;
#20173 = CARTESIAN_POINT ( 'NONE',  ( 18.12178482187499640, 4.985214923628404904, -3.028124999385484184 ) ) ;
#20174 = CARTESIAN_POINT ( 'NONE',  ( 2.311890736173452865, 73.47731371789856780, -12.53471296425189152 ) ) ;
#20175 = CARTESIAN_POINT ( 'NONE',  ( 13.62178482187501416, 199.1093750006145342, 23.59362340125806767 ) ) ;
#20176 = ORIENTED_EDGE ( 'NONE', *, *, #7343, .T. ) ;
#20177 = ORIENTED_EDGE ( 'NONE', *, *, #17571, .F. ) ;
#20178 = VERTEX_POINT ( 'NONE', #30930 ) ;
#20179 = CARTESIAN_POINT ( 'NONE',  ( 23.99999999999999645, 5.196152422706631135, -6.393749998770958953 ) ) ;
#20180 = CARTESIAN_POINT ( 'NONE',  ( 15.24356964375000167, -3.323476615752272600, -2.353124999385463489 ) ) ;
#20181 = CARTESIAN_POINT ( 'NONE',  ( 19.39230484541326049, 241.8638461906614054, -5.999999999999997335 ) ) ;
#20182 = CARTESIAN_POINT ( 'NONE',  ( 23.87821517812499650, 246.4468750006145115, -4.985214923628404904 ) ) ;
#20183 = CARTESIAN_POINT ( 'NONE',  ( 4.622313124798573369, 55.83518628210144641, 11.61527771782819940 ) ) ;
#20184 = CARTESIAN_POINT ( 'NONE',  ( -55.93377896937849414, 208.3738570449995109, 6.530955311639247363 ) ) ;
#20185 = CARTESIAN_POINT ( 'NONE',  ( 15.81961138684103929, 215.1803886131357615, -3.965927053044179917 ) ) ;
#20186 = CARTESIAN_POINT ( 'NONE',  ( -45.64211230271183695, 205.5309553116392465, 1.321298161741817356 ) ) ;
#20187 =( BOUNDED_CURVE ( )  B_SPLINE_CURVE ( 2, ( #4800, #10305, #1584, #18673, #10121 ),
 .UNSPECIFIED., .F., .F. ) 
 B_SPLINE_CURVE_WITH_KNOTS ( ( 3, 2, 3 ),
 ( 0.7608695652173906865, 0.7681159420289852546, 0.7728738931639650422 ),
 .UNSPECIFIED. ) 
 CURVE ( )  GEOMETRIC_REPRESENTATION_ITEM ( )  RATIONAL_B_SPLINE_CURVE ( ( 1.000000000000012212, 0.8660254037844263841, 1.000000000000000000, 0.9120326476671286597, 0.9395835397632965602 ) ) 
 REPRESENTATION_ITEM ( '' )  );
#20188 = CARTESIAN_POINT ( 'NONE',  ( 33.89492370443730351, 5.196152422706631135, 162.9685126448345329 ) ) ;
#20189 = CARTESIAN_POINT ( 'NONE',  ( -2.660918448318004614, 109.7023137178985621, -12.46528703574811558 ) ) ;
#20190 = CARTESIAN_POINT ( 'NONE',  ( -57.72247103062156270, 207.6499508600178387, 3.839350919129076445 ) ) ;
#20191 = CARTESIAN_POINT ( 'NONE',  ( -50.20163769728823411, 217.4189793300686233, -4.149950860017907139 ) ) ;
#20192 = CARTESIAN_POINT ( 'NONE',  ( 15.24356964375000167, -3.323476615752272600, -5.165624999385461713 ) ) ;
#20193 = DIRECTION ( 'NONE',  ( 0.000000000000000000, 0.000000000000000000, 1.000000000000000000 ) ) ;
#20194 = CARTESIAN_POINT ( 'NONE',  ( -10.83675517735179028, 78.93981371789855928, 11.08355503943118947 ) ) ;
#20195 = CARTESIAN_POINT ( 'NONE',  ( -37.13169563604516554, 210.1155267958017703, 6.500000000000000888 ) ) ;
#20196 = VERTEX_POINT ( 'NONE', #5326 ) ;
#20197 = CARTESIAN_POINT ( 'NONE',  ( -3.253724281355068545E-15, 196.2874999999999659, -27.00000000000000355 ) ) ;
#20198 = CARTESIAN_POINT ( 'NONE',  ( -10.49813415415989581, 105.5726862821014578, -7.228626920339068285 ) ) ;
#20199 = CARTESIAN_POINT ( 'NONE',  ( -14.38691631536207183, 48.93518628210144072, 5.770363421893814682 ) ) ;
#20200 = CARTESIAN_POINT ( 'NONE',  ( 26.99999999999999645, 7.347880794884117764E-16, -6.018749998770944742 ) ) ;
#20201 = VECTOR ( 'NONE', #15218, 1000.000000000000000 ) ;
#20202 = CARTESIAN_POINT ( 'NONE',  ( 37.08938175740716758, -3.604726614523238837, 162.2655472845100917 ) ) ;
#20203 = CARTESIAN_POINT ( 'NONE',  ( 14.25334919248782661, 73.08518628210143220, 6.092822981423971385 ) ) ;
#20204 = CARTESIAN_POINT ( 'NONE',  ( 13.44051670066911086, 5.407089921784856479, -9.215624999385523708 ) ) ;
#20205 = CARTESIAN_POINT ( 'NONE',  ( -51.40635080957665792, 236.9611623878118394, 0.4999999999999997780 ) ) ;
#20206 = CARTESIAN_POINT ( 'NONE',  ( -45.05580436395489841, 216.5000000000000000, 0.1155267958017343610 ) ) ;
#20207 = CARTESIAN_POINT ( 'NONE',  ( 11.41114437030077866, 3.308917692602460825, -9.999999999999996447 ) ) ;
#20208 = CARTESIAN_POINT ( 'NONE',  ( -4.944772684328673229, 38.58518628210144641, 11.48171059495397728 ) ) ;
#20209 = CARTESIAN_POINT ( 'NONE',  ( -27.00000000000000355, 196.4000000000000057, 0.000000000000000000 ) ) ;
#20210 = CARTESIAN_POINT ( 'NONE',  ( -3.253724281355068545E-15, 197.3000000012290229, -27.00000000000000355 ) ) ;
#20211 = CARTESIAN_POINT ( 'NONE',  ( -7.954856959092191815, 4.372686282101438948, -5.529263428287477744 ) ) ;
#20212 = CARTESIAN_POINT ( 'NONE',  ( 18.12178482187500350, 249.0343750006145456, 4.985214923628407568 ) ) ;
#20213 = VECTOR ( 'NONE', #28431, 1000.000000000000000 ) ;
#20214 = ORIENTED_EDGE ( 'NONE', *, *, #36489, .T. ) ;
#20215 = CARTESIAN_POINT ( 'NONE',  ( 18.00000000000000000, 5.196152422706630247, -4.124999999999989342 ) ) ;
#20216 = MECHANICAL_DESIGN_GEOMETRIC_PRESENTATION_REPRESENTATION (  '', ( #9309 ), #6902 ) ;
#20217 = CARTESIAN_POINT ( 'NONE',  ( 26.99999999999999645, 243.5124999999999602, -3.464101615137755275 ) ) ;
#20218 = CARTESIAN_POINT ( 'NONE',  ( 30.76498388983966237, 7.209453229046482114, 161.6142765964977741 ) ) ;
#20219 = CARTESIAN_POINT ( 'NONE',  ( 16.56230152254411436, -7.209453229046475009, -4.528124999385512162 ) ) ;
#20220 = CARTESIAN_POINT ( 'NONE',  ( 25.18740179294109183, 0.000000000000000000, 169.4991492277590339 ) ) ;
#20221 = CARTESIAN_POINT ( 'NONE',  ( 24.00000000000000000, 241.6000000000000227, 5.196152422706629359 ) ) ;
#20222 = DIRECTION ( 'NONE',  ( 0.9961946980917462113, 0.000000000000000000, -0.08715574274765118534 ) ) ;
#20223 = VECTOR ( 'NONE', #18739, 1000.000000000000000 ) ;
#20224 = CARTESIAN_POINT ( 'NONE',  ( 6.932735513423970097, 64.74768628210145494, 10.69584247140445044 ) ) ;
#20225 = ORIENTED_EDGE ( 'NONE', *, *, #11409, .T. ) ;
#20226 = ORIENTED_EDGE ( 'NONE', *, *, #23079, .T. ) ;
#20227 = LINE ( 'NONE', #23623, #30947 ) ;
#20228 = CARTESIAN_POINT ( 'NONE',  ( 13.50000000000001421, 195.3125000012290400, 23.38268590217984055 ) ) ;
#20229 = CARTESIAN_POINT ( 'NONE',  ( -47.00000000000000711, 237.0000000000000000, 2.500000000000001776 ) ) ;
#20230 = CARTESIAN_POINT ( 'NONE',  ( 2.908627838312458636, 45.87731371789854506, -15.53471296425188442 ) ) ;
#20231 = MANIFOLD_SOLID_BREP ( 'M5 Clearance Hole1', #34394 ) ;
#20232 = DIRECTION ( 'NONE',  ( 0.000000000000000000, 0.000000000000000000, -1.000000000000000000 ) ) ;
#20233 = CARTESIAN_POINT ( 'NONE',  ( 15.24356964374999990, 240.8218750006145399, -3.323476615752268604 ) ) ;
#20234 = CARTESIAN_POINT ( 'NONE',  ( -40.70163769728823411, 213.9548777149308592, -2.149950860017830756 ) ) ;
#20235 = CARTESIAN_POINT ( 'NONE',  ( 26.99999999999999645, 7.347880794884117764E-16, -6.074999999999997513 ) ) ;
#20236 = CARTESIAN_POINT ( 'NONE',  ( 34.39171143809891618, -5.196152422706629359, 168.6468224239574454 ) ) ;
#20237 = CARTESIAN_POINT ( 'NONE',  ( 5.233372021372610483, 28.05231371789855643, -8.152565276336593669 ) ) ;
#20238 = CARTESIAN_POINT ( 'NONE',  ( 20.99999999999999289, 249.8874999999999886, -5.999999999999997335 ) ) ;
#20239 =( BOUNDED_CURVE ( )  B_SPLINE_CURVE ( 2, ( #31660, #11757, #5324, #35060, #26342, #23514, #17084, #378, #34506, #5687, #8546, #28623, #11200, #28440, #4, #37336, #25787, #34321, #31477, #2660, #14237, #11386, #17271, #28994, #23325, #23144, #34876, #28809, #2846, #14418, #25972, #34686, #20492, #20304, #31845, #17457, #32410, #3976, #1319, #9484, #21060, #32788, #26531, #562, #32598, #24080, #6450, #15549, #3785, #9671, #35246, #35813, #15361, #27107, #12887, #12128, #1131, #6638, #752, #12697, #12322, #9109, #21249, #24269, #27289, #9855, #23895, #35625, #29568, #942, #21434, #18023, #20675, #18213, #12516, #35436, #3605, #32974, #29754, #26914, #6823, #32223, #7028, #30137, #18399, #23704, #15172, #29375, #24452, #20871, #18594, #29948, #4168, #9299, #15738, #3413, #6262, #17839, #26719, #14982, #30884, #4907, #10039, #18785, #22361, #19155, #24818, #1504, #36002, #33539, #18965, #22178, #28036, #16488, #7579, #5097, #16676, #4539, #24634, #30703, #10787, #10417, #27667, #2068, #1691, #4350, #30326, #25001, #13642, #28223, #25195, #7392, #33724, #13451, #13266, #36371, #2251, #36747, #13830, #19527, #33910, #7952, #21992, #4723, #16300, #27847, #30519, #21616, #10598, #31074, #10229, #1880, #36557, #33357, #33167, #7213, #7765, #15929, #19345, #27478, #13080, #36184, #21804, #16115, #20264, #23289, #14379, #25562, #17609, #20075, #37300, #22921, #19716, #8690, #22545, #8874, #25937, #37114, #25377, #34094, #6023, #34466, #2620, #31256, #19897, #8509, #31802, #17231, #5282, #25747, #5840, #36926, #3180, #31994, #29140, #22735, #34833, #28582, #11349, #14196, #11162, #31620, #5648, #31439, #8144, #11714, #28769, #34284, #11531, #2809, #17044, #8327, #34645, #17418, #37480, #28958, #23102, #5461, #20452, #2996, #14566, #16862, #26118, #150, #28399, #10974, #2437, #14011, #32367, #26676, #29709, #6985, #3934, #23852, #35583, #6594, #9066, #15125, #21205, #26299, #30094, #26487, #706, #14756, #35390, #11902, #14940, #18168, #20637, #12278, #9439, #20826, #23469, #1089, #17979, #519, #899, #21017, #6406, #23660, #24038, #32551, #35770, #12469, #336, #18554, #35203, #9253, #32181 ),
 .UNSPECIFIED., .F., .F. ) 
 B_SPLINE_CURVE_WITH_KNOTS ( ( 3, 2, 2, 2, 2, 2, 2, 2, 2, 2, 2, 2, 2, 2, 2, 2, 2, 2, 2, 2, 2, 2, 2, 2, 2, 2, 2, 2, 2, 2, 2, 2, 2, 2, 2, 2, 2, 2, 2, 2, 2, 2, 2, 2, 2, 2, 2, 2, 2, 2, 2, 2, 2, 2, 2, 2, 2, 2, 2, 2, 2, 2, 2, 2, 2, 2, 2, 2, 2, 2, 2, 2, 2, 2, 2, 2, 2, 2, 2, 2, 2, 2, 2, 2, 2, 2, 2, 2, 2, 2, 2, 2, 2, 2, 2, 2, 2, 2, 2, 2, 2, 2, 2, 2, 2, 2, 2, 2, 2, 2, 2, 2, 2, 2, 2, 2, 2, 2, 2, 2, 2, 2, 2, 2, 2, 2, 2, 2, 2, 2, 2, 2, 2, 2, 3 ),
 ( 0.000000000000000000, 0.007499808115352593965, 0.01499961623070518793, 0.02249942434605778016, 0.02999923246141037586, 0.03749904057676296809, 0.04499884869211556032, 0.05249865680746815949, 0.05999846492282075172, 0.06749827303817333701, 0.07499808115352593618, 0.08249788926887852147, 0.08999769738423112064, 0.09749750549958371981, 0.1049973136149363190, 0.1124971217302889043, 0.1199969298456415034, 0.1274967379609940887, 0.1349965460763466740, 0.1424963541916992871, 0.1499961623070518724, 0.1574959704224044854, 0.1649957785377570429, 0.1724955866531096560, 0.1799953947684622413, 0.1874952028838148543, 0.1949950109991674396, 0.2024948191145200527, 0.2099946272298726380, 0.2174944353452252233, 0.2249942434605778085, 0.2324940515759304216, 0.2399938596912830069, 0.2474936678066355922, 0.2549934759219881775, 0.2624932840373407905, 0.2699930921526933481, 0.2774929002680460166, 0.2849927083833985741, 0.2924925164987511317, 0.2999923246141037447, 0.3074921327294563578, 0.3149919408448089708, 0.3224917489601615284, 0.3299915570755140859, 0.3374913651908667545, 0.3449911733062193120, 0.3524909814215719250, 0.3599907895369244826, 0.3674905976522771511, 0.3749904057676297087, 0.3824902138829822662, 0.3899900219983348792, 0.3974898301136874368, 0.4049896382290401053, 0.4124894463443926629, 0.4199892544597452759, 0.4274890625750978335, 0.4349888706904504465, 0.4424886788058030596, 0.4499884869211556171, 0.4574882950365082301, 0.4649881031518608432, 0.4724879112672134007, 0.4799877193825660138, 0.4874875274979185713, 0.4949873356132711844, 0.5024871437286237974, 0.5099869518439763549, 0.5174867599593290235, 0.5249865680746815810, 0.5324863761900341386, 0.5399861843053866961, 0.5474859924207393647, 0.5549858005360920332, 0.5624856086514444797, 0.5699854167667971483, 0.5774852248821498168, 0.5849850329975022634, 0.5924848411128549319, 0.5999846492282074895, 0.6074844573435601580, 0.6149842654589127156, 0.6224840735742652731, 0.6299838816896179416, 0.6374836898049703882, 0.6449834979203230567, 0.6524833060356757253, 0.6599831141510281718, 0.6674829222663808403, 0.6749827303817335089, 0.6824825384970860664, 0.6899823466124386240, 0.6974821547277911815, 0.7049819628431438501, 0.7124817709584964076, 0.7199815790738489651, 0.7274813871892016337, 0.7349811953045543023, 0.7424810034199067488, 0.7499808115352594173, 0.7574806196506119749, 0.7649804277659645324, 0.7724802358813172010, 0.7799800439966697585, 0.7874798521120224271, 0.7949796602273748736, 0.8024794683427275421, 0.8099792764580802107, 0.8174790845734326572, 0.8249788926887853258, 0.8324787008041379943, 0.8399785089194905519, 0.8474783170348431094, 0.8549781251501956669, 0.8624779332655483355, 0.8699777413809008930, 0.8774775494962534506, 0.8849773576116061191, 0.8924771657269586767, 0.8999769738423112342, 0.9074767819576639027, 0.9149765900730164603, 0.9224763981883690178, 0.9299762063037216864, 0.9374760144190742439, 0.9449758225344268014, 0.9524756306497793590, 0.9599754387651320275, 0.9674752468804846961, 0.9749750549958371426, 0.9824748631111898112, 0.9899746712265423687, 0.9974744793418949262, 1.000000000000000000 ),
 .UNSPECIFIED. ) 
 CURVE ( )  GEOMETRIC_REPRESENTATION_ITEM ( )  RATIONAL_B_SPLINE_CURVE ( ( 1.000000000000000000, 0.8660254037844387076, 1.000000000000000000, 0.8660254037844387076, 1.000000000000000000, 0.8660254037844387076, 1.000000000000000000, 0.8660254037844387076, 1.000000000000000000, 0.8660254037844387076, 1.000000000000000000, 0.8660254037844387076, 1.000000000000000000, 0.8660254037844387076, 1.000000000000000000, 0.8660254037844387076, 1.000000000000000000, 0.8660254037844387076, 1.000000000000000000, 0.8660254037844387076, 1.000000000000000000, 0.8660254037844387076, 1.000000000000000000, 0.8660254037844387076, 1.000000000000000000, 0.8660254037844387076, 1.000000000000000000, 0.8660254037844387076, 1.000000000000000000, 0.8660254037844387076, 1.000000000000000000, 0.8660254037844387076, 1.000000000000000000, 0.8660254037844387076, 1.000000000000000000, 0.8660254037844387076, 1.000000000000000000, 0.8660254037844387076, 1.000000000000000000, 0.8660254037844387076, 1.000000000000000000, 0.8660254037844387076, 1.000000000000000000, 0.8660254037844387076, 1.000000000000000000, 0.8660254037844387076, 1.000000000000000000, 0.8660254037844387076, 1.000000000000000000, 0.8660254037844387076, 1.000000000000000000, 0.8660254037844387076, 1.000000000000000000, 0.8660254037844387076, 1.000000000000000000, 0.8660254037844387076, 1.000000000000000000, 0.8660254037844387076, 1.000000000000000000, 0.8660254037844387076, 1.000000000000000000, 0.8660254037844387076, 1.000000000000000000, 0.8660254037844387076, 1.000000000000000000, 0.8660254037844387076, 1.000000000000000000, 0.8660254037844387076, 1.000000000000000000, 0.8660254037844387076, 1.000000000000000000, 0.8660254037844387076, 1.000000000000000000, 0.8660254037844387076, 1.000000000000000000, 0.8660254037844387076, 1.000000000000000000, 0.8660254037844387076, 1.000000000000000000, 0.8660254037844387076, 1.000000000000000000, 0.8660254037844387076, 1.000000000000000000, 0.8660254037844387076, 1.000000000000000000, 0.8660254037844387076, 1.000000000000000000, 0.8660254037844387076, 1.000000000000000000, 0.8660254037844387076, 1.000000000000000000, 0.8660254037844387076, 1.000000000000000000, 0.8660254037844387076, 1.000000000000000000, 0.8660254037844387076, 1.000000000000000000, 0.8660254037844387076, 1.000000000000000000, 0.8660254037844387076, 1.000000000000000000, 0.8660254037844387076, 1.000000000000000000, 0.8660254037844387076, 1.000000000000000000, 0.8660254037844387076, 1.000000000000000000, 0.8660254037844387076, 1.000000000000000000, 0.8660254037844387076, 1.000000000000000000, 0.8660254037844387076, 1.000000000000000000, 0.8660254037844387076, 1.000000000000000000, 0.8660254037844387076, 1.000000000000000000, 0.8660254037844387076, 1.000000000000000000, 0.8660254037844387076, 1.000000000000000000, 0.8660254037844387076, 1.000000000000000000, 0.8660254037844387076, 1.000000000000000000, 0.8660254037844387076, 1.000000000000000000, 0.8660254037844387076, 1.000000000000000000, 0.8660254037844387076, 1.000000000000000000, 0.8660254037844387076, 1.000000000000000000, 0.8660254037844387076, 1.000000000000000000, 0.8660254037844387076, 1.000000000000000000, 0.8660254037844387076, 1.000000000000000000, 0.8660254037844387076, 1.000000000000000000, 0.8660254037844387076, 1.000000000000000000, 0.8660254037844387076, 1.000000000000000000, 0.8660254037844387076, 1.000000000000000000, 0.8660254037844387076, 1.000000000000000000, 0.8660254037844387076, 1.000000000000000000, 0.8660254037844387076, 1.000000000000000000, 0.8660254037844387076, 1.000000000000000000, 0.8660254037844387076, 1.000000000000000000, 0.8660254037844387076, 1.000000000000000000, 0.8660254037844387076, 1.000000000000000000, 0.8660254037844387076, 1.000000000000000000, 0.8660254037844387076, 1.000000000000000000, 0.8660254037844387076, 1.000000000000000000, 0.8660254037844387076, 1.000000000000000000, 0.8660254037844387076, 1.000000000000000000, 0.8660254037844387076, 1.000000000000000000, 0.8660254037844387076, 1.000000000000000000, 0.8660254037844387076, 1.000000000000000000, 0.8660254037844387076, 1.000000000000000000, 0.8660254037844387076, 1.000000000000000000, 0.8660254037844387076, 1.000000000000000000, 0.8660254037844387076, 1.000000000000000000, 0.8660254037844387076, 1.000000000000000000, 0.8660254037844387076, 1.000000000000000000, 0.8660254037844387076, 1.000000000000000000, 0.8660254037844387076, 1.000000000000000000, 0.8660254037844387076, 1.000000000000000000, 0.8660254037844387076, 1.000000000000000000, 0.8660254037844387076, 1.000000000000000000, 0.8660254037844387076, 1.000000000000000000, 0.8660254037844387076, 1.000000000000000000, 0.8660254037844387076, 1.000000000000000000, 0.8660254037844387076, 1.000000000000000000, 0.8660254037844387076, 1.000000000000000000, 0.8660254037844387076, 1.000000000000000000, 0.8660254037844387076, 1.000000000000000000, 0.8660254037844387076, 1.000000000000000000, 0.8660254037844387076, 1.000000000000000000, 0.8660254037844387076, 1.000000000000000000, 0.8660254037844387076, 1.000000000000000000, 0.8660254037844387076, 1.000000000000000000, 0.8660254037844387076, 1.000000000000000000, 0.8660254037844387076, 1.000000000000000000, 0.8660254037844387076, 1.000000000000000000, 0.8660254037844387076, 1.000000000000000000, 0.8660254037844387076, 1.000000000000000000, 0.8660254037844387076, 1.000000000000000000, 0.8660254037844387076, 1.000000000000000000, 0.8660254037844387076, 1.000000000000000000, 0.8660254037844387076, 1.000000000000000000, 0.8660254037844387076, 1.000000000000000000, 0.8660254037844387076, 1.000000000000000000, 0.8660254037844387076, 1.000000000000000000, 0.8660254037844387076, 1.000000000000000000, 0.8660254037844387076, 1.000000000000000000, 0.8660254037844387076, 1.000000000000000000, 0.8660254037844387076, 1.000000000000000000, 0.8660254037844387076, 1.000000000000000000, 0.8660254037844387076, 1.000000000000000000, 0.8660254037844387076, 1.000000000000000000, 0.8660254037844387076, 1.000000000000000000, 0.8660254037844387076, 1.000000000000000000, 0.8660254037844387076, 1.000000000000000000, 0.9548848677736607726, 0.9401542295229587953 ) ) 
 REPRESENTATION_ITEM ( '' )  );
#20240 = ADVANCED_FACE ( 'NONE', ( #19009 ), #2110, .F. ) ;
#20241 = APPLICATION_PROTOCOL_DEFINITION ( 'draft international standard', 'automotive_design', 1998, #13203 ) ;
#20242 = CARTESIAN_POINT ( 'NONE',  ( 14.42938872624734259, 195.0000000000000000, 23.12445431839006105 ) ) ;
#20243 = CARTESIAN_POINT ( 'NONE',  ( -13.62178482187498396, 194.9843750006145626, 23.59362340125808188 ) ) ;
#20244 = CARTESIAN_POINT ( 'NONE',  ( -11.08355503943118592, 136.4398137178985735, -10.83675517735179383 ) ) ;
#20245 = PRESENTATION_LAYER_ASSIGNMENT (  '', '', ( #3886 ) ) ;
#20246 = CIRCLE ( 'NONE', #7529, 7.500000000000000000 ) ;
#20247 = ORIENTED_EDGE ( 'NONE', *, *, #15002, .T. ) ;
#20248 = CARTESIAN_POINT ( 'NONE',  ( -2.311890736173176641, 51.52268628210145351, -12.53471296425194836 ) ) ;
#20249 = CARTESIAN_POINT ( 'NONE',  ( 19.39230484541326049, 240.4575961894323370, -5.999999999999997335 ) ) ;
#20250 = CARTESIAN_POINT ( 'NONE',  ( 10.56230152254410903, 0.000000000000000000, -1.800000000000051559 ) ) ;
#20251 = CARTESIAN_POINT ( 'NONE',  ( 30.65222614765988141, 7.209453229046475009, 160.3254497058415495 ) ) ;
#20252 = CARTESIAN_POINT ( 'NONE',  ( 26.99999999999999645, -3.464101615137751278, -2.456249998770948295 ) ) ;
#20253 = CARTESIAN_POINT ( 'NONE',  ( 22.80587116629412492, -3.604726614523238837, -7.659374999385500260 ) ) ;
#20254 = CARTESIAN_POINT ( 'NONE',  ( 13.56230152254410903, 5.196152422706636465, -0.07500000000004725109 ) ) ;
#20255 = CARTESIAN_POINT ( 'NONE',  ( 8.152565276336714462, 71.64768628210146062, -5.233372021372432847 ) ) ;
#20256 = DIRECTION ( 'NONE',  ( 0.9961946980917462113, 0.000000000000000000, -0.08715574274765118534 ) ) ;
#20257 = CARTESIAN_POINT ( 'NONE',  ( 16.56230152254410726, 0.000000000000000000, 0.000000000000000000 ) ) ;
#20258 = ADVANCED_FACE ( 'NONE', ( #28442 ), #19199, .F. ) ;
#20259 =( BOUNDED_CURVE ( )  B_SPLINE_CURVE ( 2, ( #6654, #32993, #3802, #15379, #6842, #29964, #7045 ),
 .UNSPECIFIED., .F., .F. ) 
 B_SPLINE_CURVE_WITH_KNOTS ( ( 3, 2, 2, 3 ),
 ( 0.7391304347826105348, 0.7463768115942048809, 0.7536231884057991159, 0.7608695652173934620 ),
 .UNSPECIFIED. ) 
 CURVE ( )  GEOMETRIC_REPRESENTATION_ITEM ( )  RATIONAL_B_SPLINE_CURVE ( ( 0.9999999999999651390, 0.8660254037844735686, 1.000000000000000000, 0.8660254037844387076, 1.000000000000000000, 0.8660254037843997388, 1.000000000000039080 ) ) 
 REPRESENTATION_ITEM ( '' )  );
#20260 = CARTESIAN_POINT ( 'NONE',  ( 0.1745138560725515708, 97.81018628210144072, -12.50000000000000355 ) ) ;
#20261 = FACE_OUTER_BOUND ( 'NONE', #24353, .T. ) ;
#20262 = CARTESIAN_POINT ( 'NONE',  ( -7.234628195640354420, 195.1424038105676573, 26.99999999999996803 ) ) ;
#20263 = ORIENTED_EDGE ( 'NONE', *, *, #9236, .T. ) ;
#20264 = CARTESIAN_POINT ( 'NONE',  ( 34.02033052368495447, -5.407089921784855591, 163.0045950240894967 ) ) ;
#20265 = CARTESIAN_POINT ( 'NONE',  ( 18.12178482187500350, -4.985214923628407568, -7.715624999385467753 ) ) ;
#20266 = CARTESIAN_POINT ( 'NONE',  ( 27.24356964375000345, 196.4843750006145626, -3.336375036156643733E-15 ) ) ;
#20267 = CARTESIAN_POINT ( 'NONE',  ( 37.52407102436108488, 7.646167579472024665E-16, 167.2340683412427040 ) ) ;
#20268 = CARTESIAN_POINT ( 'NONE',  ( 28.12366095802104127, -5.196152422706638241, 165.8449570743377990 ) ) ;
#20269 = CARTESIAN_POINT ( 'NONE',  ( 10.56230152254410548, 0.000000000000000000, -4.050000000000054001 ) ) ;
#20270 = CARTESIAN_POINT ( 'NONE',  ( 18.00000000000000000, 247.2249999999999943, -5.196152422706630247 ) ) ;
#20271 = CARTESIAN_POINT ( 'NONE',  ( -1.926257025242585782E-15, 197.8906250006145342, -31.45816453501076637 ) ) ;
#20272 = EDGE_CURVE ( 'NONE', #25162, #5600, #16718, .T. ) ;
#20273 = CARTESIAN_POINT ( 'NONE',  ( -6.932735513424201912, 124.6523137178985650, 10.69584247140429412 ) ) ;
#20274 = CARTESIAN_POINT ( 'NONE',  ( -12.46528703574805874, 123.3976862821014606, -2.660918448318280838 ) ) ;
#20276 = ORIENTED_EDGE ( 'NONE', *, *, #14224, .T. ) ;
#20275 = ORIENTED_EDGE ( 'NONE', *, *, #25685, .T. ) ;
#20277 = CARTESIAN_POINT ( 'NONE',  ( -1.926257025242585782E-15, 197.4406250006145740, -31.45816453501075927 ) ) ;
#20278 = CARTESIAN_POINT ( 'NONE',  ( 18.12178482187499640, 242.0218750006145001, -4.985214923628404904 ) ) ;
#20279 = LINE ( 'NONE', #31818, #26789 ) ;
#20280 = CARTESIAN_POINT ( 'NONE',  ( -0.1745138560722442889, 91.58981371789856496, -15.50000000000000533 ) ) ;
#20281 = CARTESIAN_POINT ( 'NONE',  ( 15.24356964375000167, -3.323476615752272600, -3.365624999385478322 ) ) ;
#20282 = CARTESIAN_POINT ( 'NONE',  ( 15.24356964375000167, 247.6468750006145569, 3.323476615752272600 ) ) ;
#20283 = CARTESIAN_POINT ( 'NONE',  ( -13.49999999999998401, 196.5875000012290457, 23.38268590217985476 ) ) ;
#20284 = CARTESIAN_POINT ( 'NONE',  ( -6.594114490232462877, 69.73981371789855643, 6.840914352311949109 ) ) ;
#20285 = CARTESIAN_POINT ( 'NONE',  ( 10.31873187879411446, -3.604726614523240613, -2.803124999385555149 ) ) ;
#20286 = CARTESIAN_POINT ( 'NONE',  ( 15.24356964375000167, 243.0343750006144887, 3.323476615752272600 ) ) ;
#20287 = CARTESIAN_POINT ( 'NONE',  ( -4.944772684328424539, 54.21481371789854364, -11.48171059495408031 ) ) ;
#20288 = DIRECTION ( 'NONE',  ( 0.000000000000000000, 0.000000000000000000, -1.000000000000000000 ) ) ;
#20289 = EDGE_CURVE ( 'NONE', #29417, #20367, #16363, .T. ) ;
#20290 = CARTESIAN_POINT ( 'NONE',  ( -12.53471296425194836, 95.22268628210146346, 2.311890736173176641 ) ) ;
#20291 = CARTESIAN_POINT ( 'NONE',  ( 10.56230152254411436, 3.464101615137752166, -3.974999998771034715 ) ) ;
#20292 = CARTESIAN_POINT ( 'NONE',  ( -37.33705436395490551, 205.3262412349647263, -4.842901733360204020 ) ) ;
#20293 = CARTESIAN_POINT ( 'NONE',  ( 22.60769515458672885, 240.0236538117966916, -5.999999999999998224 ) ) ;
#20294 = CARTESIAN_POINT ( 'NONE',  ( -26.99999999999999645, 198.8000000012290513, 15.58845726811991561 ) ) ;
#20295 = CARTESIAN_POINT ( 'NONE',  ( -8.927990412390661490, 94.07268628210144357, 13.04141134922759804 ) ) ;
#20296 = CARTESIAN_POINT ( 'NONE',  ( 12.46528703574805874, 8.397686282101441080, 2.660918448318279950 ) ) ;
#20297 = CARTESIAN_POINT ( 'NONE',  ( 20.99999999999999645, -6.928203230275506996, -0.3375000000000047962 ) ) ;
#20298 = EDGE_CURVE ( 'NONE', #37055, #529, #618, .T. ) ;
#20299 = CARTESIAN_POINT ( 'NONE',  ( -9.000000000000024869, 210.0000000000000000, 0.000000000000000000 ) ) ;
#20300 = CARTESIAN_POINT ( 'NONE',  ( 8.843639120294328748, 136.3351862821014606, -3.474262827703334722 ) ) ;
#20301 = CARTESIAN_POINT ( 'NONE',  ( 8.843639120294245259, 85.26481371789857633, 3.474262827703527901 ) ) ;
#20302 = CARTESIAN_POINT ( 'NONE',  ( 23.87821517812499650, 242.8468750006145171, -4.985214923628404904 ) ) ;
#20303 = ORIENTED_EDGE ( 'NONE', *, *, #14801, .T. ) ;
#20304 = CARTESIAN_POINT ( 'NONE',  ( 31.33857762179763995, -7.209453229046475009, 168.1704829533140071 ) ) ;
#20305 = CARTESIAN_POINT ( 'NONE',  ( 3.796722387233379514, 61.58518628210146062, -8.710071997420127943 ) ) ;
#20306 = CARTESIAN_POINT ( 'NONE',  ( 26.75643035624999655, 7.049594010296217766E-16, -0.8156249993854780556 ) ) ;
#20307 = ADVANCED_FACE ( 'NONE', ( #6063 ), #20494, .T. ) ;
#20308 = CARTESIAN_POINT ( 'NONE',  ( -27.24356964374999635, 194.8906250006145342, 15.72908226750539384 ) ) ;
#20309 = CARTESIAN_POINT ( 'NONE',  ( 15.00000000000000000, 246.8687500012290457, -3.464101615137752610 ) ) ;
#20310 = CARTESIAN_POINT ( 'NONE',  ( 0.000000000000000000, 141.0000000000000000, 0.000000000000000000 ) ) ;
#20311 = CARTESIAN_POINT ( 'NONE',  ( 22.60769515458672529, 246.2674038105676004, -6.000000000000004441 ) ) ;
#20312 = CARTESIAN_POINT ( 'NONE',  ( 10.56230152254410903, 0.000000000000000000, -5.737499998771017573 ) ) ;
#20313 = CARTESIAN_POINT ( 'NONE',  ( -3.796722387233185003, 45.01481371789854791, -8.710071997420207879 ) ) ;
#20314 = CARTESIAN_POINT ( 'NONE',  ( 20.00000000000024869, -5.916079783099657874, -7.999999999999998224 ) ) ;
#20315 = ORIENTED_EDGE ( 'NONE', *, *, #13660, .F. ) ;
#20316 = ORIENTED_EDGE ( 'NONE', *, *, #16671, .F. ) ;
#20317 = CARTESIAN_POINT ( 'NONE',  ( 24.00000000000000000, 239.8562500012290286, 5.196152422706629359 ) ) ;
#20318 = CARTESIAN_POINT ( 'NONE',  ( 2.311890736173452421, 36.67731371789854933, -12.53471296425189152 ) ) ;
#20319 = CARTESIAN_POINT ( 'NONE',  ( 16.56230152254411436, -7.209453229046482114, -8.634374999385517668 ) ) ;
#20320 = CARTESIAN_POINT ( 'NONE',  ( 23.87821517812500005, -4.985214923628404016, -8.203124999385469351 ) ) ;
#20321 = CARTESIAN_POINT ( 'NONE',  ( 10.49813415416005213, 10.22731371789853227, -7.228626920338837358 ) ) ;
#20322 = EDGE_CURVE ( 'NONE', #6180, #19808, #5503, .T. ) ;
#20323 = VERTEX_POINT ( 'NONE', #6 ) ;
#20324 = CARTESIAN_POINT ( 'NONE',  ( 19.68408634441910721, 5.407089921784862696, -2.596874999385518024 ) ) ;
#20325 = AXIS2_PLACEMENT_3D ( 'NONE', #17561, #3139, #106 ) ;
#20326 = CARTESIAN_POINT ( 'NONE',  ( 15.00000000000000000, 245.9687500012290684, -3.464101615137752610 ) ) ;
#20327 = CARTESIAN_POINT ( 'NONE',  ( 31.27484498491342180, 7.209453229046482114, 167.4420155803344699 ) ) ;
#20328 = CARTESIAN_POINT ( 'NONE',  ( -65.63169563604516554, 210.1155267958018271, 8.500000000000003553 ) ) ;
#20329 = CARTESIAN_POINT ( 'NONE',  ( 18.12178482187500350, 248.0218750006145001, 4.985214923628407568 ) ) ;
#20330 =( LENGTH_UNIT ( ) NAMED_UNIT ( * ) SI_UNIT ( .MILLI., .METRE. ) );
#20331 = CARTESIAN_POINT ( 'NONE',  ( -20.80563922340697403, 195.0000000000000284, -17.20829382900668492 ) ) ;
#20332 = ADVANCED_FACE ( 'NONE', ( #23327 ), #17459, .F. ) ;
#20333 = CARTESIAN_POINT ( 'NONE',  ( -54.15252896937849414, 207.6499508600178387, -3.839350919129087547 ) ) ;
#20334 = CARTESIAN_POINT ( 'NONE',  ( -45.84747103062156981, 213.3500491399821328, -5.571401726697985168 ) ) ;
#20335 = CARTESIAN_POINT ( 'NONE',  ( 37.53224187524366329, 3.604726614523238837, 167.3274615941888044 ) ) ;
#20336 = ORIENTED_EDGE ( 'NONE', *, *, #26308, .F. ) ;
#20337 = CARTESIAN_POINT ( 'NONE',  ( -7.234628195640302017, 197.9549038117966973, 27.00000000000000711 ) ) ;
#20338 = CARTESIAN_POINT ( 'NONE',  ( 26.99999999999940314, 3.464101615138096335, -1.481249998770923781 ) ) ;
#20339 = CARTESIAN_POINT ( 'NONE',  ( -14.25334919248795096, 24.31481371789855217, 6.092822981423662299 ) ) ;
#20340 = CARTESIAN_POINT ( 'NONE',  ( -62.47247103062156981, 205.6499508600178956, 7.303452534266880569 ) ) ;
#20341 = CARTESIAN_POINT ( 'NONE',  ( -8.152565276336710909, 140.6476862821014322, 5.233372021372435512 ) ) ;
#20342 = CARTESIAN_POINT ( 'NONE',  ( -2.311890736173176641, 51.52268628210145351, -12.53471296425194836 ) ) ;
#20343 = CARTESIAN_POINT ( 'NONE',  ( 10.56230152254410726, 3.464101615137757051, -5.437500000000041744 ) ) ;
#20344 = ORIENTED_EDGE ( 'NONE', *, *, #27910, .T. ) ;
#20345 = CARTESIAN_POINT ( 'NONE',  ( -42.48288769728824121, 203.5309553116391896, -1.857196546604028997 ) ) ;
#20346 = ADVANCED_FACE ( 'NONE', ( #17650 ), #5936, .T. ) ;
#20347 = DIRECTION ( 'NONE',  ( -6.123233995736766036E-17, 1.000000000000000000, 0.000000000000000000 ) ) ;
#20348 = CARTESIAN_POINT ( 'NONE',  ( 27.24356964374999635, 196.5218750006145569, -15.72908226750539029 ) ) ;
#20349 = CARTESIAN_POINT ( 'NONE',  ( 21.00000000000001066, 247.4124999999999943, 5.999999999999998224 ) ) ;
#20350 = DIRECTION ( 'NONE',  ( 0.08715574274765150453, 0.000000000000000000, 0.9961946980917461003 ) ) ;
#20351 = FACE_BOUND ( 'NONE', #15899, .T. ) ;
#20352 = AXIS2_PLACEMENT_3D ( 'NONE', #14796, #26158, #17648 ) ;
#20353 = CARTESIAN_POINT ( 'NONE',  ( 23.87821517812499650, 245.2093750006145569, -4.985214923628404904 ) ) ;
#20354 = CARTESIAN_POINT ( 'NONE',  ( -3.796722387233185003, 100.2148137178985650, -8.710071997420207879 ) ) ;
#20355 = CARTESIAN_POINT ( 'NONE',  ( 20.00041297495057435, 239.8598985277378972, -5.668978411116884608 ) ) ;
#20356 = ORIENTED_EDGE ( 'NONE', *, *, #37261, .F. ) ;
#20357 = CARTESIAN_POINT ( 'NONE',  ( -55.94122103062156270, 208.3738570449993404, -6.530955311639226935 ) ) ;
#20358 = CARTESIAN_POINT ( 'NONE',  ( 27.00000000000000355, 197.1875000012290400, -3.306546357697854128E-15 ) ) ;
#20359 = CARTESIAN_POINT ( 'NONE',  ( 26.99999999999999645, 245.8187500012290627, -3.464101615137755275 ) ) ;
#20360 = ORIENTED_EDGE ( 'NONE', *, *, #32395, .T. ) ;
#20361 = CARTESIAN_POINT ( 'NONE',  ( 8.715434833792128799, 101.9398137178985593, -8.962234695871567070 ) ) ;
#20362 = CARTESIAN_POINT ( 'NONE',  ( 10.31873187879411091, 3.604726614523240613, -0.6843749993854860714 ) ) ;
#20363 = CARTESIAN_POINT ( 'NONE',  ( 30.61300606342344111, 7.209453229046475009, 159.8771620917002565 ) ) ;
#20364 = CARTESIAN_POINT ( 'NONE',  ( 23.87821517812500005, -4.985214923628404016, -1.453124999385491112 ) ) ;
#20365 = CARTESIAN_POINT ( 'NONE',  ( 10.49813415416005213, 65.42731371789855643, -7.228626920338837358 ) ) ;
#20366 = CARTESIAN_POINT ( 'NONE',  ( -13.62178482187498396, 199.4843750006145626, 23.59362340125808188 ) ) ;
#20367 = VERTEX_POINT ( 'NONE', #30938 ) ;
#20368 = ORIENTED_EDGE ( 'NONE', *, *, #30812, .F. ) ;
#20369 = VERTEX_POINT ( 'NONE', #28451 ) ;
#20370 = CARTESIAN_POINT ( 'NONE',  ( 15.24356964374999990, 0.000000000000000000, -5.090624999385479299 ) ) ;
#20371 = CARTESIAN_POINT ( 'NONE',  ( 26.75643035624999655, 245.8843750006145399, 3.323476615752267715 ) ) ;
#20372 = AXIS2_PLACEMENT_3D ( 'NONE', #22211, #13481, #25035 ) ;
#20373 = CARTESIAN_POINT ( 'NONE',  ( -8.715434833791929847, 41.46018628210144641, -8.962234695871762469 ) ) ;
#20374 = ADVANCED_FACE ( 'NONE', ( #4956 ), #4777, .F. ) ;
#20375 = ADVANCED_FACE ( 'NONE', ( #16538 ), #36420, .F. ) ;
#20376 = CARTESIAN_POINT ( 'NONE',  ( -52.17336230271183695, 215.6869285224997270, 3.149950860017831200 ) ) ;
#20377 = CARTESIAN_POINT ( 'NONE',  ( -70.65404437008253069, 216.5466800865261234, 7.499999999999999112 ) ) ;
#20378 = CARTESIAN_POINT ( 'NONE',  ( -32.77752896937849414, 212.3500491399821613, 3.839350919129088435 ) ) ;
#20379 = CARTESIAN_POINT ( 'NONE',  ( 24.74941270219456158, -3.464101615137757051, 161.6982627647491881 ) ) ;
#20380 = CARTESIAN_POINT ( 'NONE',  ( 4.622313124798831829, 110.5648137178985593, -11.61527771782809282 ) ) ;
#20381 = CARTESIAN_POINT ( 'NONE',  ( -53.76413769728823411, 212.1499508600178387, 3.954877714930865817 ) ) ;
#20383 = EDGE_CURVE ( 'NONE', #36284, #27062, #15139, .T. ) ;
#20382 = CARTESIAN_POINT ( 'NONE',  ( -48.61830436395490551, 209.8844732041983150, 8.500000000000003553 ) ) ;
#20384 = CARTESIAN_POINT ( 'NONE',  ( 26.75643035624999655, -3.323476615752267271, -4.565624999385477167 ) ) ;
#20385 = CARTESIAN_POINT ( 'NONE',  ( 22.56230152254411792, 7.347880794884125653E-16, -5.175000000000040679 ) ) ;
#20386 = CARTESIAN_POINT ( 'NONE',  ( -0.1745138560722442889, 82.38981371789856212, -15.50000000000000533 ) ) ;
#20387 = CARTESIAN_POINT ( 'NONE',  ( -59.49627896937850835, 201.4690446883607251, -2.162041339862721845 ) ) ;
#20388 = VERTEX_POINT ( 'NONE', #20685 ) ;
#20389 = CARTESIAN_POINT ( 'NONE',  ( 24.00000000000000000, 240.6999999999999886, 5.196152422706629359 ) ) ;
#20390 = CARTESIAN_POINT ( 'NONE',  ( -4.944772684328673229, 112.1851862821014549, 11.48171059495397728 ) ) ;
#20391 = CARTESIAN_POINT ( 'NONE',  ( 15.53471296425195369, 53.82268628210144357, -2.908627838312120684 ) ) ;
#20392 = CARTESIAN_POINT ( 'NONE',  ( 18.00000000000000000, 243.1750000000000114, -5.196152422706630247 ) ) ;
#20393 = CARTESIAN_POINT ( 'NONE',  ( 36.93250142046140638, -3.604726614523238837, 160.4723968279450048 ) ) ;
#20394 = CARTESIAN_POINT ( 'NONE',  ( -15.50000000000000533, 67.91018628210144925, -0.1745138560725808530 ) ) ;
#20395 = CARTESIAN_POINT ( 'NONE',  ( 13.62178482187499640, 199.6531250006145228, -23.59362340125807123 ) ) ;
#20396 = CARTESIAN_POINT ( 'NONE',  ( 10.31873187879411091, 3.604726614523236616, -7.828124999385535965 ) ) ;
#20397 = CARTESIAN_POINT ( 'NONE',  ( 0.000000000000000000, 210.0000000000000284, -27.00000000000000000 ) ) ;
#20398 = CARTESIAN_POINT ( 'NONE',  ( -52.18080436395490551, 203.5000000000000000, -0.1155267958017335561 ) ) ;
#20399 = CARTESIAN_POINT ( 'NONE',  ( 10.53357014895476951, 1.237016744030756454, -9.999999999999998224 ) ) ;
#20400 = CARTESIAN_POINT ( 'NONE',  ( -2.311890736173176641, 33.12268628210144072, -12.53471296425194836 ) ) ;
#20401 = CARTESIAN_POINT ( 'NONE',  ( 27.00000000000000355, 196.1750000000000114, -3.306546357697854128E-15 ) ) ;
#20402 = CARTESIAN_POINT ( 'NONE',  ( 15.00000000000000000, 0.000000000000000000, -2.643749998770955401 ) ) ;
#20403 = CARTESIAN_POINT ( 'NONE',  ( 6.594114490232313663, 9.260186282101427580, 6.840914352312096547 ) ) ;
#20404 = CARTESIAN_POINT ( 'NONE',  ( 26.75643035624999655, 247.3843750006145399, -7.049594010296217766E-16 ) ) ;
#20405 = ORIENTED_EDGE ( 'NONE', *, *, #31634, .T. ) ;
#20406 = CARTESIAN_POINT ( 'NONE',  ( 26.99999999999999645, 7.347880794884117764E-16, -5.624999999999991118 ) ) ;
#20407 = CARTESIAN_POINT ( 'NONE',  ( -29.00000000000002487, 216.0000000000000000, 7.347880794884114806E-16 ) ) ;
#20408 = CARTESIAN_POINT ( 'NONE',  ( 16.56230152254410726, 0.000000000000000000, -10.00000000000000000 ) ) ;
#20409 = CARTESIAN_POINT ( 'NONE',  ( 22.80587116629410360, 3.604726614523238837, -3.478124999385532767 ) ) ;
#20410 = CARTESIAN_POINT ( 'NONE',  ( 24.99456971211191814, -3.604726614523240613, 167.2950684582310146 ) ) ;
#20411 = CARTESIAN_POINT ( 'NONE',  ( 26.99999999999999645, 241.1875000000000284, 3.464101615137751278 ) ) ;
#20412 = CARTESIAN_POINT ( 'NONE',  ( 26.99999999999999645, 7.347880794884117764E-16, -1.068749998770962550 ) ) ;
#20413 = CARTESIAN_POINT ( 'NONE',  ( -10.69584247140444866, 67.04768628210145209, 6.932735513423972762 ) ) ;
#20414 = VERTEX_POINT ( 'NONE', #14990 ) ;
#20415 = ORIENTED_EDGE ( 'NONE', *, *, #36569, .T. ) ;
#20416 = FACE_BOUND ( 'NONE', #34613, .T. ) ;
#20417 = CARTESIAN_POINT ( 'NONE',  ( 27.00000000000001066, 195.8000000012290513, 15.58845726811988897 ) ) ;
#20418 = FACE_OUTER_BOUND ( 'NONE', #30267, .T. ) ;
#20419 = CARTESIAN_POINT ( 'NONE',  ( 21.00000000000000000, -6.646953231504538984, -7.228124999385454608 ) ) ;
#20420 = AXIS2_PLACEMENT_3D ( 'NONE', #8220, #29177, #3219 ) ;
#20421 = CARTESIAN_POINT ( 'NONE',  ( -5.770363421894122880, 32.36481371789854933, 14.38691631536194393 ) ) ;
#20422 = CARTESIAN_POINT ( 'NONE',  ( 28.04522078954815356, -5.196152422706638241, 164.9483818460552413 ) ) ;
#20423 = CARTESIAN_POINT ( 'NONE',  ( 15.24356964375000167, 240.4468750006145399, 3.323476615752272600 ) ) ;
#20424 = CARTESIAN_POINT ( 'NONE',  ( -38.92038769728823411, 208.6787018382581778, 4.469044688360752637 ) ) ;
#20425 = AXIS2_PLACEMENT_3D ( 'NONE', #36632, #28107, #13901 ) ;
#20426 = CARTESIAN_POINT ( 'NONE',  ( -20.68320042480035426, 195.0000000000000000, -17.35526491262920956 ) ) ;
#20427 = CARTESIAN_POINT ( 'NONE',  ( 37.31166038496037629, 3.464101615137755275, 167.6008518709672614 ) ) ;
#20428 = CARTESIAN_POINT ( 'NONE',  ( -8.152565276336593669, 25.75231371789854506, -5.233372021372610483 ) ) ;
#20429 = CARTESIAN_POINT ( 'NONE',  ( -53.76413769728823411, 213.1499508600178672, 5.686928522499718142 ) ) ;
#20430 = CARTESIAN_POINT ( 'NONE',  ( -44.65252896937850835, 205.6499508600178103, -7.303452534266820173 ) ) ;
#20431 =( NAMED_UNIT ( * ) PLANE_ANGLE_UNIT ( ) SI_UNIT ( $, .RADIAN. ) );
#20432 = PRODUCT_RELATED_PRODUCT_CATEGORY ( 'part', '', ( #16821 ) ) ;
#20433 = CARTESIAN_POINT ( 'NONE',  ( 25.75952191513118095, 195.0000000000000000, 8.586198610466265535 ) ) ;
#20434 = CARTESIAN_POINT ( 'NONE',  ( 27.24356964375000345, 196.9343750006145228, -3.336375036156643733E-15 ) ) ;
#20435 = CARTESIAN_POINT ( 'NONE',  ( -15.53471296425188442, 135.5773137178985905, -2.908627838312459080 ) ) ;
#20436 = ORIENTED_EDGE ( 'NONE', *, *, #18646, .T. ) ;
#20437 = CARTESIAN_POINT ( 'NONE',  ( -4.944772684328673229, 38.58518628210144641, 11.48171059495397728 ) ) ;
#20438 = CARTESIAN_POINT ( 'NONE',  ( 10.56230152254411259, 0.000000000000000000, -10.23749999877102113 ) ) ;
#20439 = ADVANCED_FACE ( 'NONE', ( #14807 ), #34886, .T. ) ;
#20440 = LINE ( 'NONE', #14553, #1734 ) ;
#20441 = CARTESIAN_POINT ( 'NONE',  ( 28.24664800560418243, 5.407089921784862696, 168.6480295846443482 ) ) ;
#20442 = CARTESIAN_POINT ( 'NONE',  ( 26.99999999999999645, 3.464101615137755275, -1.481249998770931109 ) ) ;
#20443 = CARTESIAN_POINT ( 'NONE',  ( 19.68408634441911786, -5.407089921784861808, -9.496874999385534366 ) ) ;
#20444 = CARTESIAN_POINT ( 'NONE',  ( -69.20163769728823411, 215.6869285224996986, -3.149950860017881382 ) ) ;
#20445 = CARTESIAN_POINT ( 'NONE',  ( 6.840914352312096547, 52.96018628210144641, -6.594114490232313663 ) ) ;
#20446 = CARTESIAN_POINT ( 'NONE',  ( 20.99999999999999645, 185.0294372515228645, 0.000000000000000000 ) ) ;
#20447 = CARTESIAN_POINT ( 'NONE',  ( 10.49999999999999645, 237.0000000000000000, 5.000000000000000000 ) ) ;
#20448 = CARTESIAN_POINT ( 'NONE',  ( 7.228626920339068285, 98.67268628210145209, -10.49813415415989581 ) ) ;
#20449 = CARTESIAN_POINT ( 'NONE',  ( 16.56230152254410726, 0.000000000000000000, -10.00000000000000000 ) ) ;
#20450 = CARTESIAN_POINT ( 'NONE',  ( -13.49999999999998401, 195.1250000000000284, 23.38268590217985476 ) ) ;
#20451 = ORIENTED_EDGE ( 'NONE', *, *, #28157, .T. ) ;
#20452 = CARTESIAN_POINT ( 'NONE',  ( 27.62402916835064559, 5.407089921784856479, 161.5314637101514279 ) ) ;
#20453 = CARTESIAN_POINT ( 'NONE',  ( 21.00000000000000000, 6.646953231504538984, -8.353124999385492799 ) ) ;
#20454 = CARTESIAN_POINT ( 'NONE',  ( 13.62178482187499640, 196.5593750006145513, -23.59362340125807123 ) ) ;
#20455 = CARTESIAN_POINT ( 'NONE',  ( 34.25074851857407765, -5.407089921784861808, 165.6382847571695436 ) ) ;
#20456 = CARTESIAN_POINT ( 'NONE',  ( 25.04683167421379508, 3.464101615137757051, 165.0977771707628960 ) ) ;
#20457 = FACE_OUTER_BOUND ( 'NONE', #15834, .T. ) ;
#20458 = CARTESIAN_POINT ( 'NONE',  ( 26.99999999999999645, 249.3625000000000114, -3.464101615137755275 ) ) ;
#20459 = CARTESIAN_POINT ( 'NONE',  ( -13.62178482187498396, 197.6281250006145171, 23.59362340125808188 ) ) ;
#20460 = CARTESIAN_POINT ( 'NONE',  ( 11.61527771782809637, 112.8648137178985564, 4.622313124798827388 ) ) ;
#20461 = CARTESIAN_POINT ( 'NONE',  ( 10.69584247140445221, 117.6476862821014606, -6.932735513423970097 ) ) ;
#20462 = CIRCLE ( 'NONE', #4105, 4.000000000000000888 ) ;
#20464 = ORIENTED_EDGE ( 'NONE', *, *, #10991, .T. ) ;
#20463 = VERTEX_POINT ( 'NONE', #8555 ) ;
#20465 = CARTESIAN_POINT ( 'NONE',  ( 13.62178482187499640, 198.7531250006145456, -23.59362340125807123 ) ) ;
#20466 = CARTESIAN_POINT ( 'NONE',  ( 15.24356964375000167, 242.5843750006145285, 3.323476615752272600 ) ) ;
#20467 = CARTESIAN_POINT ( 'NONE',  ( -14.25334919248795096, 88.71481371789855075, 6.092822981423662299 ) ) ;
#20468 =( BOUNDED_CURVE ( )  B_SPLINE_CURVE ( 2, ( #13409, #24958, #36145, #30844, #4868, #2023, #21764, #13601, #36706 ),
 .UNSPECIFIED., .F., .F. ) 
 B_SPLINE_CURVE_WITH_KNOTS ( ( 3, 2, 2, 2, 3 ),
 ( 0.1875000000000000000, 0.1944444444444444475, 0.2083333333333333426, 0.2222222222222222099, 0.2291666666666666574 ),
 .UNSPECIFIED. ) 
 CURVE ( )  GEOMETRIC_REPRESENTATION_ITEM ( )  RATIONAL_B_SPLINE_CURVE ( ( 0.9330127018922194093, 0.9330127018922194093, 1.000000000000000000, 0.8660254037844387076, 1.000000000000000000, 0.8660254037844387076, 1.000000000000000000, 0.9330127018922194093, 0.9330127018922194093 ) ) 
 REPRESENTATION_ITEM ( '' )  );
#20469 = CARTESIAN_POINT ( 'NONE',  ( 15.24356964374999990, 0.000000000000000000, -5.203124999385494220 ) ) ;
#20470 = CARTESIAN_POINT ( 'NONE',  ( 26.75643035624999655, 246.4843750006145342, -7.049594010296217766E-16 ) ) ;
#20471 = CARTESIAN_POINT ( 'NONE',  ( -26.99999999999998934, 196.5500000012290229, 15.58845726811991561 ) ) ;
#20472 = CARTESIAN_POINT ( 'NONE',  ( 8.152565276336593669, 67.15231371789852233, 5.233372021372610483 ) ) ;
#20473 = CARTESIAN_POINT ( 'NONE',  ( 22.80587116629410716, 7.646167579472015790E-16, -4.865624999385531169 ) ) ;
#20474 = CARTESIAN_POINT ( 'NONE',  ( 20.99999999999999645, 242.8843750006145399, -6.646953231504538984 ) ) ;
#20475 = CARTESIAN_POINT ( 'NONE',  ( -2.660918448318004614, 54.50231371789855217, -12.46528703574811558 ) ) ;
#20476 = DIRECTION ( 'NONE',  ( -0.000000000000000000, -0.000000000000000000, 1.000000000000000000 ) ) ;
#20477 = CARTESIAN_POINT ( 'NONE',  ( -11.61527771782819940, 104.1351862821014578, 4.622313124798574258 ) ) ;
#20478 = CARTESIAN_POINT ( 'NONE',  ( 10.56230152254410903, 3.464101615137752166, -2.624999998770982668 ) ) ;
#20479 =( BOUNDED_CURVE ( )  B_SPLINE_CURVE ( 2, ( #29279, #17555, #26250, #23238, #34786, #9014, #12038 ),
 .UNSPECIFIED., .F., .F. ) 
 B_SPLINE_CURVE_WITH_KNOTS ( ( 3, 2, 2, 3 ),
 ( 0.6956521739130446802, 0.7028985507246381381, 0.7101449275362315960, 0.7173913043478249429 ),
 .UNSPECIFIED. ) 
 CURVE ( )  GEOMETRIC_REPRESENTATION_ITEM ( )  RATIONAL_B_SPLINE_CURVE ( ( 0.9999999999999774625, 0.8660254037844612451, 1.000000000000000000, 0.8660254037844387076, 1.000000000000000000, 0.8660254037844592467, 0.9999999999999794609 ) ) 
 REPRESENTATION_ITEM ( '' )  );
#20480 = CARTESIAN_POINT ( 'NONE',  ( -35.75372103062156981, 216.5309553116391612, -1.626142955000564383 ) ) ;
#20481 = CARTESIAN_POINT ( 'NONE',  ( 25.00000000000004263, 0.000000000000000000, 49.82535622836640954 ) ) ;
#20482 = VECTOR ( 'NONE', #13269, 1000.000000000000000 ) ;
#20483 = CARTESIAN_POINT ( 'NONE',  ( 14.38691631536207538, 108.7351862821014663, -5.770363421893813793 ) ) ;
#20484 = CARTESIAN_POINT ( 'NONE',  ( -7.228626920339070061, 11.27268628210142865, 10.49813415415989404 ) ) ;
#20485 = CARTESIAN_POINT ( 'NONE',  ( 13.56230152254410726, 5.196152422706636465, -8.175000000000043343 ) ) ;
#20486 = CARTESIAN_POINT ( 'NONE',  ( 20.99999999999999289, 241.3937500012289945, -5.999999999999997335 ) ) ;
#20487 = CARTESIAN_POINT ( 'NONE',  ( 0.1745138560725194299, 125.4101862821014635, -9.500000000000005329 ) ) ;
#20488 = FACE_OUTER_BOUND ( 'NONE', #6637, .T. ) ;
#20489 = CARTESIAN_POINT ( 'NONE',  ( -27.24356964374999635, 194.9468750006145399, 15.72908226750539384 ) ) ;
#20490 = CARTESIAN_POINT ( 'NONE',  ( 15.24356964374999990, 241.6093750006145058, -3.323476615752268604 ) ) ;
#20491 = EDGE_LOOP ( 'NONE', ( #26396, #1537, #24372, #14052 ) ) ;
#20492 = CARTESIAN_POINT ( 'NONE',  ( 34.45175145028584041, -5.407089921784855591, 167.9357587796436064 ) ) ;
#20493 = CARTESIAN_POINT ( 'NONE',  ( -3.796722387233375073, 66.18518628210145494, 8.710071997420127943 ) ) ;
#20494 = CYLINDRICAL_SURFACE ( 'NONE', #34529, 5.999999999999994671 ) ;
#20495 = CARTESIAN_POINT ( 'NONE',  ( 20.99999999999999645, 0.000000000000000000, -8.000000000000000000 ) ) ;
#20496 = CARTESIAN_POINT ( 'NONE',  ( 26.99999999999981171, 3.464101615137862300, -3.787500000000012523 ) ) ;
#20497 = CARTESIAN_POINT ( 'NONE',  ( 20.99999999999995381, 241.1687500012290570, 5.999999999999998224 ) ) ;
#20498 = DIRECTION ( 'NONE',  ( 1.000000000000000000, 0.000000000000000000, -0.000000000000000000 ) ) ;
#20499 = ADVANCED_FACE ( 'NONE', ( #32040, #31855 ), #23154, .F. ) ;
#20500 = CARTESIAN_POINT ( 'NONE',  ( 37.22341519532091070, 3.464101615137966217, 166.5922047379251012 ) ) ;
#20501 = CARTESIAN_POINT ( 'NONE',  ( 8.843639120294245259, 39.26481371789855501, 3.474262827703527901 ) ) ;
#20502 = CARTESIAN_POINT ( 'NONE',  ( 5.778771075727756162E-15, 199.5218750006145569, 31.45816453501076637 ) ) ;
#20503 = VECTOR ( 'NONE', #29840, 1000.000000000000000 ) ;
#20504 = VERTEX_POINT ( 'NONE', #20314 ) ;
#20505 = ORIENTED_EDGE ( 'NONE', *, *, #15854, .F. ) ;
#20506 = CARTESIAN_POINT ( 'NONE',  ( 15.24356964374999990, 249.2593750006145115, -3.323476615752268604 ) ) ;
#20507 = CARTESIAN_POINT ( 'NONE',  ( 10.69584247140429589, 39.55231371789854933, 6.932735513424201024 ) ) ;
#20508 = CARTESIAN_POINT ( 'NONE',  ( 16.56230152254411081, -7.209453229046482114, -9.084374999385513405 ) ) ;
#20509 = CARTESIAN_POINT ( 'NONE',  ( 21.00000000000000000, -6.646953231504538984, -9.590624999385488181 ) ) ;
#20510 = CARTESIAN_POINT ( 'NONE',  ( -10.49813415416004858, 14.82731371789855501, 7.228626920338839135 ) ) ;
#20511 = CARTESIAN_POINT ( 'NONE',  ( -47.00000000000000711, 237.0000000000000000, 5.000000000000000000 ) ) ;
#20512 = ORIENTED_EDGE ( 'NONE', *, *, #322, .T. ) ;
#20513 = CARTESIAN_POINT ( 'NONE',  ( 22.80587116629411781, 7.646167579472024665E-16, -4.921874999385511984 ) ) ;
#20514 = EDGE_LOOP ( 'NONE', ( #18153, #23671, #12191, #33188 ) ) ;
#20515 = CARTESIAN_POINT ( 'NONE',  ( -1.926257025242585782E-15, 198.7906250006145399, -31.45816453501075927 ) ) ;
#20516 = CARTESIAN_POINT ( 'NONE',  ( 37.44889919624123564, 3.604726614523243278, 166.3748504141385922 ) ) ;
#20517 = CARTESIAN_POINT ( 'NONE',  ( -32.97544563604516554, 214.8429017333602360, 4.673758765035156415 ) ) ;
#20518 = CARTESIAN_POINT ( 'NONE',  ( 15.24356964374999990, 248.8093750006144944, -3.323476615752268604 ) ) ;
#20519 = EDGE_CURVE ( 'NONE', #33723, #23833, #17656, .T. ) ;
#20520 = DIRECTION ( 'NONE',  ( 0.08715574274765150453, 0.000000000000000000, 0.9961946980917461003 ) ) ;
#20521 = CARTESIAN_POINT ( 'NONE',  ( -53.16294563604516554, 213.2096571498974527, -3.378800118222469617 ) ) ;
#20522 = CARTESIAN_POINT ( 'NONE',  ( -31.99330436395490196, 210.1155267958017134, -6.500000000000000888 ) ) ;
#20523 = CARTESIAN_POINT ( 'NONE',  ( 31.39740774815230751, 7.209453229046475009, 168.8429143745260035 ) ) ;
#20524 = ORIENTED_EDGE ( 'NONE', *, *, #31868, .T. ) ;
#20525 = CARTESIAN_POINT ( 'NONE',  ( -8.927990412390371944, 17.12731371789855217, -13.04141134922778988 ) ) ;
#20526 = CARTESIAN_POINT ( 'NONE',  ( -57.52455436395489841, 203.6929966515020283, 6.137860380172978303 ) ) ;
#20527 = CARTESIAN_POINT ( 'NONE',  ( -7.954856959092191815, 133.1726862821014663, -5.529263428287477744 ) ) ;
#20528 = CARTESIAN_POINT ( 'NONE',  ( 2.660918448318279950, 42.89768628210143930, -12.46528703574805697 ) ) ;
#20529 = CARTESIAN_POINT ( 'NONE',  ( 19.56230152254412147, -5.196152422706635576, -5.250000000000060396 ) ) ;
#20530 = VERTEX_POINT ( 'NONE', #8926 ) ;
#20531 = CARTESIAN_POINT ( 'NONE',  ( -44.26413769728823411, 213.1499508600178672, 5.686928522499718142 ) ) ;
#20532 = DIRECTION ( 'NONE',  ( 0.000000000000000000, 0.000000000000000000, 1.000000000000000000 ) ) ;
#20533 = CARTESIAN_POINT ( 'NONE',  ( 8.710071997420127943, 17.88518628210143646, 3.796722387233375073 ) ) ;
#20534 = CARTESIAN_POINT ( 'NONE',  ( -27.24356964374999990, 196.6718750006145342, -15.72908226750537786 ) ) ;
#20535 = CARTESIAN_POINT ( 'NONE',  ( 5.649999999999987921, 244.5000000000000000, -2.499999999999999556 ) ) ;
#20536 = DIRECTION ( 'NONE',  ( 0.9961946980917462113, 0.000000000000000000, -0.08715574274765118534 ) ) ;
#20537 = CARTESIAN_POINT ( 'NONE',  ( 26.99999999999999645, 197.5625000000000000, -15.58845726811990495 ) ) ;
#20538 = CARTESIAN_POINT ( 'NONE',  ( 15.00000000000000000, 0.000000000000000000, -2.250000000000001776 ) ) ;
#20539 = CARTESIAN_POINT ( 'NONE',  ( 26.75643035624999655, 246.0343750006145456, -7.049594010296217766E-16 ) ) ;
#20540 = CARTESIAN_POINT ( 'NONE',  ( -5.233372021372612259, 87.85231371789855359, 8.152565276336593669 ) ) ;
#20541 = CARTESIAN_POINT ( 'NONE',  ( 15.24356964375000167, 239.9968750006145228, 3.323476615752272600 ) ) ;
#20542 = ORIENTED_EDGE ( 'NONE', *, *, #19180, .F. ) ;
#20543 = CARTESIAN_POINT ( 'NONE',  ( -57.92038769728821990, 208.1428034533959703, 6.469044688360770401 ) ) ;
#20544 = CARTESIAN_POINT ( 'NONE',  ( 15.00000000000000178, 246.0437500012290570, 3.464101615137757051 ) ) ;
#20545 = CARTESIAN_POINT ( 'NONE',  ( -8.962234695871565293, 99.63981371789856212, -8.715434833792128799 ) ) ;
#20546 = CARTESIAN_POINT ( 'NONE',  ( 10.31873187879410558, 3.604726614523240613, -2.484374999385500882 ) ) ;
#20547 = CARTESIAN_POINT ( 'NONE',  ( 33.75886329544200493, 5.407089921784857367, 160.0160109298142288 ) ) ;
#20548 = CARTESIAN_POINT ( 'NONE',  ( 23.87821517812500005, -4.985214923628404016, -2.353124999385475036 ) ) ;
#20549 = CARTESIAN_POINT ( 'NONE',  ( -2.660918448318004614, 72.90231371789855075, -12.46528703574811558 ) ) ;
#20550 = CARTESIAN_POINT ( 'NONE',  ( 13.62178482187499640, 198.3593750006145342, -23.59362340125807123 ) ) ;
#20551 = ORIENTED_EDGE ( 'NONE', *, *, #18504, .F. ) ;
#20552 = EDGE_LOOP ( 'NONE', ( #24496, #11253, #20524, #34352 ) ) ;
#20553 = CARTESIAN_POINT ( 'NONE',  ( 20.99999999999999645, 6.646953231504538984, -5.203124999385457805 ) ) ;
#20554 = ADVANCED_BREP_SHAPE_REPRESENTATION ( '', ( #7886, #17215 ), #24466 ) ;
#20555 = CARTESIAN_POINT ( 'NONE',  ( -7.234628195640263826, 195.4075961894323825, -27.00000000000003553 ) ) ;
#20556 = CARTESIAN_POINT ( 'NONE',  ( 18.12178482187500350, 246.6718750006145342, 4.985214923628407568 ) ) ;
#20557 = CARTESIAN_POINT ( 'NONE',  ( 11.61527771782819940, 35.13518628210143646, -4.622313124798573369 ) ) ;
#20558 = CARTESIAN_POINT ( 'NONE',  ( -47.22544563604515844, 214.8429017333602360, 4.673758765035156415 ) ) ;
#20559 = FILL_AREA_STYLE ('',( #20745 ) ) ;
#20560 = CARTESIAN_POINT ( 'NONE',  ( -35.74627896937850124, 205.4690446883607535, -1.090244570138286351 ) ) ;
#20561 = DIRECTION ( 'NONE',  ( 0.000000000000000000, 0.000000000000000000, 1.000000000000000000 ) ) ;
#20562 = CARTESIAN_POINT ( 'NONE',  ( 36.88023945835949746, 3.464101615137755275, 162.6696881154131518 ) ) ;
#20563 = CARTESIAN_POINT ( 'NONE',  ( -8.962234695871565293, 108.8398137178985507, -8.715434833792128799 ) ) ;
#20564 = CARTESIAN_POINT ( 'NONE',  ( -64.05580436395490551, 214.5000000000000284, 0.1155267958017899832 ) ) ;
#20565 = CARTESIAN_POINT ( 'NONE',  ( -65.24330436395489130, 210.1155267958017134, -6.500000000000000888 ) ) ;
#20566 = CARTESIAN_POINT ( 'NONE',  ( 18.12178482187499640, 4.985214923628404904, -4.828124999385480010 ) ) ;
#20567 = CARTESIAN_POINT ( 'NONE',  ( 27.00000000000041567, 3.464101615137513690, -0.6375000000000179412 ) ) ;
#20568 = CARTESIAN_POINT ( 'NONE',  ( 14.25334919248795451, 74.91481371789855359, -6.092822981423661410 ) ) ;
#20569 = CARTESIAN_POINT ( 'NONE',  ( -52.17336230271184405, 217.4189793300686233, 4.149950860017807663 ) ) ;
#20570 = ORIENTED_EDGE ( 'NONE', *, *, #18215, .T. ) ;
#20571 = CARTESIAN_POINT ( 'NONE',  ( 0.000000000000000000, -20.00000000000000000, 0.000000000000000000 ) ) ;
#20572 = CARTESIAN_POINT ( 'NONE',  ( 4.944772684328679446, 98.38518628210145778, -11.48171059495397373 ) ) ;
#20573 = CARTESIAN_POINT ( 'NONE',  ( -11.08355503943142573, 48.36018628210145209, 10.83675517735155402 ) ) ;
#20574 = DIRECTION ( 'NONE',  ( -0.000000000000000000, -1.000000000000000000, -0.000000000000000000 ) ) ;
#20575 = CARTESIAN_POINT ( 'NONE',  ( 24.36214585379926589, -3.604726614523244610, 160.0664306802028136 ) ) ;
#20576 = CARTESIAN_POINT ( 'NONE',  ( 5.770363421893814682, 74.23518628210142367, 14.38691631536207183 ) ) ;
#20577 = CARTESIAN_POINT ( 'NONE',  ( 5.778771075727756162E-15, 199.0156250006145342, 31.45816453501076637 ) ) ;
#20578 = CARTESIAN_POINT ( 'NONE',  ( 22.80587116629411071, 3.604726614523238837, -9.778124999385537919 ) ) ;
#20579 = CARTESIAN_POINT ( 'NONE',  ( 10.56230152254305032, 3.464101615137144652, -8.587500000000064304 ) ) ;
#20580 = CARTESIAN_POINT ( 'NONE',  ( -55.94122103062156270, 208.3738570449993404, -6.530955311639226935 ) ) ;
#20581 = CARTESIAN_POINT ( 'NONE',  ( 11.14485736792927284, 2.876095549794589257, -10.00000000000000000 ) ) ;
#20582 = CARTESIAN_POINT ( 'NONE',  ( -0.1745138560725500443, 47.21018628210143930, 12.50000000000000355 ) ) ;
#20583 = CARTESIAN_POINT ( 'NONE',  ( -13.49999999999998401, 195.1250000000000284, 23.38268590217985476 ) ) ;
#20584 = CARTESIAN_POINT ( 'NONE',  ( 18.00000000000000000, 5.196152422706630247, -3.618749998770959486 ) ) ;
#20585 = CARTESIAN_POINT ( 'NONE',  ( -5.233372021372430183, 4.947686282101431132, -8.152565276336710909 ) ) ;
#20586 = CARTESIAN_POINT ( 'NONE',  ( 18.12178482187499640, 246.1843750006145228, -4.985214923628404904 ) ) ;
#20587 = VECTOR ( 'NONE', #1550, 1000.000000000000000 ) ;
#20588 = EDGE_LOOP ( 'NONE', ( #35154, #24545, #1222, #27022, #16742, #29861, #12825, #3, #37466, #10620, #11266, #14738 ) ) ;
#20589 = CARTESIAN_POINT ( 'NONE',  ( 26.99999999999999645, 3.464101615137755275, -7.837500000000007461 ) ) ;
#20590 = CARTESIAN_POINT ( 'NONE',  ( 22.60769515458672885, 243.3825961894323484, 5.999999999999997335 ) ) ;
#20591 = EDGE_CURVE ( 'NONE', #5529, #21803, #21680, .T. ) ;
#20592 = CYLINDRICAL_SURFACE ( 'NONE', #5593, 5.999999999999999112 ) ;
#20593 = CARTESIAN_POINT ( 'NONE',  ( 22.80587116629410716, 7.646167579472015790E-16, -3.965624999385547689 ) ) ;
#20594 = CARTESIAN_POINT ( 'NONE',  ( 24.91612954363903043, -3.604726614523240613, 166.3984932299484569 ) ) ;
#20595 = CARTESIAN_POINT ( 'NONE',  ( 18.00000000000000355, 241.9749999999999943, 5.196152422706632912 ) ) ;
#20596 = DIRECTION ( 'NONE',  ( -2.057406622567553763E-16, 0.000000000000000000, 1.000000000000000000 ) ) ;
#20597 = EDGE_CURVE ( 'NONE', #15372, #21580, #7395, .T. ) ;
#20598 = CARTESIAN_POINT ( 'NONE',  ( 7.228626920339069173, 61.87268628210144783, -10.49813415415989404 ) ) ;
#20599 = ORIENTED_EDGE ( 'NONE', *, *, #34724, .F. ) ;
#20600 = VERTEX_POINT ( 'NONE', #29939 ) ;
#20601 = LINE ( 'NONE', #26453, #13384 ) ;
#20602 = CARTESIAN_POINT ( 'NONE',  ( 26.99999999999999645, 246.6250000000000000, -7.347880794884117764E-16 ) ) ;
#20603 = CARTESIAN_POINT ( 'NONE',  ( 1.120210788295102201E-13, 195.3875000000000455, -27.00000000000000711 ) ) ;
#20604 = CARTESIAN_POINT ( 'NONE',  ( 15.24356964374999990, 3.323476615752268604, -5.578124999385491556 ) ) ;
#20605 = CIRCLE ( 'NONE', #24226, 27.00000000000000000 ) ;
#20606 = CARTESIAN_POINT ( 'NONE',  ( 11.08355503943118769, 12.23981371789853512, 10.83675517735179028 ) ) ;
#20607 = DIRECTION ( 'NONE',  ( -0.8083506638593009885, -0.5887012860850802110, 0.000000000000000000 ) ) ;
#20608 = ADVANCED_FACE ( 'NONE', ( #12507 ), #934, .T. ) ;
#20609 = CARTESIAN_POINT ( 'NONE',  ( 26.75643035624999655, 241.1218750006145228, -3.323476615752271712 ) ) ;
#20610 = CARTESIAN_POINT ( 'NONE',  ( -34.56622103062156981, 211.0902445701382533, 4.530955311639240257 ) ) ;
#20611 = CARTESIAN_POINT ( 'NONE',  ( 2.999999999999997335, 244.5000000000000000, 5.000000000000000000 ) ) ;
#20612 = CARTESIAN_POINT ( 'NONE',  ( 33.70166733926387082, -5.407089921784861808, 159.3622581591915548 ) ) ;
#20613 = CARTESIAN_POINT ( 'NONE',  ( 3.474262827703532341, 18.56481371789855928, -8.843639120294245259 ) ) ;
#20614 = CARTESIAN_POINT ( 'NONE',  ( -56.73288769728823411, 203.5309553116391612, -1.857196546604028775 ) ) ;
#20615 = CARTESIAN_POINT ( 'NONE',  ( -48.80877896937850124, 212.1620413398627534, -8.530955311639255356 ) ) ;
#20616 = DIRECTION ( 'NONE',  ( 0.08715574274765144902, 0.9961946980917462113, 0.000000000000000000 ) ) ;
#20617 = CARTESIAN_POINT ( 'NONE',  ( 19.61859908393741492, 194.9999999999999432, 18.97589165950046208 ) ) ;
#20618 = CARTESIAN_POINT ( 'NONE',  ( -13.62178482187500528, 196.1843750006145228, -23.59362340125807123 ) ) ;
#20619 = CARTESIAN_POINT ( 'NONE',  ( 2.908627838312458636, 137.8773137178985735, -15.53471296425188442 ) ) ;
#20620 = CARTESIAN_POINT ( 'NONE',  ( -56.92336230271182984, 215.6869285224997270, 3.149950860017831200 ) ) ;
#20621 = EDGE_LOOP ( 'NONE', ( #33295, #9854, #7485, #11218 ) ) ;
#20622 = CARTESIAN_POINT ( 'NONE',  ( -11.61527771782819940, 48.93518628210144783, 4.622313124798574258 ) ) ;
#20623 = CYLINDRICAL_SURFACE ( 'NONE', #14723, 9.999999999999998224 ) ;
#20624 = CARTESIAN_POINT ( 'NONE',  ( 26.99999999999999645, 198.9125000000000512, -15.58845726811990495 ) ) ;
#20625 = CARTESIAN_POINT ( 'NONE',  ( 31.41211527974097706, -7.209453229046482114, 169.0110222298289671 ) ) ;
#20626 = CARTESIAN_POINT ( 'NONE',  ( 23.99999999999999645, 5.196152422706631135, -1.443749998770949006 ) ) ;
#20627 = CARTESIAN_POINT ( 'NONE',  ( 16.56230152254411436, -7.209453229046482114, -7.734374999385493332 ) ) ;
#20628 = DIRECTION ( 'NONE',  ( 1.000000000000000000, 0.000000000000000000, 0.000000000000000000 ) ) ;
#20629 = CARTESIAN_POINT ( 'NONE',  ( 22.80587116629411071, 3.604726614523238837, -1.228124999385522331 ) ) ;
#20630 = CARTESIAN_POINT ( 'NONE',  ( 1.715153634034233487, 65.32268628210144357, 9.534712964251941258 ) ) ;
#20631 = DIRECTION ( 'NONE',  ( -0.000000000000000000, -1.000000000000000000, -0.000000000000000000 ) ) ;
#20632 = CARTESIAN_POINT ( 'NONE',  ( 24.00000000000000000, 245.6500000000000057, 5.196152422706629359 ) ) ;
#20633 = CARTESIAN_POINT ( 'NONE',  ( -7.228626920339069173, 103.2726862821014606, 10.49813415415989581 ) ) ;
#20634 = CARTESIAN_POINT ( 'NONE',  ( 36.95541128647934670, 7.347880794884117764E-16, 163.5289060425172636 ) ) ;
#20635 = DIRECTION ( 'NONE',  ( 1.000000000000000000, 0.000000000000000000, 0.000000000000000000 ) ) ;
#20636 = VERTEX_POINT ( 'NONE', #12688 ) ;
#20637 = CARTESIAN_POINT ( 'NONE',  ( 33.74578993402985816, -5.407089921784855591, 159.8665817251004739 ) ) ;
#20638 = CARTESIAN_POINT ( 'NONE',  ( 23.87821517812499650, 4.985214923628404904, -7.940624999385470062 ) ) ;
#20639 = CARTESIAN_POINT ( 'NONE',  ( 31.11796464796764994, 7.209453229046482114, 165.6488651237693261 ) ) ;
#20640 = CARTESIAN_POINT ( 'NONE',  ( 24.96839150574091093, 3.464101615137757051, 164.2012019424803100 ) ) ;
#20641 = DIRECTION ( 'NONE',  ( -0.000000000000000000, -1.000000000000000000, -0.000000000000000000 ) ) ;
#20642 = CARTESIAN_POINT ( 'NONE',  ( 26.99999999999999645, 249.2874999999999943, 3.464101615137751278 ) ) ;
#20643 = CARTESIAN_POINT ( 'NONE',  ( -27.24356964375000345, 199.3531250006145399, 0.000000000000000000 ) ) ;
#20644 = CARTESIAN_POINT ( 'NONE',  ( -6.932735513424201912, 106.2523137178985735, 10.69584247140429412 ) ) ;
#20645 = CARTESIAN_POINT ( 'NONE',  ( -2.311890736173176641, 115.9226862821014521, -12.53471296425194659 ) ) ;
#20646 = VECTOR ( 'NONE', #3708, 1000.000000000000000 ) ;
#20648 = ORIENTED_EDGE ( 'NONE', *, *, #5426, .F. ) ;
#20647 = EDGE_LOOP ( 'NONE', ( #32941, #33178, #33882, #14319 ) ) ;
#20649 = CARTESIAN_POINT ( 'NONE',  ( 27.24356964374999635, 195.1156250006145001, -15.72908226750539029 ) ) ;
#20650 = CARTESIAN_POINT ( 'NONE',  ( 18.12178482187500350, 243.0718750006145399, 4.985214923628407568 ) ) ;
#20651 = CARTESIAN_POINT ( 'NONE',  ( 15.46528703574811736, 93.60231371789855359, -3.257655550456947768 ) ) ;
#20652 = CARTESIAN_POINT ( 'NONE',  ( 21.00000000000000000, -6.646953231504538984, -4.190624999385508254 ) ) ;
#20653 = CARTESIAN_POINT ( 'NONE',  ( 15.24356964374999990, 248.5093750006145399, 0.000000000000000000 ) ) ;
#20654 = CARTESIAN_POINT ( 'NONE',  ( 3.474262827703335166, 92.63518628210147199, 8.843639120294326972 ) ) ;
#20655 = CARTESIAN_POINT ( 'NONE',  ( -13.50000000000000533, 195.5375000012290343, -23.38268590217984411 ) ) ;
#20656 = CARTESIAN_POINT ( 'NONE',  ( -7.954856959092309943, 70.02731371789855075, 5.529263428287300108 ) ) ;
#20657 = CARTESIAN_POINT ( 'NONE',  ( 16.56230152254411081, 7.209453229046475009, -4.303124999385498306 ) ) ;
#20658 = CARTESIAN_POINT ( 'NONE',  ( 23.87821517812499650, 241.4968750006144944, -4.985214923628404904 ) ) ;
#20659 = CARTESIAN_POINT ( 'NONE',  ( 12.46528703574811558, 56.80231371789856354, -2.660918448318005503 ) ) ;
#20660 = CARTESIAN_POINT ( 'NONE',  ( 36.87697111800645899, 7.347880794884117764E-16, 162.6323308142347059 ) ) ;
#20661 = MANIFOLD_SOLID_BREP ( 'M5 Clearance Hole1', #18063 ) ;
#20662 = CARTESIAN_POINT ( 'NONE',  ( 8.715434833791931624, 101.2601862821014578, 8.962234695871760692 ) ) ;
#20663 = CARTESIAN_POINT ( 'NONE',  ( 19.56230152254410370, 5.196152422706631135, -7.237499998771018461 ) ) ;
#20664 = CARTESIAN_POINT ( 'NONE',  ( -63.26413769728823411, 212.1499508600178387, 3.954877714930865817 ) ) ;
#20665 = CARTESIAN_POINT ( 'NONE',  ( 4.622313124798573369, 138.6351862821014720, 11.61527771782819940 ) ) ;
#20666 = AXIS2_PLACEMENT_3D ( 'NONE', #18390, #3967, #9289 ) ;
#20667 = CARTESIAN_POINT ( 'NONE',  ( -3.257655550457281723, 84.29768628210146630, 15.46528703574804986 ) ) ;
#20668 =( NAMED_UNIT ( * ) SI_UNIT ( $, .STERADIAN. ) SOLID_ANGLE_UNIT ( ) );
#20669 = CARTESIAN_POINT ( 'NONE',  ( -80.98946968704737515, 222.6276076386831733, 7.500000000000000000 ) ) ;
#20670 = CARTESIAN_POINT ( 'NONE',  ( -9.500000000000005329, 113.9101862821014493, -0.1745138560725176813 ) ) ;
#20671 = CARTESIAN_POINT ( 'NONE',  ( 14.25334919248782661, 8.685186282101437172, 6.092822981423971385 ) ) ;
#20672 = CARTESIAN_POINT ( 'NONE',  ( 27.24356964375000700, 195.9968750006145513, 15.72908226750537075 ) ) ;
#20673 = CARTESIAN_POINT ( 'NONE',  ( 15.24356964374999990, 242.9593750006145001, -3.323476615752268604 ) ) ;
#20674 = ORIENTED_EDGE ( 'NONE', *, *, #33601, .F. ) ;
#20675 = CARTESIAN_POINT ( 'NONE',  ( 24.99130137175887612, 0.000000000000000000, 167.2577111570525972 ) ) ;
#20676 = CARTESIAN_POINT ( 'NONE',  ( 3.796722387233379514, 52.38518628210145778, -8.710071997420127943 ) ) ;
#20677 = CARTESIAN_POINT ( 'NONE',  ( 15.24356964374999990, 3.323476615752268604, -1.528124999385498173 ) ) ;
#20678 = CARTESIAN_POINT ( 'NONE',  ( 0.000000000000000000, 200.0000000000000000, 0.000000000000000000 ) ) ;
#20680 = CARTESIAN_POINT ( 'NONE',  ( 20.99999999999999645, -6.928203230275506996, -4.781249998770952914 ) ) ;
#20679 =( BOUNDED_CURVE ( )  B_SPLINE_CURVE ( 2, ( #5273, #36359, #7569, #11153, #7941, #22350, #1869 ),
 .UNSPECIFIED., .F., .F. ) 
 B_SPLINE_CURVE_WITH_KNOTS ( ( 3, 2, 2, 3 ),
 ( 0.2608695652173908530, 0.2681159420289850326, 0.2753623188405791011, 0.2826086956521732252 ),
 .UNSPECIFIED. ) 
 CURVE ( )  GEOMETRIC_REPRESENTATION_ITEM ( )  RATIONAL_B_SPLINE_CURVE ( ( 1.000000000000008216, 0.8660254037844304920, 1.000000000000000000, 0.8660254037844387076, 1.000000000000000000, 0.8660254037844510311, 0.9999999999999876765 ) ) 
 REPRESENTATION_ITEM ( '' )  );
#20681 = CARTESIAN_POINT ( 'NONE',  ( 20.99999999999999645, 245.2187500012290116, 5.999999999999998224 ) ) ;
#20682 = CARTESIAN_POINT ( 'NONE',  ( 2.867614517141320096, 194.9999999999999432, 27.09578238708614961 ) ) ;
#20683 = CARTESIAN_POINT ( 'NONE',  ( 27.00000000000001421, 198.3875000000000171, 15.58845726811988897 ) ) ;
#20684 = CARTESIAN_POINT ( 'NONE',  ( -9.534712964251895073, 34.37731371789854506, -1.715153634034446428 ) ) ;
#20685 = CARTESIAN_POINT ( 'NONE',  ( 22.56230152254412502, 7.347880794884125653E-16, -2.925000000000066436 ) ) ;
#20686 = ORIENTED_EDGE ( 'NONE', *, *, #1589, .F. ) ;
#20687 = CARTESIAN_POINT ( 'NONE',  ( 23.87821517812499650, 249.5968750006145171, -4.985214923628404904 ) ) ;
#20689 = AXIS2_PLACEMENT_3D ( 'NONE', #36560, #21298, #10601 ) ;
#20688 = CARTESIAN_POINT ( 'NONE',  ( -2.660918448318005058, 45.30231371789855643, -12.46528703574811558 ) ) ;
#20690 = CARTESIAN_POINT ( 'NONE',  ( 23.87821517812500005, -4.985214923628404016, -9.553124999385486760 ) ) ;
#20691 = CARTESIAN_POINT ( 'NONE',  ( 12.53471296425189330, 11.37731371789854506, 2.311890736173451977 ) ) ;
#20692 = CARTESIAN_POINT ( 'NONE',  ( 24.00000000000000000, 247.9000000000000057, 5.196152422706629359 ) ) ;
#20693 = EDGE_LOOP ( 'NONE', ( #16219, #6655, #10237, #4007 ) ) ;
#20694 = CARTESIAN_POINT ( 'NONE',  ( 16.56230152254411436, 7.209453229046482114, -3.459374999385518734 ) ) ;
#20695 = CIRCLE ( 'NONE', #9188, 4.899999999999999467 ) ;
#20696 = CARTESIAN_POINT ( 'NONE',  ( -13.62178482187498396, 198.0781250006145342, 23.59362340125808188 ) ) ;
#20697 = CARTESIAN_POINT ( 'NONE',  ( 37.44563085588819717, 7.646167579472024665E-16, 166.3374931129601464 ) ) ;
#20698 =( BOUNDED_CURVE ( )  B_SPLINE_CURVE ( 3, ( #9577, #9391, #30230, #20965 ),
 .UNSPECIFIED., .F., .F. ) 
 B_SPLINE_CURVE_WITH_KNOTS ( ( 4, 4 ),
 ( 4.712388980384689674, 7.853981633974482790 ),
 .UNSPECIFIED. ) 
 CURVE ( )  GEOMETRIC_REPRESENTATION_ITEM ( )  RATIONAL_B_SPLINE_CURVE ( ( 1.000000000000000000, 0.3333333333333333703, 0.3333333333333333703, 1.000000000000000000 ) ) 
 REPRESENTATION_ITEM ( '' )  );
#20699 = CARTESIAN_POINT ( 'NONE',  ( -35.94419563604516554, 203.5000000000000000, 0.1155267958017914542 ) ) ;
#20700 = CARTESIAN_POINT ( 'NONE',  ( 26.75643035624999655, 249.5593750006144944, -3.323476615752271268 ) ) ;
#20701 = CYLINDRICAL_SURFACE ( 'NONE', #13986, 5.000000000000000888 ) ;
#20702 = CARTESIAN_POINT ( 'NONE',  ( -57.91294563604517265, 213.2096571498974527, -3.378800118222469617 ) ) ;
#20704 = EDGE_CURVE ( 'NONE', #9483, #12534, #9828, .T. ) ;
#20703 = CARTESIAN_POINT ( 'NONE',  ( -33.97247103062156270, 206.6499508600178672, 5.571401726697986057 ) ) ;
#20705 = CARTESIAN_POINT ( 'NONE',  ( 25.14491336835161306, 3.604726614523236616, 169.0135043124392951 ) ) ;
#20706 = ORIENTED_EDGE ( 'NONE', *, *, #30955, .F. ) ;
#20707 = CARTESIAN_POINT ( 'NONE',  ( 22.60769515458672885, 248.1236538117966859, -6.000000000000000000 ) ) ;
#20708 = CARTESIAN_POINT ( 'NONE',  ( 14.38691631536194393, 30.06481371789855572, 5.770363421894124656 ) ) ;
#20709 = CARTESIAN_POINT ( 'NONE',  ( -64.64955436395490551, 216.3070033484980002, -6.137860380172975638 ) ) ;
#20710 = VECTOR ( 'NONE', #2246, 1000.000000000000000 ) ;
#20711 = CARTESIAN_POINT ( 'NONE',  ( -9.500000000000005329, 123.1101862821014663, -0.1745138560725176813 ) ) ;
#20712 = CARTESIAN_POINT ( 'NONE',  ( 12.53471296425194836, 35.42268628210144499, -2.311890736173178418 ) ) ;
#20713 = CARTESIAN_POINT ( 'NONE',  ( 16.56230152254411436, 6.928203230275514990, -5.512500000000036593 ) ) ;
#20714 = ORIENTED_EDGE ( 'NONE', *, *, #16331, .F. ) ;
#20715 = CARTESIAN_POINT ( 'NONE',  ( -38.32663769728824121, 204.3130714775002730, 3.149950860017883603 ) ) ;
#20716 = FACE_OUTER_BOUND ( 'NONE', #31605, .T. ) ;
#20717 = CARTESIAN_POINT ( 'NONE',  ( -3.474262827703337830, 14.43518628210144072, -8.843639120294326972 ) ) ;
#20718 = CARTESIAN_POINT ( 'NONE',  ( -13.62178482187500528, 195.2843750006145456, -23.59362340125807123 ) ) ;
#20719 = DIRECTION ( 'NONE',  ( 0.08715574274765150453, 0.000000000000000000, 0.9961946980917461003 ) ) ;
#20720 = CARTESIAN_POINT ( 'NONE',  ( -50.22894823740646331, 235.3444610600932094, -7.500000000000000000 ) ) ;
#20721 = EDGE_CURVE ( 'NONE', #9774, #23018, #12119, .T. ) ;
#20722 = CARTESIAN_POINT ( 'NONE',  ( 37.38683221308021842, 7.347880794884117764E-16, 168.4600697980714017 ) ) ;
#20723 = CARTESIAN_POINT ( 'NONE',  ( 26.75643035624999655, 245.1343750006145115, -7.049594010296217766E-16 ) ) ;
#20724 = CARTESIAN_POINT ( 'NONE',  ( 8.152565276336593669, 85.55231371789855643, 5.233372021372610483 ) ) ;
#20725 = CARTESIAN_POINT ( 'NONE',  ( 3.306546357697854128E-15, 200.0000000000000000, 27.00000000000000355 ) ) ;
#20726 = ORIENTED_EDGE ( 'NONE', *, *, #33945, .T. ) ;
#20727 = CARTESIAN_POINT ( 'NONE',  ( -51.78497103062156981, 204.4285982733020148, -3.350049139982115509 ) ) ;
#20728 = EDGE_CURVE ( 'NONE', #14336, #21814, #23693, .T. ) ;
#20729 = CARTESIAN_POINT ( 'NONE',  ( 24.00000000000000000, 246.6062500012290570, 5.196152422706629359 ) ) ;
#20730 = CARTESIAN_POINT ( 'NONE',  ( 8.715434833792128799, 92.73981371789855643, -8.962234695871567070 ) ) ;
#20731 = CARTESIAN_POINT ( 'NONE',  ( 13.44051670066911264, 5.407089921784862696, -2.521874999385525840 ) ) ;
#20732 = CARTESIAN_POINT ( 'NONE',  ( 24.43895185209563792, 3.604726614523236616, 160.9443272578961626 ) ) ;
#20733 = CARTESIAN_POINT ( 'NONE',  ( 23.87821517812500005, -4.985214923628404016, -3.253124999385486937 ) ) ;
#20734 = CARTESIAN_POINT ( 'NONE',  ( -12.46528703574811558, 61.40231371789855785, 2.660918448318003726 ) ) ;
#20735 = CARTESIAN_POINT ( 'NONE',  ( 13.62178482187501416, 198.2093750006145285, 23.59362340125806767 ) ) ;
#20736 = EDGE_CURVE ( 'NONE', #24665, #25759, #17806, .T. ) ;
#20737 = VERTEX_POINT ( 'NONE', #369 ) ;
#20738 = ORIENTED_EDGE ( 'NONE', *, *, #20933, .F. ) ;
#20739 = CARTESIAN_POINT ( 'NONE',  ( 26.75643035624999655, 7.049594010296217766E-16, -4.415624999385469707 ) ) ;
#20740 = CARTESIAN_POINT ( 'NONE',  ( -82.45892874490161262, 210.6708926576488921, -5.000000000000000000 ) ) ;
#20741 =( BOUNDED_CURVE ( )  B_SPLINE_CURVE ( 2, ( #1213, #32875, #26432, #20767, #9387, #12221, #12412 ),
 .UNSPECIFIED., .F., .F. ) 
 B_SPLINE_CURVE_WITH_KNOTS ( ( 3, 2, 2, 3 ),
 ( 0.2391304347826091470, 0.2463768115942034931, 0.2536231884057978392, 0.2608695652173921298 ),
 .UNSPECIFIED. ) 
 CURVE ( )  GEOMETRIC_REPRESENTATION_ITEM ( )  RATIONAL_B_SPLINE_CURVE ( ( 0.9999999999999917843, 0.8660254037844469233, 1.000000000000000000, 0.8660254037844387076, 1.000000000000000000, 0.8660254037844232755, 1.000000000000015321 ) ) 
 REPRESENTATION_ITEM ( '' )  );
#20742 = CARTESIAN_POINT ( 'NONE',  ( 15.24356964375000167, 247.5343750006144887, 3.323476615752272600 ) ) ;
#20743 = CARTESIAN_POINT ( 'NONE',  ( -8.962234695871760692, 39.16018628210144215, 8.715434833791933400 ) ) ;
#20744 = CARTESIAN_POINT ( 'NONE',  ( -47.42336230271183695, 215.6869285224997270, 3.149950860017831200 ) ) ;
#20745 = FILL_AREA_STYLE_COLOUR ( '', #9337 ) ;
#20746 = CARTESIAN_POINT ( 'NONE',  ( -31.19419563604517265, 205.4999999999999716, 0.1155267958017633378 ) ) ;
#20747 = SURFACE_SIDE_STYLE ('',( #18474 ) ) ;
#20748 = CARTESIAN_POINT ( 'NONE',  ( 33.69882328325508070, 5.196152422706631135, 160.7270745741280962 ) ) ;
#20749 = CARTESIAN_POINT ( 'NONE',  ( -10.49813415416004858, 88.42731371789858485, 7.228626920338839135 ) ) ;
#20750 = CARTESIAN_POINT ( 'NONE',  ( -56.13913769728823411, 207.8500491399821613, -3.954877714930864485 ) ) ;
#20751 = CARTESIAN_POINT ( 'NONE',  ( -65.44122103062157692, 208.3738570449993404, -6.530955311639226935 ) ) ;
#20752 = CARTESIAN_POINT ( 'NONE',  ( 26.75643035624999655, -3.323476615752267271, -6.815624999385487826 ) ) ;
#20753 = CARTESIAN_POINT ( 'NONE',  ( 15.00000000000010658, 3.464101615137812562, -2.287500000000008527 ) ) ;
#20754 = CARTESIAN_POINT ( 'NONE',  ( -13.04141134922778456, 70.02731371789855075, 8.927990412390377273 ) ) ;
#20755 = CARTESIAN_POINT ( 'NONE',  ( -60.68377896937850835, 207.8379586601372750, 8.530955311639258909 ) ) ;
#20756 = EDGE_CURVE ( 'NONE', #13615, #33723, #24399, .T. ) ;
#20757 = EDGE_LOOP ( 'NONE', ( #17055, #6216, #15698, #33758 ) ) ;
#20758 = PLANE ( 'NONE',  #18044 ) ;
#20759 = CARTESIAN_POINT ( 'NONE',  ( 10.49813415415989581, 110.1726862821014521, 7.228626920339068285 ) ) ;
#20760 = CARTESIAN_POINT ( 'NONE',  ( -13.04141134922759804, 50.37268628210144783, -8.927990412390657937 ) ) ;
#20761 = CARTESIAN_POINT ( 'NONE',  ( 3.306546357697854128E-15, 200.0000000000000000, 27.00000000000000355 ) ) ;
#20762 = CARTESIAN_POINT ( 'NONE',  ( 27.57990657358465114, 5.407089921784862696, 161.0271401442424803 ) ) ;
#20763 = CARTESIAN_POINT ( 'NONE',  ( 2.908627838312118019, 56.12268628210142651, 15.53471296425195369 ) ) ;
#20764 = CARTESIAN_POINT ( 'NONE',  ( -54.50000000000000711, 244.5000000000000000, -5.000000000000000000 ) ) ;
#20765 = EDGE_CURVE ( 'NONE', #55, #32329, #8602, .T. ) ;
#20766 = CARTESIAN_POINT ( 'NONE',  ( 16.56230152254411081, -7.209453229046475009, -9.028124999385500615 ) ) ;
#20767 = CARTESIAN_POINT ( 'NONE',  ( 16.56230152254411792, -6.928203230275514990, -2.587500000000015454 ) ) ;
#20768 = CARTESIAN_POINT ( 'NONE',  ( -48.61830436395490551, 209.8844732041982581, 6.500000000000000888 ) ) ;
#20769 = CARTESIAN_POINT ( 'NONE',  ( 10.59328565399995803, 1.478247113626270481, -10.00000000000000355 ) ) ;
#20770 = CARTESIAN_POINT ( 'NONE',  ( 10.69584247140445221, 34.84768628210143504, -6.932735513423970097 ) ) ;
#20771 = DIRECTION ( 'NONE',  ( -0.000000000000000000, -0.000000000000000000, -1.000000000000000000 ) ) ;
#20772 = CARTESIAN_POINT ( 'NONE',  ( 2.064181346179272847, 6.097686282101443922, -9.465287035748065847 ) ) ;
#20773 = CARTESIAN_POINT ( 'NONE',  ( 26.75643035624999655, 246.9343750006145228, -7.049594010296217766E-16 ) ) ;
#20774 = ORIENTED_EDGE ( 'NONE', *, *, #35891, .T. ) ;
#20775 = CARTESIAN_POINT ( 'NONE',  ( 21.00000000000000000, -6.928203230275506996, -7.987499999999996270 ) ) ;
#20777 = DIRECTION ( 'NONE',  ( 0.000000000000000000, 0.000000000000000000, 1.000000000000000000 ) ) ;
#20776 = PRODUCT_DEFINITION_SHAPE ( 'NONE', 'NONE',  #37501 ) ;
#20778 = EDGE_CURVE ( 'NONE', #28622, #11418, #4939, .T. ) ;
#20779 = CARTESIAN_POINT ( 'NONE',  ( 27.00000000000015632, 3.464101615137663348, -6.881249998770978316 ) ) ;
#20780 = CARTESIAN_POINT ( 'NONE',  ( 10.31873187879411269, 3.604726614523236616, -4.678124999385532945 ) ) ;
#20781 = CARTESIAN_POINT ( 'NONE',  ( 37.52897353489062482, 7.646167579472015790E-16, 167.2901042930103586 ) ) ;
#20782 = CARTESIAN_POINT ( 'NONE',  ( 26.99999999999999645, 241.7125000000000057, -3.464101615137755275 ) ) ;
#20783 = CARTESIAN_POINT ( 'NONE',  ( -10.38977131807862975, 218.0044321092237283, 3.786121002044094741 ) ) ;
#20784 = CARTESIAN_POINT ( 'NONE',  ( 12.46528703574805874, 54.39768628210145351, 2.660918448318279950 ) ) ;
#20785 = ORIENTED_EDGE ( 'NONE', *, *, #9857, .T. ) ;
#20786 = ORIENTED_EDGE ( 'NONE', *, *, #21200, .T. ) ;
#20787 = CARTESIAN_POINT ( 'NONE',  ( 0.000000000000000000, 200.0000000000000000, -25.00000000000000000 ) ) ;
#20788 = CARTESIAN_POINT ( 'NONE',  ( 24.58926402489574770, 0.000000000000000000, 159.8677550070055702 ) ) ;
#20789 = CARTESIAN_POINT ( 'NONE',  ( -47.00000000000000711, 244.5000000000000000, 2.500000000000001776 ) ) ;
#20790 = CARTESIAN_POINT ( 'NONE',  ( 21.00000000000000000, -6.646953231504538984, -6.328124999385495997 ) ) ;
#20791 = CARTESIAN_POINT ( 'NONE',  ( -12.53471296425194836, 104.4226862821014379, 2.311890736173176641 ) ) ;
#20792 = CARTESIAN_POINT ( 'NONE',  ( 10.83675517735179206, 28.33981371789855430, -11.08355503943118769 ) ) ;
#20793 = MANIFOLD_SOLID_BREP ( 'Fillet1', #27737 ) ;
#20794 = DIRECTION ( 'NONE',  ( 1.000000000000000000, 0.000000000000000000, 0.000000000000000000 ) ) ;
#20795 = CARTESIAN_POINT ( 'NONE',  ( 23.87821517812499650, 240.2593750006145399, -4.985214923628404904 ) ) ;
#20796 = CARTESIAN_POINT ( 'NONE',  ( -36.34747103062156981, 212.3500491399821613, -3.839350919129076445 ) ) ;
#20797 = B_SPLINE_CURVE_WITH_KNOTS ( 'NONE', 3,
 ( #27110, #24456, #35817, #12891 ),
 .UNSPECIFIED., .F., .F.,
 ( 4, 4 ),
 ( 0.000000000000000000, 1.000000000000000000 ),
 .UNSPECIFIED. ) ;
#20798 = CYLINDRICAL_SURFACE ( 'NONE', #9486, 27.00000000000000355 ) ;
#20799 = CARTESIAN_POINT ( 'NONE',  ( 33.75396078491245078, 5.407089921784862696, 159.9599749780466027 ) ) ;
#20800 = CARTESIAN_POINT ( 'NONE',  ( 3.796722387233182339, 12.81481371789855217, 8.710071997420207879 ) ) ;
#20801 = CARTESIAN_POINT ( 'NONE',  ( -59.30580436395489841, 216.5000000000000000, 0.1155267958017343610 ) ) ;
#20802 = CARTESIAN_POINT ( 'NONE',  ( -66.03497103062157692, 202.6965474657331185, -4.350049139982091084 ) ) ;
#20803 = AXIS2_PLACEMENT_3D ( 'NONE', #20117, #31850, #2483 ) ;
#20804 = DIRECTION ( 'NONE',  ( 1.000000000000000000, 0.000000000000000000, 0.000000000000000000 ) ) ;
#20805 = CARTESIAN_POINT ( 'NONE',  ( 20.99999999999997868, 246.9625000000000057, 5.999999999999999112 ) ) ;
#20806 = CARTESIAN_POINT ( 'NONE',  ( 13.62178482187501416, 196.4093750006145456, 23.59362340125806767 ) ) ;
#20807 = CARTESIAN_POINT ( 'NONE',  ( -5.770363421894122880, 124.3648137178985849, 14.38691631536194393 ) ) ;
#20808 = CARTESIAN_POINT ( 'NONE',  ( -60.68377896937848703, 208.3738570449995109, 6.530955311639247363 ) ) ;
#20809 = ADVANCED_FACE ( 'NONE', ( #13070, #24809 ), #16480, .T. ) ;
#20810 = ORIENTED_EDGE ( 'NONE', *, *, #24434, .F. ) ;
#20811 = CARTESIAN_POINT ( 'NONE',  ( 2.660918448318279950, 42.89768628210143930, -12.46528703574805697 ) ) ;
#20812 = DIRECTION ( 'NONE',  ( -0.000000000000000000, -1.000000000000000000, -0.000000000000000000 ) ) ;
#20813 = CARTESIAN_POINT ( 'NONE',  ( 24.39973617568989184, 4.660121730947068386, -8.000000000000026645 ) ) ;
#20814 = CARTESIAN_POINT ( 'NONE',  ( 37.48811928047766884, 3.604726614523243278, 166.8231380282798568 ) ) ;
#20815 = CARTESIAN_POINT ( 'NONE',  ( 18.00000000000000355, -5.196152422706632912, -2.568749998770964105 ) ) ;
#20816 = CARTESIAN_POINT ( 'NONE',  ( -47.00000000000000711, 244.5000000000000000, 5.000000000000000000 ) ) ;
#20817 = CARTESIAN_POINT ( 'NONE',  ( 16.56230152254411436, -7.209453229046475009, -1.378124999385542226 ) ) ;
#20818 = CARTESIAN_POINT ( 'NONE',  ( -8.710071997420127943, 59.28518628210144925, -3.796722387233380402 ) ) ;
#20819 = DIRECTION ( 'NONE',  ( 0.000000000000000000, 0.000000000000000000, -1.000000000000000000 ) ) ;
#20820 = CARTESIAN_POINT ( 'NONE',  ( 22.60769515458672885, 245.6325961894323768, 5.999999999999997335 ) ) ;
#20821 = CIRCLE ( 'NONE', #4465, 25.00000000000000000 ) ;
#20822 = CARTESIAN_POINT ( 'NONE',  ( -0.1745138560725500443, 102.4101862821014493, 12.50000000000000355 ) ) ;
#20823 = CARTESIAN_POINT ( 'NONE',  ( 1.069080835302379631E-14, 199.3250000012290286, 27.00000000000000000 ) ) ;
#20824 = CARTESIAN_POINT ( 'NONE',  ( 20.99999999999999645, 185.0294372515228645, 0.000000000000000000 ) ) ;
#20825 = ORIENTED_EDGE ( 'NONE', *, *, #22396, .F. ) ;
#20826 = CARTESIAN_POINT ( 'NONE',  ( 24.40626844856526745, -3.604726614523240613, 160.5707542461117612 ) ) ;
#20827 = CARTESIAN_POINT ( 'NONE',  ( 18.12178482187500350, -4.985214923628407568, -9.515624999385464022 ) ) ;
#20828 = CARTESIAN_POINT ( 'NONE',  ( -27.00000000000000355, 195.5750000012290570, -15.58845726811989429 ) ) ;
#20829 = CARTESIAN_POINT ( 'NONE',  ( 24.82951852428355011, 0.000000000000000000, 165.4085247487197989 ) ) ;
#20830 = CARTESIAN_POINT ( 'NONE',  ( 28.08444087378459741, -5.196152422706638241, 165.3966694601965060 ) ) ;
#20831 = CARTESIAN_POINT ( 'NONE',  ( 26.99999999999999645, 7.347880794884117764E-16, -6.918749998770956644 ) ) ;
#20832 = CARTESIAN_POINT ( 'NONE',  ( 23.99999999999999645, 248.9500000000000171, -5.196152422706631135 ) ) ;
#20833 = CARTESIAN_POINT ( 'NONE',  ( -1.926257025242585782E-15, 195.1906250006145456, -31.45816453501076637 ) ) ;
#20834 = CARTESIAN_POINT ( 'NONE',  ( -8.715434833792127023, 97.33981371789855075, 8.962234695871568846 ) ) ;
#20835 = CARTESIAN_POINT ( 'NONE',  ( 0.1745138560725515708, 97.81018628210144072, -12.50000000000000355 ) ) ;
#20837 = ORIENTED_EDGE ( 'NONE', *, *, #6712, .T. ) ;
#20836 = ORIENTED_EDGE ( 'NONE', *, *, #35764, .T. ) ;
#20838 = CARTESIAN_POINT ( 'NONE',  ( 27.24356964374999635, 196.0156250006145626, -15.72908226750539029 ) ) ;
#20839 = CARTESIAN_POINT ( 'NONE',  ( 15.24356964374999990, 239.8468750006145171, 0.000000000000000000 ) ) ;
#20840 = CARTESIAN_POINT ( 'NONE',  ( -13.23911966647199812, 71.75231371789854506, -8.632099005475788900 ) ) ;
#20841 = CARTESIAN_POINT ( 'NONE',  ( 18.12178482187500350, -4.985214923628407568, -3.778124999385484628 ) ) ;
#20842 = CARTESIAN_POINT ( 'NONE',  ( 18.12178482187500350, 246.7843750006145456, 4.985214923628407568 ) ) ;
#20843 = CARTESIAN_POINT ( 'NONE',  ( -7.954856959092191815, 105.5726862821014294, -5.529263428287477744 ) ) ;
#20844 = AXIS2_PLACEMENT_3D ( 'NONE', #13171, #31900, #8235 ) ;
#20845 = PRODUCT_DEFINITION_FORMATION_WITH_SPECIFIED_SOURCE ( 'ANY', '', #2880, .NOT_KNOWN. ) ;
#20846 = CARTESIAN_POINT ( 'NONE',  ( 27.00000000000001066, 195.8000000012290513, 15.58845726811988897 ) ) ;
#20847 = CARTESIAN_POINT ( 'NONE',  ( 7.954856959092311719, 74.62731371789853085, -5.529263428287300108 ) ) ;
#20848 = CARTESIAN_POINT ( 'NONE',  ( 10.31873187879411269, 3.604726614523236616, -6.028124999385552130 ) ) ;
#20849 = EDGE_CURVE ( 'NONE', #27522, #23999, #32095, .T. ) ;
#20850 = CARTESIAN_POINT ( 'NONE',  ( 23.87821517812500005, 240.8968750006145285, 4.985214923628404016 ) ) ;
#20851 = CARTESIAN_POINT ( 'NONE',  ( 10.69584247140429589, 48.75231371789854506, 6.932735513424201024 ) ) ;
#20852 = EDGE_CURVE ( 'NONE', #17354, #25471, #25543, .T. ) ;
#20853 = CARTESIAN_POINT ( 'NONE',  ( 2.999999999999997335, 244.5000000000000000, 2.500000000000000000 ) ) ;
#20854 = CARTESIAN_POINT ( 'NONE',  ( 2.660918448318279950, 107.2976862821014521, -12.46528703574805697 ) ) ;
#20855 = CARTESIAN_POINT ( 'NONE',  ( 10.56230152254411614, -3.464101615137757051, -7.049999998771010468 ) ) ;
#20856 = EDGE_CURVE ( 'NONE', #4359, #6022, #8824, .T. ) ;
#20857 = CARTESIAN_POINT ( 'NONE',  ( -34.36830436395490551, 209.8844732041982581, 6.500000000000000888 ) ) ;
#20858 = CARTESIAN_POINT ( 'NONE',  ( 2.311890736173175753, 138.9226862821014663, 12.53471296425194836 ) ) ;
#20859 = CARTESIAN_POINT ( 'NONE',  ( 37.21194452064604974, -3.604726614523235284, 163.6664460787016253 ) ) ;
#20860 = CARTESIAN_POINT ( 'NONE',  ( 0.1745138560725837118, 88.61018628210146630, -15.50000000000000533 ) ) ;
#20861 = CARTESIAN_POINT ( 'NONE',  ( 10.31873187879411269, 3.604726614523240613, -4.284374999385515359 ) ) ;
#20862 =( LENGTH_UNIT ( ) NAMED_UNIT ( * ) SI_UNIT ( .MILLI., .METRE. ) );
#20863 = LINE ( 'NONE', #1123, #7364 ) ;
#20864 = CARTESIAN_POINT ( 'NONE',  ( 15.00000000000000000, 0.000000000000000000, -5.793749998770941545 ) ) ;
#20865 = CARTESIAN_POINT ( 'NONE',  ( 3.796722387233379514, 116.7851862821014635, -8.710071997420127943 ) ) ;
#20866 = CARTESIAN_POINT ( 'NONE',  ( 10.44051670066910908, 0.000000000000000000, -0.2671874990782807657 ) ) ;
#20867 = CARTESIAN_POINT ( 'NONE',  ( 15.53471296425195369, 7.822686282101448896, -2.908627838312120684 ) ) ;
#20868 = CARTESIAN_POINT ( 'NONE',  ( 27.24356964374999635, 196.5218750006145569, -15.72908226750539029 ) ) ;
#20869 = CARTESIAN_POINT ( 'NONE',  ( 15.24356964374999990, 241.1593750006145171, -3.323476615752268604 ) ) ;
#20870 = ORIENTED_EDGE ( 'NONE', *, *, #25320, .F. ) ;
#20871 = CARTESIAN_POINT ( 'NONE',  ( 37.37536153829788077, 3.604726614523238837, 165.5343111376236607 ) ) ;
#20872 = CARTESIAN_POINT ( 'NONE',  ( 26.75643035624999655, -3.323476615752267715, -2.203124999385475569 ) ) ;
#20873 = CARTESIAN_POINT ( 'NONE',  ( 27.24356964375000700, 199.1468750006145285, 15.72908226750537075 ) ) ;
#20874 = CARTESIAN_POINT ( 'NONE',  ( 18.00000000000000000, 5.196152422706630247, -3.675000000000011369 ) ) ;
#20875 = CARTESIAN_POINT ( 'NONE',  ( 19.56230152254410726, 5.196152422706631135, -5.887499998771001053 ) ) ;
#20876 = CARTESIAN_POINT ( 'NONE',  ( 37.05999817766988258, -3.464101615137495926, 164.7243396790029522 ) ) ;
#20877 = CARTESIAN_POINT ( 'NONE',  ( 27.00000000000000355, 198.8750000000000284, -3.306546357697854128E-15 ) ) ;
#20878 = CARTESIAN_POINT ( 'NONE',  ( 1.715153634034445762, 27.47731371789854649, -9.534712964251895073 ) ) ;
#20879 = CARTESIAN_POINT ( 'NONE',  ( 27.24356964374999279, 198.7718750006145569, -15.72908226750539207 ) ) ;
#20880 = ORIENTED_EDGE ( 'NONE', *, *, #15675, .T. ) ;
#20881 = CARTESIAN_POINT ( 'NONE',  ( 23.87821517812499650, 247.3468750006144887, -4.985214923628404904 ) ) ;
#20882 = CARTESIAN_POINT ( 'NONE',  ( -11.48171059495408208, 42.71481371789855075, 4.944772684328421875 ) ) ;
#20883 = CARTESIAN_POINT ( 'NONE',  ( 26.75643035624999655, 7.049594010296217766E-16, -1.715624999385462202 ) ) ;
#20884 = CARTESIAN_POINT ( 'NONE',  ( -5.770363421894122880, 133.5648137178985735, 14.38691631536194393 ) ) ;
#20885 = CARTESIAN_POINT ( 'NONE',  ( 15.00000000000000178, -3.464101615137757051, -7.556249998770954157 ) ) ;
#20886 = ORIENTED_EDGE ( 'NONE', *, *, #31697, .T. ) ;
#20887 = CARTESIAN_POINT ( 'NONE',  ( 10.31873187879410736, 0.000000000000000000, -3.346874999385518468 ) ) ;
#20888 = CARTESIAN_POINT ( 'NONE',  ( -13.62178482187500528, 199.7281250006145399, -23.59362340125807123 ) ) ;
#20889 = CARTESIAN_POINT ( 'NONE',  ( 34.14616162727688931, 5.407089921784862696, 164.4428511194594478 ) ) ;
#20890 = CARTESIAN_POINT ( 'NONE',  ( -64.64211230271182274, 201.5309553116392181, 2.393094931466368980 ) ) ;
#20891 = CARTESIAN_POINT ( 'NONE',  ( 18.12178482187500350, 248.4718750006145171, 4.985214923628407568 ) ) ;
#20892 = DIRECTION ( 'NONE',  ( -1.000000000000000000, 0.000000000000000000, 1.636531581110199847E-16 ) ) ;
#20893 = CARTESIAN_POINT ( 'NONE',  ( -63.65252896937850124, 207.6499508600178387, -3.839350919129087547 ) ) ;
#20894 = VECTOR ( 'NONE', #3653, 1000.000000000000000 ) ;
#20895 = CARTESIAN_POINT ( 'NONE',  ( 37.03058311459962937, -3.464101615137506140, 164.3881239696213754 ) ) ;
#20896 = CARTESIAN_POINT ( 'NONE',  ( 31.26013745332475224, -7.209453229046475009, 167.2739077250314779 ) ) ;
#20897 = ORIENTED_EDGE ( 'NONE', *, *, #25595, .T. ) ;
#20898 = AXIS2_PLACEMENT_3D ( 'NONE', #25934, #36744, #10784 ) ;
#20899 = DIRECTION ( 'NONE',  ( 0.000000000000000000, 0.000000000000000000, 1.000000000000000000 ) ) ;
#20900 = CARTESIAN_POINT ( 'NONE',  ( -3.257655550457281723, 139.4976862821014549, 15.46528703574804986 ) ) ;
#20901 = CARTESIAN_POINT ( 'NONE',  ( -62.27455436395490551, 203.6929966515020283, 6.137860380172978303 ) ) ;
#20902 = CARTESIAN_POINT ( 'NONE',  ( 8.710071997420127943, 137.4851862821014379, 3.796722387233375073 ) ) ;
#20903 =( BOUNDED_CURVE ( )  B_SPLINE_CURVE ( 2, ( #36967, #1544, #7617, #13116, #31656, #2655, #26335 ),
 .UNSPECIFIED., .F., .F. ) 
 B_SPLINE_CURVE_WITH_KNOTS ( ( 3, 2, 2, 3 ),
 ( 0.1956521739130434034, 0.2028985507246377218, 0.2101449275362319846, 0.2173913043478263030 ),
 .UNSPECIFIED. ) 
 CURVE ( )  GEOMETRIC_REPRESENTATION_ITEM ( )  RATIONAL_B_SPLINE_CURVE ( ( 1.000000000000001554, 0.8660254037844372643, 1.000000000000000000, 0.8660254037844387076, 1.000000000000000000, 0.8660254037844345998, 1.000000000000003997 ) ) 
 REPRESENTATION_ITEM ( '' )  );
#20904 = DIRECTION ( 'NONE',  ( -0.000000000000000000, -1.000000000000000000, -0.000000000000000000 ) ) ;
#20905 = CARTESIAN_POINT ( 'NONE',  ( 6.932735513423970097, 27.94768628210143646, 10.69584247140445044 ) ) ;
#20907 = EDGE_CURVE ( 'NONE', #32162, #5775, #37107, .T. ) ;
#20906 = CARTESIAN_POINT ( 'NONE',  ( 19.56230152254412502, 5.196152422706637353, -6.450000000000039257 ) ) ;
#20908 = EDGE_LOOP ( 'NONE', ( #31354, #20836, #30971, #14767 ) ) ;
#20909 = SURFACE_SIDE_STYLE ('',( #33210 ) ) ;
#20910 = CARTESIAN_POINT ( 'NONE',  ( -0.1745138560725817967, 120.8101862821014691, 15.50000000000000533 ) ) ;
#20911 = DIRECTION ( 'NONE',  ( 0.000000000000000000, 0.000000000000000000, 1.000000000000000000 ) ) ;
#20912 = CARTESIAN_POINT ( 'NONE',  ( -5.529263428287477744, 11.27268628210142865, 7.954856959092191815 ) ) ;
#20913 = CARTESIAN_POINT ( 'NONE',  ( 13.62178482187499640, 197.8531250006145399, -23.59362340125807123 ) ) ;
#20914 = CARTESIAN_POINT ( 'NONE',  ( 27.00000000000001421, 195.8000000012290513, 15.58845726811988897 ) ) ;
#20915 = CARTESIAN_POINT ( 'NONE',  ( 18.47613065999978232, -5.877663906574049690, -10.00000000000000178 ) ) ;
#20916 = LINE ( 'NONE', #20720, #28542 ) ;
#20917 = CARTESIAN_POINT ( 'NONE',  ( 30.65467740297821919, -6.928203230275506996, 160.3534676823375378 ) ) ;
#20918 = CARTESIAN_POINT ( 'NONE',  ( 26.75643035624999655, 243.7843750006145456, -7.049594010296217766E-16 ) ) ;
#20919 = CARTESIAN_POINT ( 'NONE',  ( -2.064181346179062349, 82.10231371789853938, -9.465287035748106703 ) ) ;
#20920 = CARTESIAN_POINT ( 'NONE',  ( 19.00081571707366379, 239.8729221881839067, -5.492723647597353320 ) ) ;
#20921 = VERTEX_POINT ( 'NONE', #2429 ) ;
#20922 = CARTESIAN_POINT ( 'NONE',  ( 26.99999999999999645, 245.3312500012290513, -7.347880794884117764E-16 ) ) ;
#20923 = CARTESIAN_POINT ( 'NONE',  ( -8.962234695871565293, 90.43981371789855928, -8.715434833792128799 ) ) ;
#20924 = CARTESIAN_POINT ( 'NONE',  ( 16.56230152254411436, 7.209453229046482114, -3.009374999385522553 ) ) ;
#20925 = CARTESIAN_POINT ( 'NONE',  ( 1.069080835302379631E-14, 197.9750000012290343, 27.00000000000000000 ) ) ;
#20926 = CARTESIAN_POINT ( 'NONE',  ( 21.00000000000000000, 6.646953231504538984, -4.865624999385484983 ) ) ;
#20927 = CARTESIAN_POINT ( 'NONE',  ( -6.932735513424201912, 60.25231371789855217, 10.69584247140429412 ) ) ;
#20928 = CARTESIAN_POINT ( 'NONE',  ( 27.24356964375000345, 197.8343750006145569, -3.336375036156643733E-15 ) ) ;
#20929 = EDGE_CURVE ( 'NONE', #31515, #20196, #34637, .T. ) ;
#20930 = AXIS2_PLACEMENT_3D ( 'NONE', #19822, #37035, #33837 ) ;
#20931 = VERTEX_POINT ( 'NONE', #22538 ) ;
#20932 =( BOUNDED_CURVE ( )  B_SPLINE_CURVE ( 2, ( #7875, #5017, #2549, #19448, #22467, #28141, #10895 ),
 .UNSPECIFIED., .F., .F. ) 
 B_SPLINE_CURVE_WITH_KNOTS ( ( 3, 2, 2, 3 ),
 ( 0.4130434782608670141, 0.4202898550724613047, 0.4275362318840557063, 0.4347826086956499969 ),
 .UNSPECIFIED. ) 
 CURVE ( )  GEOMETRIC_REPRESENTATION_ITEM ( )  RATIONAL_B_SPLINE_CURVE ( ( 1.000000000000047296, 0.8660254037843915231, 1.000000000000000000, 0.8660254037844387076, 1.000000000000000000, 0.8660254037844787867, 0.9999999999999599209 ) ) 
 REPRESENTATION_ITEM ( '' )  );
#20933 = EDGE_CURVE ( 'NONE', #33922, #16460, #11155, .T. ) ;
#20934 = ORIENTED_EDGE ( 'NONE', *, *, #35322, .T. ) ;
#20935 = CARTESIAN_POINT ( 'NONE',  ( 15.24356964375000167, -3.323476615752272600, -5.053124999385469884 ) ) ;
#20936 = CARTESIAN_POINT ( 'NONE',  ( 13.56230152254410548, 5.196152422706630247, -6.262499998771015264 ) ) ;
#20937 = CARTESIAN_POINT ( 'NONE',  ( 26.75643035624999655, 247.3093750006144944, -3.323476615752271712 ) ) ;
#20938 = CARTESIAN_POINT ( 'NONE',  ( -11.61527771782819940, 48.93518628210144783, 4.622313124798574258 ) ) ;
#20939 = CARTESIAN_POINT ( 'NONE',  ( -39.90252896937850124, 206.6499508600178387, -5.571401726697954970 ) ) ;
#20940 = DIRECTION ( 'NONE',  ( 0.000000000000000000, 0.000000000000000000, 1.000000000000000000 ) ) ;
#20941 = CARTESIAN_POINT ( 'NONE',  ( -65.63169563604516554, 210.1155267958017703, 6.500000000000000888 ) ) ;
#20942 =( NAMED_UNIT ( * ) PLANE_ANGLE_UNIT ( ) SI_UNIT ( $, .RADIAN. ) );
#20943 = CARTESIAN_POINT ( 'NONE',  ( 36.67760235647121903, -3.464101615137751278, 160.3535354423498234 ) ) ;
#20944 = CARTESIAN_POINT ( 'NONE',  ( -7.228626920338836470, 81.52731371789855075, -10.49813415416005213 ) ) ;
#20945 = CARTESIAN_POINT ( 'NONE',  ( -58.90997103062156981, 213.8393509191290889, 2.350049139982164359 ) ) ;
#20946 = CARTESIAN_POINT ( 'NONE',  ( -67.61830436395489130, 209.8844732041982581, 6.500000000000000888 ) ) ;
#20947 = CARTESIAN_POINT ( 'NONE',  ( 15.24356964374999990, 0.000000000000000000, -7.903124999385474858 ) ) ;
#20948 = DIRECTION ( 'NONE',  ( 0.000000000000000000, 0.000000000000000000, -1.000000000000000000 ) ) ;
#20949 = CARTESIAN_POINT ( 'NONE',  ( 6.092822981423662299, 58.81481371789855217, 14.25334919248795096 ) ) ;
#20950 = CARTESIAN_POINT ( 'NONE',  ( -64.44419563604517975, 201.5000000000000000, 0.1155267958018195706 ) ) ;
#20951 = CARTESIAN_POINT ( 'NONE',  ( 20.99999999999995381, 244.7125000000000057, 5.999999999999998224 ) ) ;
#20952 = CARTESIAN_POINT ( 'NONE',  ( -12.50000000000000355, 77.11018628210145209, -0.1745138560725492671 ) ) ;
#20953 = CARTESIAN_POINT ( 'NONE',  ( -14.38691631536207183, 39.73518628210145209, 5.770363421893814682 ) ) ;
#20954 = EDGE_CURVE ( 'NONE', #2700, #32942, #17584, .T. ) ;
#20955 = VECTOR ( 'NONE', #33036, 1000.000000000000000 ) ;
#20956 = DIRECTION ( 'NONE',  ( 0.000000000000000000, 0.000000000000000000, 1.000000000000000000 ) ) ;
#20957 = CARTESIAN_POINT ( 'NONE',  ( 27.47531968228746990, -5.407089921784865361, 159.8317065065323845 ) ) ;
#20958 = CARTESIAN_POINT ( 'NONE',  ( 8.632099005475504683, 55.54768628210144499, 13.23911966647218996 ) ) ;
#20959 = CARTESIAN_POINT ( 'NONE',  ( -1.045839947578415010E-13, 194.8250000012290570, 27.00000000000000355 ) ) ;
#20960 = CARTESIAN_POINT ( 'NONE',  ( 22.80587116629411071, -3.604726614523235284, -8.503124999385544669 ) ) ;
#20961 = CARTESIAN_POINT ( 'NONE',  ( 20.99999999999999645, -6.928203230275506996, -2.081249998770946963 ) ) ;
#20962 = CARTESIAN_POINT ( 'NONE',  ( -55.34747103062156981, 213.3500491399821328, -5.571401726697985168 ) ) ;
#20963 = CARTESIAN_POINT ( 'NONE',  ( 34.35575969410840003, 5.196152422706637353, 168.2358921097703046 ) ) ;
#20964 = CARTESIAN_POINT ( 'NONE',  ( -8.962234695871760692, 29.96018628210143930, 8.715434833791933400 ) ) ;
#20965 = CARTESIAN_POINT ( 'NONE',  ( 20.99999999999997868, 210.0000000000000000, -5.999999999999999112 ) ) ;
#20966 = CARTESIAN_POINT ( 'NONE',  ( 8.152565276336593669, 140.7523137178985166, 5.233372021372610483 ) ) ;
#20967 = CARTESIAN_POINT ( 'NONE',  ( 15.24356964374999990, 247.1593750006145171, 0.000000000000000000 ) ) ;
#20968 = EDGE_LOOP ( 'NONE', ( #7620, #23337 ) ) ;
#20969 = CARTESIAN_POINT ( 'NONE',  ( 18.00000000000000355, -5.196152422706632912, -6.225000000000008527 ) ) ;
#20970 =( BOUNDED_CURVE ( )  B_SPLINE_CURVE ( 2, ( #23330, #18402, #20874, #3609, #29379, #20496, #32413 ),
 .UNSPECIFIED., .F., .F. ) 
 B_SPLINE_CURVE_WITH_KNOTS ( ( 3, 2, 2, 3 ),
 ( 0.3478260869565210078, 0.3550724637681153539, 0.3623188405797096445, 0.3695652173913039351 ),
 .UNSPECIFIED. ) 
 CURVE ( )  GEOMETRIC_REPRESENTATION_ITEM ( )  RATIONAL_B_SPLINE_CURVE ( ( 1.000000000000013323, 0.8660254037844252739, 1.000000000000000000, 0.8660254037844387076, 1.000000000000000000, 0.8660254037844459241, 0.9999999999999927836 ) ) 
 REPRESENTATION_ITEM ( '' )  );
#20971 = FACE_OUTER_BOUND ( 'NONE', #24206, .T. ) ;
#20972 = VECTOR ( 'NONE', #33980, 1000.000000000000000 ) ;
#20973 = CARTESIAN_POINT ( 'NONE',  ( 10.31873187879410736, 0.000000000000000000, -4.190624999385549998 ) ) ;
#20974 = CARTESIAN_POINT ( 'NONE',  ( 24.94881294716939379, 3.604726614523236616, 166.7720662417328299 ) ) ;
#20975 = CARTESIAN_POINT ( 'NONE',  ( 26.99999999999999645, 242.0875000000000057, 3.464101615137751278 ) ) ;
#20976 = EDGE_CURVE ( 'NONE', #33186, #19052, #25317, .T. ) ;
#20977 = CARTESIAN_POINT ( 'NONE',  ( -12.46528703574805874, 40.59768628210144925, -2.660918448318280838 ) ) ;
#20978 = ORIENTED_EDGE ( 'NONE', *, *, #15002, .F. ) ;
#20979 = ORIENTED_EDGE ( 'NONE', *, *, #16382, .T. ) ;
#20980 = CARTESIAN_POINT ( 'NONE',  ( -26.99999999999999645, 195.9875000000000114, 15.58845726811991561 ) ) ;
#20981 = CARTESIAN_POINT ( 'NONE',  ( 13.56230152254411436, -5.196152422706632912, -2.062499998771005760 ) ) ;
#20982 = DIRECTION ( 'NONE',  ( -0.000000000000000000, -0.000000000000000000, 1.000000000000000000 ) ) ;
#20983 = CARTESIAN_POINT ( 'NONE',  ( 27.77068019989305370, -5.196152422706638241, 161.8103685470662469 ) ) ;
#20984 = CARTESIAN_POINT ( 'NONE',  ( 18.12178482187499640, 4.985214923628404904, -6.965624999385466865 ) ) ;
#20985 = CARTESIAN_POINT ( 'NONE',  ( 11.48171059495397728, 100.6851862821014691, 4.944772684328674117 ) ) ;
#20986 = CARTESIAN_POINT ( 'NONE',  ( 15.46528703574811736, 29.20231371789855501, -3.257655550456947768 ) ) ;
#20987 = CARTESIAN_POINT ( 'NONE',  ( 23.99999999999999645, 249.4000000000000057, -5.196152422706631135 ) ) ;
#20988 = CARTESIAN_POINT ( 'NONE',  ( 37.14170668649535401, 7.347880794884125653E-16, 165.6582722084640125 ) ) ;
#20989 = CARTESIAN_POINT ( 'NONE',  ( -37.53497103062155560, 206.1606490808709111, -2.350049139982163027 ) ) ;
#20990 = CARTESIAN_POINT ( 'NONE',  ( -9.000000000000024869, 204.5000000000000000, 0.000000000000000000 ) ) ;
#20991 = CARTESIAN_POINT ( 'NONE',  ( 33.71474070067601048, 5.407089921784862696, 159.5116873639053097 ) ) ;
#20992 = CARTESIAN_POINT ( 'NONE',  ( 12.53471296425189330, 140.1773137178985849, 2.311890736173451977 ) ) ;
#20993 = CARTESIAN_POINT ( 'NONE',  ( -59.50372103062156981, 216.5309553116391612, -1.626142955000564383 ) ) ;
#20994 = CARTESIAN_POINT ( 'NONE',  ( -33.56919563604517265, 218.5000000000000000, -0.1155267958018185298 ) ) ;
#20995 = APPLICATION_PROTOCOL_DEFINITION ( 'draft international standard', 'automotive_design', 1998, #26974 ) ;
#20996 = DIRECTION ( 'NONE',  ( 1.000000000000000000, 0.000000000000000000, 0.000000000000000000 ) ) ;
#20997 = CARTESIAN_POINT ( 'NONE',  ( 13.62178482187501416, 198.1531250006145228, 23.59362340125806767 ) ) ;
#20998 = CARTESIAN_POINT ( 'NONE',  ( -0.1745138560722442889, 119.1898137178985593, -15.50000000000000533 ) ) ;
#20999 = CARTESIAN_POINT ( 'NONE',  ( -61.87127896937849414, 216.5309553116391612, 1.626142955000506873 ) ) ;
#21000 = AXIS2_PLACEMENT_3D ( 'NONE', #5621, #19874, #14171 ) ;
#21001 = EDGE_CURVE ( 'NONE', #36330, #32727, #19150, .T. ) ;
#21002 = ORIENTED_EDGE ( 'NONE', *, *, #2188, .F. ) ;
#21003 = CARTESIAN_POINT ( 'NONE',  ( -7.228626920339069173, 38.87268628210144072, 10.49813415415989581 ) ) ;
#21004 = CARTESIAN_POINT ( 'NONE',  ( 24.00000000000000000, -5.196152422706629359, -6.149999999999988809 ) ) ;
#21005 = CARTESIAN_POINT ( 'NONE',  ( 27.00000000000000355, 198.8750000000000284, -3.306546357697854128E-15 ) ) ;
#21006 = CARTESIAN_POINT ( 'NONE',  ( 37.37045902776835504, 3.604726614523243278, 165.4782751858559777 ) ) ;
#21007 = CARTESIAN_POINT ( 'NONE',  ( 15.46528703574804986, 109.5976862821014493, 3.257655550457285720 ) ) ;
#21008 = CARTESIAN_POINT ( 'NONE',  ( -63.26413769728824121, 213.1499508600178672, 5.686928522499718142 ) ) ;
#21009 = CARTESIAN_POINT ( 'NONE',  ( 10.31873187879411091, 3.604726614523236616, -1.078124999385534410 ) ) ;
#21010 = CARTESIAN_POINT ( 'NONE',  ( -0.1745138560725182642, 56.41018628210145636, 9.500000000000005329 ) ) ;
#21011 = CARTESIAN_POINT ( 'NONE',  ( -77.00000000000002842, 210.0000000000000000, 5.000000000000000000 ) ) ;
#21012 = DIRECTION ( 'NONE',  ( -1.000000000000000000, 0.000000000000000000, 0.000000000000000000 ) ) ;
#21013 = CARTESIAN_POINT ( 'NONE',  ( 8.715434833791931624, 82.86018628210145209, 8.962234695871760692 ) ) ;
#21014 = CARTESIAN_POINT ( 'NONE',  ( 9.184850993605147944E-16, 148.0000000000000000, -7.500000000000000000 ) ) ;
#21015 = DIRECTION ( 'NONE',  ( 0.000000000000000000, 1.000000000000000000, 0.000000000000000000 ) ) ;
#21016 = ORIENTED_EDGE ( 'NONE', *, *, #6300, .T. ) ;
#21017 = CARTESIAN_POINT ( 'NONE',  ( 36.82628035898768815, 3.604726614523238837, 159.2582845396456719 ) ) ;
#21018 = CARTESIAN_POINT ( 'NONE',  ( 26.75643035624999655, -3.323476615752267715, -9.403124999385470417 ) ) ;
#21019 = CARTESIAN_POINT ( 'NONE',  ( -44.35000000000002274, 244.5000000000000000, 5.000000000000000888 ) ) ;
#21020 = CARTESIAN_POINT ( 'NONE',  ( 24.86873860851999041, 0.000000000000000000, 165.8568123628610920 ) ) ;
#21021 = PRODUCT_DEFINITION_CONTEXT ( 'detailed design', #21182, 'design' ) ;
#21022 = CARTESIAN_POINT ( 'NONE',  ( 27.95370725966311554, 5.196152422706636465, 163.9023774130589288 ) ) ;
#21023 = CARTESIAN_POINT ( 'NONE',  ( 6.123233995736767268E-16, 148.0000000000000000, 5.000000000000000888 ) ) ;
#21024 = CARTESIAN_POINT ( 'NONE',  ( 26.99999999999999645, 247.4875000000000398, 3.464101615137751278 ) ) ;
#21025 = CARTESIAN_POINT ( 'NONE',  ( -13.62178482187498396, 197.1781250006145569, 23.59362340125808188 ) ) ;
#21026 = CARTESIAN_POINT ( 'NONE',  ( 12.50000000000000355, 112.2898137178985678, -0.1745138560722771515 ) ) ;
#21027 = CARTESIAN_POINT ( 'NONE',  ( -11.61527771782819940, 104.1351862821014578, 4.622313124798574258 ) ) ;
#21028 = ORIENTED_EDGE ( 'NONE', *, *, #1566, .T. ) ;
#21029 = CARTESIAN_POINT ( 'NONE',  ( 27.24356964375000345, 196.8781250006145171, -3.336375036156643733E-15 ) ) ;
#21030 = CARTESIAN_POINT ( 'NONE',  ( 20.99999999999999645, 185.0294372515228645, 0.000000000000000000 ) ) ;
#21031 = CARTESIAN_POINT ( 'NONE',  ( 8.927990412390371944, 67.72731371789853938, 13.04141134922778811 ) ) ;
#21032 = CARTESIAN_POINT ( 'NONE',  ( 18.12178482187499640, 4.985214923628404904, -3.478124999385490135 ) ) ;
#21033 = CARTESIAN_POINT ( 'NONE',  ( 21.00000000000000000, 247.7218750006145171, 6.646953231504538984 ) ) ;
#21034 = CARTESIAN_POINT ( 'NONE',  ( -3.474262827703337830, 106.4351862821014691, -8.843639120294326972 ) ) ;
#21035 = ADVANCED_BREP_SHAPE_REPRESENTATION ( '', ( #33379, #17215 ), #29865 ) ;
#21036 = CARTESIAN_POINT ( 'NONE',  ( -13.49999999999998401, 194.7875000012290343, 23.38268590217985476 ) ) ;
#21037 = CARTESIAN_POINT ( 'NONE',  ( 5.529263428287300108, 58.52731371789855785, 7.954856959092309943 ) ) ;
#21038 = CARTESIAN_POINT ( 'NONE',  ( 19.68408634441910365, -5.407089921784855591, -5.840624999385535254 ) ) ;
#21039 = CARTESIAN_POINT ( 'NONE',  ( -3.796722387233185003, 109.4148137178985536, -8.710071997420207879 ) ) ;
#21040 = CARTESIAN_POINT ( 'NONE',  ( -27.24356964375000345, 199.8593750006145342, 0.000000000000000000 ) ) ;
#21041 = CARTESIAN_POINT ( 'NONE',  ( -4.622313124798826500, 50.76481371789855501, 11.61527771782809637 ) ) ;
#21042 = CARTESIAN_POINT ( 'NONE',  ( -81.72704584564827712, 216.6260876520869658, 5.000000000000000000 ) ) ;
#21043 = CARTESIAN_POINT ( 'NONE',  ( 12.50000000000000355, 109.3101862821014549, 0.1745138560725507937 ) ) ;
#21044 = CARTESIAN_POINT ( 'NONE',  ( 19.56230152254411081, 5.196152422706631135, -5.437499998771022192 ) ) ;
#21045 = CARTESIAN_POINT ( 'NONE',  ( -33.18080436395490551, 203.5000000000000000, -0.1155267958017335561 ) ) ;
#21046 = CARTESIAN_POINT ( 'NONE',  ( -8.715434833791929847, 133.4601862821014606, -8.962234695871762469 ) ) ;
#21047 = CARTESIAN_POINT ( 'NONE',  ( 31.02481694790609268, -7.209453229046475009, 164.5841820401837765 ) ) ;
#21048 = CARTESIAN_POINT ( 'NONE',  ( -15.53471296425195369, 86.02268628210144641, 2.908627838312118019 ) ) ;
#21049 = AXIS2_PLACEMENT_3D ( 'NONE', #20824, #3562, #28956 ) ;
#21050 = CARTESIAN_POINT ( 'NONE',  ( 10.31873187879410558, 3.604726614523240613, -2.934374999385496618 ) ) ;
#21051 = SURFACE_SIDE_STYLE ('',( #18389 ) ) ;
#21052 = CARTESIAN_POINT ( 'NONE',  ( 26.99999999999999645, 7.347880794884117764E-16, -7.368749998770962151 ) ) ;
#21053 = CARTESIAN_POINT ( 'NONE',  ( 29.48995970988985604, 6.148715791637016537, 159.4803054849043917 ) ) ;
#21054 = CARTESIAN_POINT ( 'NONE',  ( -2.064181346179269738, 121.0976862821014635, 9.465287035748067623 ) ) ;
#21055 = CARTESIAN_POINT ( 'NONE',  ( 20.99999999999999645, 6.928203230275506996, -2.306249998770960818 ) ) ;
#21056 = CARTESIAN_POINT ( 'NONE',  ( -8.632099005475501130, 4.947686282101431132, -13.23911966647218996 ) ) ;
#21057 = CARTESIAN_POINT ( 'NONE',  ( 27.24356964375000700, 195.0968750006145456, 15.72908226750537075 ) ) ;
#21058 = CARTESIAN_POINT ( 'NONE',  ( 21.00000000000000000, 242.6593750006145171, 6.646953231504538984 ) ) ;
#21059 = ORIENTED_EDGE ( 'NONE', *, *, #21920, .T. ) ;
#21060 = CARTESIAN_POINT ( 'NONE',  ( 34.42560472746153977, 5.407089921784857367, 167.6369003702161251 ) ) ;
#21061 = CARTESIAN_POINT ( 'NONE',  ( 21.00000000000000000, -6.646953231504538984, -2.728124999385465266 ) ) ;
#21063 = EDGE_CURVE ( 'NONE', #16244, #35488, #3502, .T. ) ;
#21062 = CARTESIAN_POINT ( 'NONE',  ( 13.56230152254411792, -5.196152422706638241, -4.875000000000101252 ) ) ;
#21064 = CARTESIAN_POINT ( 'NONE',  ( 24.90302469878729141, 0.000000000000000000, 163.4540559201358576 ) ) ;
#21065 = LINE ( 'NONE', #29758, #24541 ) ;
#21066 = CARTESIAN_POINT ( 'NONE',  ( 26.99999999999999645, 7.347880794884117764E-16, -7.368749998770962151 ) ) ;
#21067 = CYLINDRICAL_SURFACE ( 'NONE', #11524, 6.000000000000001776 ) ;
#21068 = CARTESIAN_POINT ( 'NONE',  ( 9.465287035748106703, 20.00231371789855217, -2.064181346179063237 ) ) ;
#21069 = CARTESIAN_POINT ( 'NONE',  ( 13.62178482187501416, 197.7593750006145399, 23.59362340125806767 ) ) ;
#21071 = VERTEX_POINT ( 'NONE', #34275 ) ;
#21070 = VERTEX_POINT ( 'NONE', #31794 ) ;
#21072 = CARTESIAN_POINT ( 'NONE',  ( 18.12178482187499640, 246.0718750006145115, -4.985214923628404904 ) ) ;
#21073 = CARTESIAN_POINT ( 'NONE',  ( 8.715434833792128799, 19.13981371789855146, -8.962234695871567070 ) ) ;
#21074 = ADVANCED_FACE ( 'NONE', ( #26110 ), #2243, .T. ) ;
#21075 = CARTESIAN_POINT ( 'NONE',  ( 15.24356964374999990, 0.000000000000000000, -0.5906249993854750802 ) ) ;
#21076 = CARTESIAN_POINT ( 'NONE',  ( 5.770363421894130873, 138.1648137178985678, -14.38691631536193860 ) ) ;
#21077 = ADVANCED_FACE ( 'NONE', ( #19707 ), #25369, .F. ) ;
#21078 = CARTESIAN_POINT ( 'NONE',  ( 15.00000000000000000, 3.464101615137752166, -8.081249998770942966 ) ) ;
#21079 = CARTESIAN_POINT ( 'NONE',  ( -7.234628195640313564, 199.5700961906613884, -27.00000000000000355 ) ) ;
#21080 = ORIENTED_EDGE ( 'NONE', *, *, #2868, .F. ) ;
#21081 = CARTESIAN_POINT ( 'NONE',  ( 22.80587116629411426, 3.604726614523243278, -7.134374999385543425 ) ) ;
#21082 = VECTOR ( 'NONE', #8080, 1000.000000000000000 ) ;
#21083 = CARTESIAN_POINT ( 'NONE',  ( 13.62178482187499640, 197.4031250006145228, -23.59362340125807123 ) ) ;
#21084 = CARTESIAN_POINT ( 'NONE',  ( 24.82625018393050809, 3.604726614523240613, 165.3711674475413531 ) ) ;
#21085 = CARTESIAN_POINT ( 'NONE',  ( -62.46502896937850124, 217.3034525342667962, -4.350049139982195001 ) ) ;
#21086 = CARTESIAN_POINT ( 'NONE',  ( 23.87821517812499650, 249.5968750006145171, -4.985214923628404904 ) ) ;
#21087 = CARTESIAN_POINT ( 'NONE',  ( -39.50669563604516554, 209.8844732041982297, -4.499999999999996447 ) ) ;
#21088 = PLANE ( 'NONE',  #30876 ) ;
#21089 = CARTESIAN_POINT ( 'NONE',  ( 25.06974154023176382, 0.000000000000000000, 168.1542863853351548 ) ) ;
#21090 = ORIENTED_EDGE ( 'NONE', *, *, #15688, .T. ) ;
#21091 = CARTESIAN_POINT ( 'NONE',  ( -28.16023620420738993, 205.9774825840613346, 6.934657662760876917 ) ) ;
#21092 = CARTESIAN_POINT ( 'NONE',  ( -15.53471296425195369, 141.2226862821014493, 2.908627838312118019 ) ) ;
#21093 = CARTESIAN_POINT ( 'NONE',  ( -45.25372103062157692, 218.5309553116391896, -2.162041339862839084 ) ) ;
#21094 = CARTESIAN_POINT ( 'NONE',  ( -3.474262827703337830, 124.8351862821014748, -8.843639120294326972 ) ) ;
#21095 = DIRECTION ( 'NONE',  ( 0.000000000000000000, 1.000000000000000000, 0.000000000000000000 ) ) ;
#21096 = CARTESIAN_POINT ( 'NONE',  ( 4.944772684328679446, 24.78518628210143859, -11.48171059495397373 ) ) ;
#21097 = CARTESIAN_POINT ( 'NONE',  ( 19.56230152254412502, -5.196152422706635576, -7.050000000000084199 ) ) ;
#21098 = CLOSED_SHELL ( 'NONE', ( #14013, #12372, #28018, #2231, #11259 ) ) ;
#21099 = AXIS2_PLACEMENT_3D ( 'NONE', #29461, #17358, #26238 ) ;
#21100 = ORIENTED_EDGE ( 'NONE', *, *, #4954, .T. ) ;
#21101 = CARTESIAN_POINT ( 'NONE',  ( -34.36830436395490551, 209.8844732041982581, 6.500000000000000888 ) ) ;
#21102 = CARTESIAN_POINT ( 'NONE',  ( -6.092822981423970496, 121.3851862821014578, 14.25334919248782661 ) ) ;
#21103 = DIRECTION ( 'NONE',  ( 0.000000000000000000, -0.000000000000000000, 1.000000000000000000 ) ) ;
#21104 = CARTESIAN_POINT ( 'NONE',  ( 8.152565276336714462, 7.247686282101430066, -5.233372021372432847 ) ) ;
#21105 = CARTESIAN_POINT ( 'NONE',  ( 27.24356964375000345, 197.7781250006145228, -3.336375036156643733E-15 ) ) ;
#21106 = CARTESIAN_POINT ( 'NONE',  ( 27.00000000000001421, 198.0500000012290513, 15.58845726811988897 ) ) ;
#21107 = CARTESIAN_POINT ( 'NONE',  ( 13.56230152254410903, 5.196152422706636465, -5.475000000000035172 ) ) ;
#21108 = CARTESIAN_POINT ( 'NONE',  ( 15.09967099808794266, 0.4797207149645432156, -8.000000000000000000 ) ) ;
#21109 = LINE ( 'NONE', #32648, #14534 ) ;
#21110 = CARTESIAN_POINT ( 'NONE',  ( 3.796722387233182339, 68.01481371789854791, 8.710071997420207879 ) ) ;
#21111 = CARTESIAN_POINT ( 'NONE',  ( 0.000000000000000000, 210.0000000000000284, -27.00000000000000000 ) ) ;
#21112 = VERTEX_POINT ( 'NONE', #16855 ) ;
#21113 = CARTESIAN_POINT ( 'NONE',  ( 15.00000000000000000, 243.2687500012290229, -3.464101615137752166 ) ) ;
#21114 = CARTESIAN_POINT ( 'NONE',  ( 10.69584247140429589, 85.55231371789857064, 6.932735513424201024 ) ) ;
#21115 = CARTESIAN_POINT ( 'NONE',  ( 16.56230152254411436, -7.209453229046482114, -4.584374999385491201 ) ) ;
#21116 = CARTESIAN_POINT ( 'NONE',  ( 19.39230484541324273, 242.8924038105677141, 5.999999999999987566 ) ) ;
#21117 = CARTESIAN_POINT ( 'NONE',  ( 15.24356964374999990, 3.323476615752268604, -4.790624999385491023 ) ) ;
#21118 = CARTESIAN_POINT ( 'NONE',  ( -12.50000000000000355, 43.28981371789855359, 0.1745138560722786503 ) ) ;
#21119 = CARTESIAN_POINT ( 'NONE',  ( -27.24356964375000345, 197.6093750006145342, 0.000000000000000000 ) ) ;
#21120 = ORIENTED_EDGE ( 'NONE', *, *, #10140, .F. ) ;
#21121 = ORIENTED_EDGE ( 'NONE', *, *, #36787, .T. ) ;
#21122 = CARTESIAN_POINT ( 'NONE',  ( 18.12178482187499640, 4.985214923628404904, -5.165624999385470595 ) ) ;
#21123 = CARTESIAN_POINT ( 'NONE',  ( 15.24356964374999990, 244.7968750006145058, 0.000000000000000000 ) ) ;
#21124 = CARTESIAN_POINT ( 'NONE',  ( 11.61527771782819940, 44.33518628210145351, -4.622313124798573369 ) ) ;
#21125 = CARTESIAN_POINT ( 'NONE',  ( -40.49627896937849414, 203.4690446883607535, -1.626142955000504209 ) ) ;
#21126 = DIRECTION ( 'NONE',  ( 1.000000000000000000, 0.000000000000000000, 0.000000000000000000 ) ) ;
#21127 = AXIS2_PLACEMENT_3D ( 'NONE', #16061, #24026, #21565 ) ;
#21128 = CARTESIAN_POINT ( 'NONE',  ( -66.81919563604517975, 216.5000000000000000, -0.1155267958017906493 ) ) ;
#21129 = CARTESIAN_POINT ( 'NONE',  ( 24.70692427760507570, 0.000000000000000000, 161.2126178494294493 ) ) ;
#21130 = CARTESIAN_POINT ( 'NONE',  ( -8.962234695871565293, 90.43981371789855928, -8.715434833792128799 ) ) ;
#21131 = CARTESIAN_POINT ( 'NONE',  ( -48.02455436395490551, 206.6211998817774997, 3.209657149897401585 ) ) ;
#21132 =( BOUNDED_CURVE ( )  B_SPLINE_CURVE ( 2, ( #29079, #31564, #5587, #28715, #24350, #837, #10124 ),
 .UNSPECIFIED., .F., .F. ) 
 B_SPLINE_CURVE_WITH_KNOTS ( ( 3, 2, 2, 3 ),
 ( 0.9130434782608737310, 0.9202898550724665228, 0.9275362318840592035, 0.9334794156559244049 ),
 .UNSPECIFIED. ) 
 CURVE ( )  GEOMETRIC_REPRESENTATION_ITEM ( )  RATIONAL_B_SPLINE_CURVE ( ( 0.9999999999999219513, 0.8660254037845167563, 1.000000000000000000, 0.8660254037844387076, 1.000000000000000000, 0.8901194808422465687, 0.9604780343360148631 ) ) 
 REPRESENTATION_ITEM ( '' )  );
#21133 = CARTESIAN_POINT ( 'NONE',  ( -33.77455436395489841, 203.6929966515020283, 6.137860380172978303 ) ) ;
#21134 = CARTESIAN_POINT ( 'NONE',  ( 23.87821517812500005, -4.985214923628404016, -6.403124999385473082 ) ) ;
#21135 = CARTESIAN_POINT ( 'NONE',  ( 20.99999999999999645, 6.928203230275506996, -2.362500000000002043 ) ) ;
#21136 = CARTESIAN_POINT ( 'NONE',  ( -13.23911966647199812, 53.35231371789856780, -8.632099005475788900 ) ) ;
#21137 = CARTESIAN_POINT ( 'NONE',  ( -58.50669563604516554, 209.8844732041981729, -8.500000000000003553 ) ) ;
#21138 = CARTESIAN_POINT ( 'NONE',  ( 5.438367727407757775E-14, 198.5374999999999943, -27.00000000000000355 ) ) ;
#21139 = CARTESIAN_POINT ( 'NONE',  ( 4.622313124798573369, 92.63518628210145778, 11.61527771782819940 ) ) ;
#21140 = CARTESIAN_POINT ( 'NONE',  ( -0.1745138560725817967, 28.81018628210143717, 15.50000000000000533 ) ) ;
#21141 = CARTESIAN_POINT ( 'NONE',  ( 36.75931086529713099, 7.347880794884117764E-16, 161.2874679718108553 ) ) ;
#21142 = CARTESIAN_POINT ( 'NONE',  ( 24.39482925732963281, 3.604726614523240613, 160.4400036919872150 ) ) ;
#21143 = CARTESIAN_POINT ( 'NONE',  ( 14.38691631536207538, 53.53518628210145636, -5.770363421893813793 ) ) ;
#21144 = CARTESIAN_POINT ( 'NONE',  ( -27.24356964375000345, 198.4531250006145342, 0.000000000000000000 ) ) ;
#21145 = CARTESIAN_POINT ( 'NONE',  ( 15.00000000000000000, 0.000000000000000000, -3.993749998770945719 ) ) ;
#21146 = FACE_OUTER_BOUND ( 'NONE', #27116, .T. ) ;
#21147 = CARTESIAN_POINT ( 'NONE',  ( -42.08705436395489841, 205.3262412349647263, -4.842901733360204020 ) ) ;
#21148 = CARTESIAN_POINT ( 'NONE',  ( 22.56230152254351395, 3.464101615138092782, -7.724999998770981868 ) ) ;
#21149 = CARTESIAN_POINT ( 'NONE',  ( -11.48171059495397373, 13.28518628210142971, -4.944772684328680334 ) ) ;
#21150 =( BOUNDED_CURVE ( )  B_SPLINE_CURVE ( 2, ( #36669, #32895, #30439, #21543, #30246, #30807, #4458, #4273, #15847 ),
 .UNSPECIFIED., .F., .F. ) 
 B_SPLINE_CURVE_WITH_KNOTS ( ( 3, 2, 2, 2, 3 ),
 ( 0.01086956521739129364, 0.01449275362318840597, 0.02173913043478260809, 0.02898550724637681195, 0.03260869565217391908 ),
 .UNSPECIFIED. ) 
 CURVE ( )  GEOMETRIC_REPRESENTATION_ITEM ( )  RATIONAL_B_SPLINE_CURVE ( ( 0.9330127018922194093, 0.9330127018922191873, 1.000000000000000000, 0.8660254037844387076, 1.000000000000000000, 0.8660254037844387076, 1.000000000000000000, 0.9330127018922191873, 0.9330127018922192983 ) ) 
 REPRESENTATION_ITEM ( '' )  );
#21151 = CARTESIAN_POINT ( 'NONE',  ( 15.00000000000000000, 247.3187500012290343, -3.464101615137752610 ) ) ;
#21152 = CARTESIAN_POINT ( 'NONE',  ( 8.843639120294245259, 131.2648137178985621, 3.474262827703527901 ) ) ;
#21153 = CARTESIAN_POINT ( 'NONE',  ( 18.12178482187500350, 247.2343750006145342, 4.985214923628407568 ) ) ;
#21154 = ORIENTED_EDGE ( 'NONE', *, *, #2222, .F. ) ;
#21155 = CARTESIAN_POINT ( 'NONE',  ( 21.00000000000000000, -6.928203230275506996, -7.087500000000004796 ) ) ;
#21156 = CARTESIAN_POINT ( 'NONE',  ( 14.99999999999979039, -3.464101615137634038, -4.462499999999995026 ) ) ;
#21157 = LINE ( 'NONE', #291, #15850 ) ;
#21158 = CARTESIAN_POINT ( 'NONE',  ( 16.56230152254411436, -7.209453229046475009, -7.228124999385518556 ) ) ;
#21159 = CARTESIAN_POINT ( 'NONE',  ( 34.22950430627932406, 5.407089921784857367, 165.3954622995096599 ) ) ;
#21160 = FACE_OUTER_BOUND ( 'NONE', #35071, .T. ) ;
#21161 = CARTESIAN_POINT ( 'NONE',  ( -13.49999999999998401, 199.1750000000000114, 23.38268590217985476 ) ) ;
#21162 = CARTESIAN_POINT ( 'NONE',  ( 12.50000000000000355, 44.91018628210144215, 0.1745138560725507937 ) ) ;
#21163 = VERTEX_POINT ( 'NONE', #25741 ) ;
#21164 = ORIENTED_EDGE ( 'NONE', *, *, #9364, .T. ) ;
#21165 = FACE_OUTER_BOUND ( 'NONE', #15406, .T. ) ;
#21166 = CARTESIAN_POINT ( 'NONE',  ( 22.56230152254410370, 7.347880794884117764E-16, -1.912499998771022280 ) ) ;
#21167 = CARTESIAN_POINT ( 'NONE',  ( 1.069080835302379631E-14, 196.6250000012290400, 27.00000000000000000 ) ) ;
#21168 = CARTESIAN_POINT ( 'NONE',  ( -26.99999999999999645, 198.3500000012290343, 15.58845726811991561 ) ) ;
#21169 = CARTESIAN_POINT ( 'NONE',  ( 15.24356964374999990, 0.000000000000000000, -9.140624999385476457 ) ) ;
#21170 = CARTESIAN_POINT ( 'NONE',  ( 4.622313124798573369, 92.63518628210145778, 11.61527771782819940 ) ) ;
#21171 = CARTESIAN_POINT ( 'NONE',  ( 2.908627838312458636, 18.27731371789853299, -15.53471296425188442 ) ) ;
#21172 = MANIFOLD_SOLID_BREP ( 'Cavity1', #21098 ) ;
#21173 = CARTESIAN_POINT ( 'NONE',  ( 26.99999999999999645, 7.347880794884117764E-16, -6.018749998770944742 ) ) ;
#21174 = CARTESIAN_POINT ( 'NONE',  ( 20.28004929560864511, 210.7199507044221320, 5.999999999998711253 ) ) ;
#21175 = CARTESIAN_POINT ( 'NONE',  ( -67.01711230271185116, 214.4690446883608104, -1.321298161741814914 ) ) ;
#21176 = CARTESIAN_POINT ( 'NONE',  ( 15.00000000000000000, 245.4625000000000057, -3.464101615137752610 ) ) ;
#21177 = CARTESIAN_POINT ( 'NONE',  ( 25.14161354455898945, -3.464101615137757051, 166.1811389061620048 ) ) ;
#21178 = CARTESIAN_POINT ( 'NONE',  ( -12.50000000000000355, 135.2898137178985678, 0.1745138560722786503 ) ) ;
#21179 = CARTESIAN_POINT ( 'NONE',  ( -64.25372103062154849, 216.5309553116391612, -1.626142955000564383 ) ) ;
#21180 = CARTESIAN_POINT ( 'NONE',  ( -32.57961230271184405, 212.3930949314663792, 8.469044688360751749 ) ) ;
#21182 = APPLICATION_CONTEXT ( 'automotive_design' ) ;
#21181 = APPLICATION_PROTOCOL_DEFINITION ( 'draft international standard', 'automotive_design', 1998, #32784 ) ;
#21183 = CARTESIAN_POINT ( 'NONE',  ( 27.79682692271734012, 5.196152422706636465, 162.1092269564937851 ) ) ;
#21184 = CARTESIAN_POINT ( 'NONE',  ( -27.24356964374999990, 199.7656250006145342, -15.72908226750537786 ) ) ;
#21185 = CARTESIAN_POINT ( 'NONE',  ( 2.908627838312458636, 110.2773137178985650, -15.53471296425188442 ) ) ;
#21186 = CARTESIAN_POINT ( 'NONE',  ( -54.94419563604517265, 203.5000000000000000, 0.1155267958017914542 ) ) ;
#21187 = VERTEX_POINT ( 'NONE', #24029 ) ;
#21188 = CARTESIAN_POINT ( 'NONE',  ( -12.53471296425194836, 21.62268628210144072, 2.311890736173176641 ) ) ;
#21189 = CARTESIAN_POINT ( 'NONE',  ( 18.00000000000000000, 5.196152422706630247, -7.725000000000009415 ) ) ;
#21190 = ADVANCED_FACE ( 'NONE', ( #12648 ), #5275, .F. ) ;
#21191 = LINE ( 'NONE', #7154, #12012 ) ;
#21192 = CARTESIAN_POINT ( 'NONE',  ( 24.95044711734591658, -3.604726614523244610, 166.7907448923220954 ) ) ;
#21193 = CARTESIAN_POINT ( 'NONE',  ( 15.46528703574804986, 100.3976862821014606, 3.257655550457285720 ) ) ;
#21194 =( BOUNDED_CURVE ( )  B_SPLINE_CURVE ( 2, ( #35959, #9627, #6780, #21204, #35389, #9813, #33124 ),
 .UNSPECIFIED., .F., .F. ) 
 B_SPLINE_CURVE_WITH_KNOTS ( ( 3, 2, 2, 3 ),
 ( 0.5217391304347814840, 0.5289855072463758301, 0.5362318840579701762, 0.5434782608695644113 ),
 .UNSPECIFIED. ) 
 CURVE ( )  GEOMETRIC_REPRESENTATION_ITEM ( )  RATIONAL_B_SPLINE_CURVE ( ( 1.000000000000020428, 0.8660254037844181685, 1.000000000000000000, 0.8660254037844387076, 1.000000000000000000, 0.8660254037844530295, 0.9999999999999856781 ) ) 
 REPRESENTATION_ITEM ( '' )  );
#21195 = CARTESIAN_POINT ( 'NONE',  ( -68.01413769728823411, 213.1499508600178672, 5.686928522499718142 ) ) ;
#21196 = CARTESIAN_POINT ( 'NONE',  ( 19.68408634441911076, 5.407089921784857367, -4.790624999385539873 ) ) ;
#21197 = CARTESIAN_POINT ( 'NONE',  ( -8.152565276336710909, 67.04768628210143788, 5.233372021372435512 ) ) ;
#21198 = CARTESIAN_POINT ( 'NONE',  ( 0.000000000000000000, 143.0000000000000000, 0.000000000000000000 ) ) ;
#21199 = CARTESIAN_POINT ( 'NONE',  ( -41.29538769728824121, 212.3930949314662371, -8.469044688360781947 ) ) ;
#21200 = EDGE_CURVE ( 'NONE', #36238, #8445, #22174, .T. ) ;
#21201 = CARTESIAN_POINT ( 'NONE',  ( 10.69584247140445221, 80.84768628210144925, -6.932735513423970097 ) ) ;
#21202 = CARTESIAN_POINT ( 'NONE',  ( 7.234628195640312676, 199.8674038105676800, -27.00000000000000711 ) ) ;
#21203 = CARTESIAN_POINT ( 'NONE',  ( 0.000000000000000000, 0.000000000000000000, 5.000000000000000000 ) ) ;
#21204 = CARTESIAN_POINT ( 'NONE',  ( 20.99999999999999645, 6.928203230275506996, -5.512500000000003730 ) ) ;
#21205 = CARTESIAN_POINT ( 'NONE',  ( 27.55866236128991176, -5.407089921784859143, 160.7843176865825967 ) ) ;
#21206 = CARTESIAN_POINT ( 'NONE',  ( 15.00000000000000000, 0.000000000000000000, -0.9000000000000119016 ) ) ;
#21207 = AXIS2_PLACEMENT_3D ( 'NONE', #6596, #9068, #35586 ) ;
#21208 = CARTESIAN_POINT ( 'NONE',  ( 34.36556471527461554, 5.196152422706631135, 168.3479640145299641 ) ) ;
#21209 = CARTESIAN_POINT ( 'NONE',  ( 34.22460179574976991, 5.407089921784862696, 165.3394263477420054 ) ) ;
#21210 = CARTESIAN_POINT ( 'NONE',  ( 33.98970557456826214, -5.196152422706635576, 164.0518743777849409 ) ) ;
#21211 = CARTESIAN_POINT ( 'NONE',  ( 21.00000000000000000, 246.0625000000000000, 6.928203230275506996 ) ) ;
#21212 = CARTESIAN_POINT ( 'NONE',  ( -1.926257025242585782E-15, 196.9906250006145001, -31.45816453501076637 ) ) ;
#21213 = CARTESIAN_POINT ( 'NONE',  ( -11.61527771782809282, 99.06481371789855928, -4.622313124798832717 ) ) ;
#21214 = CARTESIAN_POINT ( 'NONE',  ( 0.1745138560725515708, 107.0101862821014578, -12.50000000000000355 ) ) ;
#21215 = ORIENTED_EDGE ( 'NONE', *, *, #12154, .T. ) ;
#21216 = ORIENTED_EDGE ( 'NONE', *, *, #4481, .F. ) ;
#21217 = CARTESIAN_POINT ( 'NONE',  ( -27.00000000000000355, 199.6625000012290343, 0.000000000000000000 ) ) ;
#21218 = CARTESIAN_POINT ( 'NONE',  ( 26.75643035624999655, 240.0718750006145399, -7.049594010296217766E-16 ) ) ;
#21219 = EDGE_CURVE ( 'NONE', #16114, #33325, #12485, .T. ) ;
#21220 = CARTESIAN_POINT ( 'NONE',  ( 14.25334919248795451, 74.91481371789855359, -6.092822981423661410 ) ) ;
#21221 = CARTESIAN_POINT ( 'NONE',  ( 21.00000000000000000, -6.646953231504538984, -7.790624999385473259 ) ) ;
#21222 = CARTESIAN_POINT ( 'NONE',  ( 18.12178482187500350, 246.3343750006145285, 4.985214923628407568 ) ) ;
#21223 = CARTESIAN_POINT ( 'NONE',  ( 8.843639120294328748, 99.53518628210146346, -3.474262827703334722 ) ) ;
#21224 = CARTESIAN_POINT ( 'NONE',  ( 13.50000000000001421, 194.8625000012290513, 23.38268590217984055 ) ) ;
#21225 = CARTESIAN_POINT ( 'NONE',  ( 5.233372021372610483, 55.65231371789855785, -8.152565276336593669 ) ) ;
#21226 = CARTESIAN_POINT ( 'NONE',  ( 22.80587116629411781, 3.604726614523238837, -4.378124999385524241 ) ) ;
#21227 = CARTESIAN_POINT ( 'NONE',  ( 0.1745138560723095977, 114.5898137178985650, 9.500000000000005329 ) ) ;
#21228 = FACE_OUTER_BOUND ( 'NONE', #22029, .T. ) ;
#21229 = CARTESIAN_POINT ( 'NONE',  ( 12.46528703574811558, 29.20231371789855501, -2.660918448318005503 ) ) ;
#21230 = LINE ( 'NONE', #35230, #17017 ) ;
#21231 = AXIS2_PLACEMENT_3D ( 'NONE', #3339, #23632, #20794 ) ;
#21232 = MANIFOLD_SOLID_BREP ( 'Thread1', #14427 ) ;
#21233 = CARTESIAN_POINT ( 'NONE',  ( -2.660918448318275509, 84.29768628210145209, 12.46528703574805874 ) ) ;
#21234 = CARTESIAN_POINT ( 'NONE',  ( 10.56230152254410726, 0.000000000000000000, -6.637499998771001941 ) ) ;
#21235 = CARTESIAN_POINT ( 'NONE',  ( 20.99999999999999645, 6.928203230275506996, -1.856249998770964638 ) ) ;
#21236 = CARTESIAN_POINT ( 'NONE',  ( 31.00520690578787253, 7.209453229046475009, 164.3600382331131300 ) ) ;
#21237 = CARTESIAN_POINT ( 'NONE',  ( 15.53471296425195369, 90.62268628210145494, -2.908627838312120684 ) ) ;
#21238 = CARTESIAN_POINT ( 'NONE',  ( 19.68408634441911076, 5.407089921784862696, -3.946874999385563410 ) ) ;
#21239 = CARTESIAN_POINT ( 'NONE',  ( 20.99999999999995026, 241.3375000000000341, -5.999999999999998224 ) ) ;
#21240 = EDGE_CURVE ( 'NONE', #26868, #18985, #32448, .T. ) ;
#21241 = CARTESIAN_POINT ( 'NONE',  ( 10.31873187879411091, 0.000000000000000000, -0.1406249993855246405 ) ) ;
#21242 = CARTESIAN_POINT ( 'NONE',  ( -6.594114490232312775, 115.0601862821014691, -6.840914352312096547 ) ) ;
#21243 = CARTESIAN_POINT ( 'NONE',  ( 20.99999999999999645, -6.928203230275506996, -4.331249998770957177 ) ) ;
#21244 = CARTESIAN_POINT ( 'NONE',  ( 12.50000000000000355, 127.7101862821014606, 0.1745138560725507937 ) ) ;
#21245 = CARTESIAN_POINT ( 'NONE',  ( -27.24356964375000345, 194.9093750006145456, 0.000000000000000000 ) ) ;
#21246 = CARTESIAN_POINT ( 'NONE',  ( 15.24356964375000167, 240.7843750006145171, 3.323476615752272600 ) ) ;
#21248 = EDGE_LOOP ( 'NONE', ( #2157, #12182 ) ) ;
#21247 = MECHANICAL_DESIGN_GEOMETRIC_PRESENTATION_REPRESENTATION (  '', ( #26656 ), #26062 ) ;
#21249 = CARTESIAN_POINT ( 'NONE',  ( 28.13389026342440857, 5.407089921784856479, 167.3592026939881237 ) ) ;
#21250 = CARTESIAN_POINT ( 'NONE',  ( 23.87821517812500005, -4.985214923628404016, -1.790624999385481697 ) ) ;
#21252 = EDGE_CURVE ( 'NONE', #27758, #30367, #16589, .T. ) ;
#21251 = CARTESIAN_POINT ( 'NONE',  ( 22.56230152254410370, 7.347880794884117764E-16, -5.062499998771007981 ) ) ;
#21253 = CARTESIAN_POINT ( 'NONE',  ( -12.50000000000000355, 5.000000000000004441, -1.353084311261909534E-13 ) ) ;
#21254 = CYLINDRICAL_SURFACE ( 'NONE', #31229, 5.999999999999999112 ) ;
#21255 = CARTESIAN_POINT ( 'NONE',  ( 26.99999999999999645, 199.4750000012290343, -15.58845726811990495 ) ) ;
#21256 = CARTESIAN_POINT ( 'NONE',  ( -9.500000000000005329, 24.88981371789854080, 0.1745138560723101806 ) ) ;
#21257 = CARTESIAN_POINT ( 'NONE',  ( -27.24356964374999279, 198.0968750006145456, 15.72908226750539384 ) ) ;
#21259 = VERTEX_POINT ( 'NONE', #30180 ) ;
#21258 = EDGE_LOOP ( 'NONE', ( #8182, #20870, #23067 ) ) ;
#21260 = CARTESIAN_POINT ( 'NONE',  ( 26.75643035624999655, 248.1718750006145342, -7.049594010296217766E-16 ) ) ;
#21261 = CARTESIAN_POINT ( 'NONE',  ( 2.311890736173452421, 18.27731371789853654, -12.53471296425189152 ) ) ;
#21262 = CARTESIAN_POINT ( 'NONE',  ( 23.87821517812500005, -4.985214923628404016, -0.4406249993854638447 ) ) ;
#21263 = CARTESIAN_POINT ( 'NONE',  ( 15.46528703574811736, 130.4023137178985792, -3.257655550456947768 ) ) ;
#21264 = CARTESIAN_POINT ( 'NONE',  ( 15.00000000000000000, 3.464101615137752166, -7.181249998770951493 ) ) ;
#21265 =( BOUNDED_CURVE ( )  B_SPLINE_CURVE ( 2, ( #13803, #22332, #5068, #18938, #4882, #21777, #2038 ),
 .UNSPECIFIED., .F., .F. ) 
 B_SPLINE_CURVE_WITH_KNOTS ( ( 3, 2, 2, 3 ),
 ( 0.08695652173913158423, 0.09420289855072500051, 0.1014492753623184029, 0.1086956521739118053 ),
 .UNSPECIFIED. ) 
 CURVE ( )  GEOMETRIC_REPRESENTATION_ITEM ( )  RATIONAL_B_SPLINE_CURVE ( ( 0.9999999999999786837, 0.8660254037844600239, 1.000000000000000000, 0.8660254037844387076, 1.000000000000000000, 0.8660254037844615782, 0.9999999999999771294 ) ) 
 REPRESENTATION_ITEM ( '' )  );
#21266 = DIRECTION ( 'NONE',  ( 0.000000000000000000, 0.000000000000000000, 1.000000000000000000 ) ) ;
#21267 = ORIENTED_EDGE ( 'NONE', *, *, #3669, .F. ) ;
#21268 = CARTESIAN_POINT ( 'NONE',  ( 10.31873187879410736, -3.604726614523244610, -5.109374999385545735 ) ) ;
#21269 = CARTESIAN_POINT ( 'NONE',  ( -1.926257025242585782E-15, 195.6406250006145058, -31.45816453501075927 ) ) ;
#21270 = CARTESIAN_POINT ( 'NONE',  ( 12.53471296425194836, 136.6226862821014834, -2.311890736173178418 ) ) ;
#21271 = CARTESIAN_POINT ( 'NONE',  ( 30.96108431102187808, 7.209453229046482114, 163.8557146672041824 ) ) ;
#21272 = AXIS2_PLACEMENT_3D ( 'NONE', #33004, #9699, #32435 ) ;
#21273 = CARTESIAN_POINT ( 'NONE',  ( -58.50669563604516554, 209.8844732041981729, -8.500000000000003553 ) ) ;
#21274 = CARTESIAN_POINT ( 'NONE',  ( 26.75643035624999655, 247.3093750006144944, -3.323476615752271268 ) ) ;
#21275 =( NAMED_UNIT ( * ) PLANE_ANGLE_UNIT ( ) SI_UNIT ( $, .RADIAN. ) );
#21276 = CARTESIAN_POINT ( 'NONE',  ( 13.56230152254411614, -5.196152422706632912, -9.712499998771024323 ) ) ;
#21277 = CARTESIAN_POINT ( 'NONE',  ( -39.11086230271183695, 212.1499508600178387, -3.954877714930852495 ) ) ;
#21278 = CARTESIAN_POINT ( 'NONE',  ( -36.54538769728823411, 211.8571965466039444, -6.469044688360768625 ) ) ;
#21279 = CARTESIAN_POINT ( 'NONE',  ( 37.44726502606470575, -3.604726614523235284, 166.3561717635493835 ) ) ;
#21280 = VERTEX_POINT ( 'NONE', #29608 ) ;
#21281 = CARTESIAN_POINT ( 'NONE',  ( -28.51651240191029757, 203.9818979280190092, 5.277347936512516213 ) ) ;
#21282 = CARTESIAN_POINT ( 'NONE',  ( -14.38691631536207183, 140.9351862821014549, 5.770363421893814682 ) ) ;
#21283 = CARTESIAN_POINT ( 'NONE',  ( -44.85788769728823411, 218.4690446883607535, 2.393094931466250408 ) ) ;
#21284 = CARTESIAN_POINT ( 'NONE',  ( -8.152565276336710909, 122.2476862821014691, 5.233372021372435512 ) ) ;
#21285 = ADVANCED_FACE ( 'NONE', ( #4206 ), #36043, .T. ) ;
#21286 = CARTESIAN_POINT ( 'NONE',  ( 20.99999999999999645, 249.2687500012290513, 5.999999999999998224 ) ) ;
#21287 = CARTESIAN_POINT ( 'NONE',  ( 4.944772684328679446, 33.98518628210143788, -11.48171059495397373 ) ) ;
#21288 = CARTESIAN_POINT ( 'NONE',  ( 22.56230152254411436, 3.464101615137759271, -7.387500000000012612 ) ) ;
#21289 = VERTEX_POINT ( 'NONE', #981 ) ;
#21290 = CARTESIAN_POINT ( 'NONE',  ( 27.00000000000001421, 197.6000000012290627, 15.58845726811988897 ) ) ;
#21291 = CARTESIAN_POINT ( 'NONE',  ( -8.927990412390661490, 130.8726862821014834, 13.04141134922759804 ) ) ;
#21292 = CARTESIAN_POINT ( 'NONE',  ( 37.26917196037089042, 7.347880794884117764E-16, 167.1152069556475510 ) ) ;
#21293 = CARTESIAN_POINT ( 'NONE',  ( 1.715153634034445762, 137.8773137178985735, -9.534712964251895073 ) ) ;
#21294 = CARTESIAN_POINT ( 'NONE',  ( 13.62178482187499640, 198.3031250006145285, -23.59362340125807123 ) ) ;
#21295 = CARTESIAN_POINT ( 'NONE',  ( -1.045839947578415010E-13, 196.5125000000000455, 27.00000000000000355 ) ) ;
#21296 = CARTESIAN_POINT ( 'NONE',  ( 5.727106289114498080E-15, 195.6125000000000398, 31.17691453623979214 ) ) ;
#21297 = CARTESIAN_POINT ( 'NONE',  ( 15.75780091040682862, -6.201764924782260380, -10.00000000000000000 ) ) ;
#21298 = DIRECTION ( 'NONE',  ( -0.000000000000000000, -0.000000000000000000, 1.000000000000000000 ) ) ;
#21299 = CARTESIAN_POINT ( 'NONE',  ( 36.78872592836736288, 7.347880794884125653E-16, 161.6236836811924604 ) ) ;
#21300 = CARTESIAN_POINT ( 'NONE',  ( 1.715153634034445762, 82.67731371789852801, -9.534712964251895073 ) ) ;
#21301 = CYLINDRICAL_SURFACE ( 'NONE', #6352, 5.999999999999999112 ) ;
#21302 = ORIENTED_EDGE ( 'NONE', *, *, #8088, .T. ) ;
#21303 = CARTESIAN_POINT ( 'NONE',  ( 21.00000000000000000, 244.0937500012290400, -6.928203230275506996 ) ) ;
#21304 = CARTESIAN_POINT ( 'NONE',  ( 8.715434833792128799, 83.53981371789856780, -8.962234695871567070 ) ) ;
#21305 = CARTESIAN_POINT ( 'NONE',  ( 22.80587116629412137, 7.646167579472024665E-16, -3.571874999385521221 ) ) ;
#21306 = CARTESIAN_POINT ( 'NONE',  ( -6.996070402016868250, 143.0000000000000000, 10.82654737139870882 ) ) ;
#21307 = CARTESIAN_POINT ( 'NONE',  ( 15.24356964374999990, 0.000000000000000000, -4.303124999385482319 ) ) ;
#21308 = CARTESIAN_POINT ( 'NONE',  ( 11.61527771782809637, 39.26481371789855501, 4.622313124798827388 ) ) ;
#21309 = ORIENTED_EDGE ( 'NONE', *, *, #6809, .F. ) ;
#21310 = LINE ( 'NONE', #30198, #28014 ) ;
#21311 = CARTESIAN_POINT ( 'NONE',  ( 18.12178482187499640, 244.2718750006145001, -4.985214923628404904 ) ) ;
#21312 = CARTESIAN_POINT ( 'NONE',  ( -10.69584247140444866, 21.04768628210144854, 6.932735513423972762 ) ) ;
#21313 = CARTESIAN_POINT ( 'NONE',  ( -39.70461230271183695, 208.1428034533958851, -6.469044688360754414 ) ) ;
#21314 = CARTESIAN_POINT ( 'NONE',  ( -56.72544563604517265, 214.8429017333602360, 4.673758765035156415 ) ) ;
#21315 = VECTOR ( 'NONE', #15924, 1000.000000000000000 ) ;
#21316 = CARTESIAN_POINT ( 'NONE',  ( 36.55994210376188391, -3.464101615137751278, 159.0086725999259727 ) ) ;
#21317 = CARTESIAN_POINT ( 'NONE',  ( 12.46528703574811558, 84.40231371789853654, -2.660918448318005503 ) ) ;
#21318 = CARTESIAN_POINT ( 'NONE',  ( -48.81622103062156981, 211.0902445701382533, 4.530955311639240257 ) ) ;
#21319 = EDGE_CURVE ( 'NONE', #29192, #8245, #21465, .T. ) ;
#21320 = CARTESIAN_POINT ( 'NONE',  ( -68.60788769728823411, 216.4690446883607535, 1.857196546604031662 ) ) ;
#21321 = CARTESIAN_POINT ( 'NONE',  ( 15.24356964375000167, -3.323476615752272600, -6.965624999385507721 ) ) ;
#21322 = CARTESIAN_POINT ( 'NONE',  ( 10.56230152254410903, 0.000000000000000000, -7.200000000000040146 ) ) ;
#21323 = CARTESIAN_POINT ( 'NONE',  ( -3.257655550456946880, 54.50231371789855928, -15.46528703574811736 ) ) ;
#21324 = CARTESIAN_POINT ( 'NONE',  ( -39.50669563604516554, 209.8844732041981729, -8.500000000000003553 ) ) ;
#21325 = AXIS2_PLACEMENT_3D ( 'NONE', #18301, #15071, #32684 ) ;
#21326 = CARTESIAN_POINT ( 'NONE',  ( 25.02068495149662297, 0.000000000000000000, 164.7989187625597367 ) ) ;
#21327 = CARTESIAN_POINT ( 'NONE',  ( -2.660918448318275509, 84.29768628210145209, 12.46528703574805874 ) ) ;
#21328 = EDGE_CURVE ( 'NONE', #23913, #23915, #27632, .T. ) ;
#21329 = CARTESIAN_POINT ( 'NONE',  ( 11.08355503943142750, 34.56018628210144783, -10.83675517735155225 ) ) ;
#21330 = CARTESIAN_POINT ( 'NONE',  ( -77.00000000000002842, 210.0000000000000000, 5.000000000000000888 ) ) ;
#21331 = FACE_OUTER_BOUND ( 'NONE', #22442, .T. ) ;
#21332 = VERTEX_POINT ( 'NONE', #33583 ) ;
#21333 = CARTESIAN_POINT ( 'NONE',  ( 6.092822981423978490, 43.18518628210144072, -14.25334919248782306 ) ) ;
#21334 = CARTESIAN_POINT ( 'NONE',  ( 13.62178482187501416, 197.2531250006145456, 23.59362340125806767 ) ) ;
#21335 = CARTESIAN_POINT ( 'NONE',  ( -1.926257025242585782E-15, 199.7468750006145513, -31.45816453501075927 ) ) ;
#21336 = CARTESIAN_POINT ( 'NONE',  ( 18.00000000000000355, -5.196152422706632912, -2.118749998770957710 ) ) ;
#21337 = CARTESIAN_POINT ( 'NONE',  ( -43.07663769728823411, 204.3130714775002730, 3.149950860017883603 ) ) ;
#21338 = CARTESIAN_POINT ( 'NONE',  ( -13.50000000000000533, 195.4250000000000114, -23.38268590217984411 ) ) ;
#21339 = CARTESIAN_POINT ( 'NONE',  ( -0.1745138560725500443, 19.61018628210144144, 12.50000000000000355 ) ) ;
#21340 = CARTESIAN_POINT ( 'NONE',  ( 23.87821517812500005, 249.5593750006145228, 4.985214923628404016 ) ) ;
#21341 = CARTESIAN_POINT ( 'NONE',  ( -5.529263428287297444, 136.7273137178985110, -7.954856959092311719 ) ) ;
#21342 = CARTESIAN_POINT ( 'NONE',  ( 23.87821517812499650, 242.9593750006145285, -4.985214923628404904 ) ) ;
#21343 = EDGE_LOOP ( 'NONE', ( #34789, #17742, #7991, #30603 ) ) ;
#21344 = CARTESIAN_POINT ( 'NONE',  ( 18.00000000000000000, 5.196152422706630247, -6.374999999999992006 ) ) ;
#21345 = DIRECTION ( 'NONE',  ( 1.000000000000000000, 0.000000000000000000, 0.000000000000000000 ) ) ;
#21346 = CARTESIAN_POINT ( 'NONE',  ( -2.660918448318005058, 137.3023137178985564, -12.46528703574811558 ) ) ;
#21347 = CARTESIAN_POINT ( 'NONE',  ( 16.56230152254411081, 7.209453229046475009, -6.103124999385545202 ) ) ;
#21348 = CARTESIAN_POINT ( 'NONE',  ( 24.83768937516614272, -3.604726614523240613, 165.5019180016658993 ) ) ;
#21349 = CARTESIAN_POINT ( 'NONE',  ( -1.909035429704832693E-15, 199.4375000000000284, -31.17691453623979214 ) ) ;
#21350 = CARTESIAN_POINT ( 'NONE',  ( 12.50000000000000355, 54.11018628210144499, 0.1745138560725507937 ) ) ;
#21351 = ORIENTED_EDGE ( 'NONE', *, *, #35567, .T. ) ;
#21352 = ORIENTED_EDGE ( 'NONE', *, *, #5298, .F. ) ;
#21353 = CARTESIAN_POINT ( 'NONE',  ( 24.56230152254410726, 0.000000000000000000, -10.00000000000000000 ) ) ;
#21354 = CARTESIAN_POINT ( 'NONE',  ( 20.99999999999999645, -6.646953231504538984, -1.378124999385478056 ) ) ;
#21355 = CARTESIAN_POINT ( 'NONE',  ( 15.00000000000045297, -3.464101615138017287, -1.312499999999984457 ) ) ;
#21356 = CARTESIAN_POINT ( 'NONE',  ( 0.000000000000000000, 200.0000000000000000, 0.000000000000000000 ) ) ;
#21357 = CARTESIAN_POINT ( 'NONE',  ( 21.00000000000000000, -6.646953231504538984, -9.478124999385466154 ) ) ;
#21358 = CARTESIAN_POINT ( 'NONE',  ( -7.228626920339069173, 75.67268628210146630, 10.49813415415989581 ) ) ;
#21359 = CARTESIAN_POINT ( 'NONE',  ( -15.53471296425188442, 15.97731371789853405, -2.908627838312459080 ) ) ;
#21360 =( BOUNDED_CURVE ( )  B_SPLINE_CURVE ( 3, ( #2193, #22121, #33669, #36691 ),
 .UNSPECIFIED., .F., .F. ) 
 B_SPLINE_CURVE_WITH_KNOTS ( ( 4, 4 ),
 ( 0.000000000000000000, 1.570796326794937414 ),
 .UNSPECIFIED. ) 
 CURVE ( )  GEOMETRIC_REPRESENTATION_ITEM ( )  RATIONAL_B_SPLINE_CURVE ( ( 1.000000000000000000, 0.8047378541243555006, 0.8047378541243555006, 1.000000000000000000 ) ) 
 REPRESENTATION_ITEM ( '' )  );
#21361 = CARTESIAN_POINT ( 'NONE',  ( 26.99999999999999645, 243.4937500012290457, 3.464101615137751278 ) ) ;
#21362 = CARTESIAN_POINT ( 'NONE',  ( 14.16903250681090398, 216.8309674931867903, 1.338899061175305771 ) ) ;
#21363 = CARTESIAN_POINT ( 'NONE',  ( -35.75372103062156981, 214.5309553116392749, -1.090244570138262148 ) ) ;
#21364 = DIRECTION ( 'NONE',  ( -0.000000000000000000, -0.000000000000000000, 1.000000000000000000 ) ) ;
#21365 = CARTESIAN_POINT ( 'NONE',  ( 37.26917196037089042, 7.347880794884117764E-16, 167.1152069556475510 ) ) ;
#21366 = CARTESIAN_POINT ( 'NONE',  ( -2.660918448318004614, 137.3023137178985564, -12.46528703574811558 ) ) ;
#21367 = CARTESIAN_POINT ( 'NONE',  ( -44.65997103062156981, 215.5714017266979852, 3.350049139982118618 ) ) ;
#21368 = CARTESIAN_POINT ( 'NONE',  ( -65.04538769728823411, 212.3930949314662371, -8.469044688360781947 ) ) ;
#21369 = SHAPE_DEFINITION_REPRESENTATION ( #25269, #9842 ) ;
#21370 = CARTESIAN_POINT ( 'NONE',  ( 33.76745843056175289, 5.196152422706637353, 161.5115778976509944 ) ) ;
#21371 = CARTESIAN_POINT ( 'NONE',  ( -13.62178482187500528, 197.9281250006145569, -23.59362340125807123 ) ) ;
#21372 = CARTESIAN_POINT ( 'NONE',  ( 15.46528703574811736, 112.0023137178985451, -3.257655550456947768 ) ) ;
#21373 = CARTESIAN_POINT ( 'NONE',  ( -45.84002896937850124, 204.4285982733020433, 3.350049139982171020 ) ) ;
#21374 = ORIENTED_EDGE ( 'NONE', *, *, #18146, .T. ) ;
#21375 = CARTESIAN_POINT ( 'NONE',  ( 12.46528703574805874, 35.99768628210144072, 2.660918448318279950 ) ) ;
#21376 = CARTESIAN_POINT ( 'NONE',  ( 23.99999999999999645, 5.196152422706631135, -7.800000000000001599 ) ) ;
#21377 = CIRCLE ( 'NONE', #758, 9.999999999999994671 ) ;
#21378 = CARTESIAN_POINT ( 'NONE',  ( 28.43742163191258499, -5.196152422706638241, 169.4312579874681148 ) ) ;
#21379 = CARTESIAN_POINT ( 'NONE',  ( 28.05054758442196672, 5.407089921784862696, 166.4065915139379115 ) ) ;
#21380 = CARTESIAN_POINT ( 'NONE',  ( -15.46528703574804986, 104.9976862821014549, -3.257655550457287497 ) ) ;
#21381 = CARTESIAN_POINT ( 'NONE',  ( -61.68080436395489841, 203.5000000000000000, -0.1155267958017335561 ) ) ;
#21382 = CARTESIAN_POINT ( 'NONE',  ( 22.80587116629410716, 7.646167579472015790E-16, -5.315624999385537564 ) ) ;
#21383 = CARTESIAN_POINT ( 'NONE',  ( -1.715153634034234598, 42.32268628210145067, -9.534712964251941258 ) ) ;
#21384 = CARTESIAN_POINT ( 'NONE',  ( 15.00000000000000178, 240.6437500012289945, 3.464101615137757051 ) ) ;
#21385 = CARTESIAN_POINT ( 'NONE',  ( -41.09747103062157692, 214.3500491399821044, -7.303452534266878793 ) ) ;
#21386 = DIRECTION ( 'NONE',  ( 0.000000000000000000, 0.000000000000000000, 1.000000000000000000 ) ) ;
#21387 = CARTESIAN_POINT ( 'NONE',  ( 4.622313124798573369, 74.23518628210145209, 11.61527771782819940 ) ) ;
#21388 = CARTESIAN_POINT ( 'NONE',  ( 13.56230152254411614, -5.196152422706638241, -8.475000000000093792 ) ) ;
#21389 = DIRECTION ( 'NONE',  ( -0.1219804832088933616, -0.9925324990730152175, 0.000000000000000000 ) ) ;
#21390 = CARTESIAN_POINT ( 'NONE',  ( -6.840914352312096547, 39.16018628210144215, 6.594114490232313663 ) ) ;
#21391 = FACE_OUTER_BOUND ( 'NONE', #5961, .T. ) ;
#21392 = CARTESIAN_POINT ( 'NONE',  ( 15.00000000000000000, 0.000000000000000000, 0.000000000000000000 ) ) ;
#21393 = MECHANICAL_DESIGN_GEOMETRIC_PRESENTATION_REPRESENTATION (  '', ( #7467 ), #17755 ) ;
#21394 = CARTESIAN_POINT ( 'NONE',  ( 24.55497793462844669, 0.000000000000000000, 162.2705114497308045 ) ) ;
#21395 = CARTESIAN_POINT ( 'NONE',  ( 30.80175271875776843, -6.928203230275514990, 162.0345462341430505 ) ) ;
#21396 = CARTESIAN_POINT ( 'NONE',  ( 15.00000000000000000, 245.5000000000000000, 0.000000000000000000 ) ) ;
#21397 = AXIS2_PLACEMENT_3D ( 'NONE', #1272, #35582, #9438 ) ;
#21398 = CARTESIAN_POINT ( 'NONE',  ( 5.778771075727756162E-15, 196.7656250006145342, 31.45816453501076637 ) ) ;
#21399 = CARTESIAN_POINT ( 'NONE',  ( 7.228626920338837358, 95.32731371789856212, 10.49813415416005036 ) ) ;
#21400 = CARTESIAN_POINT ( 'NONE',  ( -0.1745138560725500443, 111.6101862821014521, 12.50000000000000355 ) ) ;
#21401 = ORIENTED_EDGE ( 'NONE', *, *, #16877, .T. ) ;
#21402 = ORIENTED_EDGE ( 'NONE', *, *, #7744, .F. ) ;
#21403 = CARTESIAN_POINT ( 'NONE',  ( 27.24356964375000345, 195.9781250006145399, -3.336375036156643733E-15 ) ) ;
#21404 = CARTESIAN_POINT ( 'NONE',  ( 15.24356964375000167, 240.7843750006145171, 3.323476615752272600 ) ) ;
#21405 = CARTESIAN_POINT ( 'NONE',  ( -15.50000000000000533, 80.08981371789856496, 0.1745138560722471477 ) ) ;
#21406 = ADVANCED_FACE ( 'NONE', ( #16716 ), #36599, .T. ) ;
#21407 = CARTESIAN_POINT ( 'NONE',  ( 26.75643035624999655, 7.049594010296217766E-16, -6.778124999385487293 ) ) ;
#21408 = CARTESIAN_POINT ( 'NONE',  ( 21.00000000000000000, 244.7968750006145626, -6.646953231504538984 ) ) ;
#21409 = CARTESIAN_POINT ( 'NONE',  ( 9.500000000000005329, 100.1101862821014521, 0.1745138560725188748 ) ) ;
#21410 = CARTESIAN_POINT ( 'NONE',  ( -27.00000000000000355, 194.7125000012290172, 0.000000000000000000 ) ) ;
#21411 = CARTESIAN_POINT ( 'NONE',  ( -3.796722387233185003, 54.21481371789855785, -8.710071997420207879 ) ) ;
#21412 = CARTESIAN_POINT ( 'NONE',  ( 22.80587116629410360, 7.646167579472015790E-16, -8.015624999385517313 ) ) ;
#21413 = CARTESIAN_POINT ( 'NONE',  ( 8.843639120294245259, 112.8648137178985564, 3.474262827703527901 ) ) ;
#21414 = CARTESIAN_POINT ( 'NONE',  ( 23.87821517812500005, 239.9968750006144944, 4.985214923628404016 ) ) ;
#21415 = CARTESIAN_POINT ( 'NONE',  ( 4.944772684328420986, 22.01481371789855501, 11.48171059495408208 ) ) ;
#21416 = CARTESIAN_POINT ( 'NONE',  ( 25.21678537267883868, 0.000000000000000000, 167.0403568332661450 ) ) ;
#21417 = CARTESIAN_POINT ( 'NONE',  ( 11.48171059495397728, 91.48518628210145209, 4.944772684328674117 ) ) ;
#21418 = CARTESIAN_POINT ( 'NONE',  ( 13.56230152254411436, -5.196152422706632912, -6.112499998771031784 ) ) ;
#21419 = AXIS2_PLACEMENT_3D ( 'NONE', #1227, #3893, #27387 ) ;
#21420 = ADVANCED_FACE ( 'NONE', ( #16527 ), #2108, .T. ) ;
#21421 = CARTESIAN_POINT ( 'NONE',  ( 7.234628195640309123, 196.2674038105676573, -27.00000000000000711 ) ) ;
#21422 = CARTESIAN_POINT ( 'NONE',  ( 24.71349244175073778, 3.604726614523236616, 164.0823405568851570 ) ) ;
#21423 = CARTESIAN_POINT ( 'NONE',  ( 19.68408634441911786, -5.407089921784861808, -4.546874999385525307 ) ) ;
#21424 = CARTESIAN_POINT ( 'NONE',  ( 5.999999999999999112, -30.00000000000000000, -19.99999999999999289 ) ) ;
#21425 = CARTESIAN_POINT ( 'NONE',  ( 21.00000000000000000, 244.2624999999999886, 5.999999999999998224 ) ) ;
#21426 = CARTESIAN_POINT ( 'NONE',  ( 8.152565276336714462, 117.6476862821014322, -5.233372021372432847 ) ) ;
#21427 = LINE ( 'NONE', #32969, #21315 ) ;
#21428 = ADVANCED_FACE ( 'NONE', ( #10269 ), #34134, .T. ) ;
#21429 = CARTESIAN_POINT ( 'NONE',  ( -10.49813415415989581, 123.9726862821014493, -7.228626920339068285 ) ) ;
#21430 = AXIS2_PLACEMENT_3D ( 'NONE', #10274, #19390, #7255 ) ;
#21431 = CARTESIAN_POINT ( 'NONE',  ( 20.99999999999997868, 210.0000000000000000, 5.999999999999999112 ) ) ;
#21432 = CARTESIAN_POINT ( 'NONE',  ( 26.75643035624999655, 249.6718750006145342, -3.323476615752271712 ) ) ;
#21433 = ORIENTED_EDGE ( 'NONE', *, *, #17603, .F. ) ;
#21434 = CARTESIAN_POINT ( 'NONE',  ( 28.10774354060011504, -5.407089921784859143, 167.0603442845606139 ) ) ;
#21435 = CARTESIAN_POINT ( 'NONE',  ( 18.12178482187500350, -4.985214923628407568, -2.765624999385457805 ) ) ;
#21436 = CARTESIAN_POINT ( 'NONE',  ( 22.56230152254411792, 7.347880794884125653E-16, -4.725000000000035172 ) ) ;
#21437 = CYLINDRICAL_SURFACE ( 'NONE', #11835, 6.000000000000001776 ) ;
#21438 = PLANE ( 'NONE',  #33039 ) ;
#21439 = CARTESIAN_POINT ( 'NONE',  ( 17.48528137423856776, 206.4852813742385820, 5.999999999999996447 ) ) ;
#21440 = CARTESIAN_POINT ( 'NONE',  ( 7.234628195640337545, 198.5174038105677141, -26.99999999999999289 ) ) ;
#21441 = CARTESIAN_POINT ( 'NONE',  ( -7.954856959092309943, 14.82731371789855324, 5.529263428287300108 ) ) ;
#21442 = CARTESIAN_POINT ( 'NONE',  ( 13.62178482187499640, 198.3593750006145342, -23.59362340125807123 ) ) ;
#21444 = ORIENTED_EDGE ( 'NONE', *, *, #14737, .F. ) ;
#21443 = ORIENTED_EDGE ( 'NONE', *, *, #31093, .T. ) ;
#21445 = AXIS2_PLACEMENT_3D ( 'NONE', #21531, #4260, #20777 ) ;
#21446 = AXIS2_PLACEMENT_3D ( 'NONE', #15768, #30549, #12918 ) ;
#21447 = CARTESIAN_POINT ( 'NONE',  ( 21.00000000000000000, 246.9343750006145228, -6.646953231504538984 ) ) ;
#21448 = CARTESIAN_POINT ( 'NONE',  ( -2.311890736173447980, 22.87731371789854151, 12.53471296425189330 ) ) ;
#21449 = CARTESIAN_POINT ( 'NONE',  ( 26.75643035624999655, 3.323476615752271712, -1.228124999385458160 ) ) ;
#21450 = CARTESIAN_POINT ( 'NONE',  ( 3.257655550456945548, 132.7023137178985337, 15.46528703574811736 ) ) ;
#21451 = VECTOR ( 'NONE', #30047, 1000.000000000000000 ) ;
#21452 = CARTESIAN_POINT ( 'NONE',  ( 18.00000000000000000, 5.196152422706630247, -9.468749998770952914 ) ) ;
#21453 = DIRECTION ( 'NONE',  ( -0.000000000000000000, -1.000000000000000000, -0.000000000000000000 ) ) ;
#21454 = ORIENTED_EDGE ( 'NONE', *, *, #12556, .T. ) ;
#21455 = CARTESIAN_POINT ( 'NONE',  ( 10.31873187879410736, 0.000000000000000000, -5.596874999385520688 ) ) ;
#21456 = ORIENTED_EDGE ( 'NONE', *, *, #211, .F. ) ;
#21457 = CARTESIAN_POINT ( 'NONE',  ( 27.24356964375000345, 195.5281250006145228, -3.336375036156643733E-15 ) ) ;
#21458 = CARTESIAN_POINT ( 'NONE',  ( -4.622313124798576922, 124.8351862821014748, -11.61527771782819762 ) ) ;
#21459 = CARTESIAN_POINT ( 'NONE',  ( 30.92186422678543778, 7.209453229046482114, 163.4074270530628894 ) ) ;
#21460 = CARTESIAN_POINT ( 'NONE',  ( -51.38169563604516554, 210.1155267958018271, 8.500000000000003553 ) ) ;
#21461 = CARTESIAN_POINT ( 'NONE',  ( 26.75643035624999655, 247.7593750006145399, -3.323476615752271268 ) ) ;
#21462 = DIRECTION ( 'NONE',  ( -1.558072081575740353E-16, -1.134704379232807653E-16, -1.000000000000000000 ) ) ;
#21463 = EDGE_CURVE ( 'NONE', #27062, #35303, #13870, .T. ) ;
#21464 = CARTESIAN_POINT ( 'NONE',  ( -43.46502896937849414, 213.8393509191290889, -2.350049139982142155 ) ) ;
#21465 =( BOUNDED_CURVE ( )  B_SPLINE_CURVE ( 2, ( #24123, #19006, #25043, #5135, #25235, #27889, #7809 ),
 .UNSPECIFIED., .F., .F. ) 
 B_SPLINE_CURVE_WITH_KNOTS ( ( 3, 2, 2, 3 ),
 ( 0.3260869565217380805, 0.3333333333333323711, 0.3405797101449267728, 0.3478260869565210633 ),
 .UNSPECIFIED. ) 
 CURVE ( )  GEOMETRIC_REPRESENTATION_ITEM ( )  RATIONAL_B_SPLINE_CURVE ( ( 1.000000000000019540, 0.8660254037844192787, 1.000000000000000000, 0.8660254037844387076, 1.000000000000000000, 0.8660254037844510311, 0.9999999999999876765 ) ) 
 REPRESENTATION_ITEM ( '' )  );
#21466 = CARTESIAN_POINT ( 'NONE',  ( 4.622313124798573369, 138.6351862821014720, 11.61527771782819940 ) ) ;
#21467 = CARTESIAN_POINT ( 'NONE',  ( 24.91612954363903043, -3.604726614523240613, 166.3984932299484569 ) ) ;
#21468 = ORIENTED_EDGE ( 'NONE', *, *, #33807, .F. ) ;
#21469 = CARTESIAN_POINT ( 'NONE',  ( 26.99999999999936051, -3.464101615138118984, -5.212500000000003020 ) ) ;
#21470 = CARTESIAN_POINT ( 'NONE',  ( 15.50000000000000533, 11.08981371789854897, -0.1745138560722452326 ) ) ;
#21471 = CIRCLE ( 'NONE', #25069, 27.00000000000000355 ) ;
#21472 = CARTESIAN_POINT ( 'NONE',  ( -43.86830436395490551, 209.8844732041983150, 8.500000000000003553 ) ) ;
#21473 = EDGE_CURVE ( 'NONE', #21578, #16024, #12700, .T. ) ;
#21474 = CARTESIAN_POINT ( 'NONE',  ( 9.500000000000005329, 109.3101862821014549, 0.1745138560725188748 ) ) ;
#21475 = CARTESIAN_POINT ( 'NONE',  ( 15.00000000000000178, 241.4874999999999829, 3.464101615137757051 ) ) ;
#21476 = CARTESIAN_POINT ( 'NONE',  ( 12.46528703574805874, 26.79768628210144144, 2.660918448318279950 ) ) ;
#21477 = CARTESIAN_POINT ( 'NONE',  ( 16.56230152254411436, 6.928203230275514990, -7.312500000000050626 ) ) ;
#21478 = UNCERTAINTY_MEASURE_WITH_UNIT (LENGTH_MEASURE( 1.000000000000000082E-05 ), #33793, 'distance_accuracy_value', 'NONE');
#21479 = ORIENTED_EDGE ( 'NONE', *, *, #33078, .T. ) ;
#21480 = CARTESIAN_POINT ( 'NONE',  ( -10.83675517735155047, 115.0601862821014691, -11.08355503943142750 ) ) ;
#21481 = CARTESIAN_POINT ( 'NONE',  ( -29.50000000000000711, 252.0000000000000000, -2.499999999999994671 ) ) ;
#21482 = CARTESIAN_POINT ( 'NONE',  ( 9.534712964251941258, 7.822686282101448896, -1.715153634034235708 ) ) ;
#21483 = CARTESIAN_POINT ( 'NONE',  ( -27.24356964374999635, 199.3906250006145342, 15.72908226750539384 ) ) ;
#21484 = CARTESIAN_POINT ( 'NONE',  ( 15.00000000000000000, 246.9062500012290400, 0.000000000000000000 ) ) ;
#21485 = CARTESIAN_POINT ( 'NONE',  ( 13.50000000000001421, 195.2000000000000171, 23.38268590217984055 ) ) ;
#21486 = CARTESIAN_POINT ( 'NONE',  ( 20.43890260697799377, -4.778814664990964189, -9.999999999999994671 ) ) ;
#21487 = CARTESIAN_POINT ( 'NONE',  ( 28.32508817407707014, 5.407089921784862696, 169.5446048129269059 ) ) ;
#21488 = EDGE_CURVE ( 'NONE', #36971, #1101, #1548, .T. ) ;
#21489 =( BOUNDED_CURVE ( )  B_SPLINE_CURVE ( 2, ( #20269, #11167, #22926, #8879, #34290, #34099, #19721 ),
 .UNSPECIFIED., .F., .F. ) 
 B_SPLINE_CURVE_WITH_KNOTS ( ( 3, 2, 2, 3 ),
 ( 0.3913043478260868624, 0.3985507246376802093, 0.4057971014492736672, 0.4130434782608670141 ),
 .UNSPECIFIED. ) 
 CURVE ( )  GEOMETRIC_REPRESENTATION_ITEM ( )  RATIONAL_B_SPLINE_CURVE ( ( 1.000000000000001998, 0.8660254037844367092, 1.000000000000000000, 0.8660254037844387076, 1.000000000000000000, 0.8660254037844858921, 0.9999999999999528155 ) ) 
 REPRESENTATION_ITEM ( '' )  );
#21490 = CARTESIAN_POINT ( 'NONE',  ( -2.064181346179062349, 72.90231371789855075, -9.465287035748106703 ) ) ;
#21491 = ORIENTED_EDGE ( 'NONE', *, *, #31566, .T. ) ;
#21492 = CARTESIAN_POINT ( 'NONE',  ( 18.00000000000000355, 244.7312500012290570, 5.196152422706632912 ) ) ;
#21493 = CARTESIAN_POINT ( 'NONE',  ( 2.660918448318003282, 77.50231371789855928, 12.46528703574811558 ) ) ;
#21494 = CARTESIAN_POINT ( 'NONE',  ( 10.31873187879410736, 0.000000000000000000, -2.896874999385512517 ) ) ;
#21495 = CARTESIAN_POINT ( 'NONE',  ( -56.70466238434234185, 244.2363183625454894, 7.500000000000000000 ) ) ;
#21496 = CARTESIAN_POINT ( 'NONE',  ( 18.12178482187499640, 4.985214923628404904, -3.928124999385496086 ) ) ;
#21497 = CARTESIAN_POINT ( 'NONE',  ( -11.48171059495408208, 51.91481371789855359, 4.944772684328421875 ) ) ;
#21498 = ORIENTED_EDGE ( 'NONE', *, *, #14680, .T. ) ;
#21499 = CARTESIAN_POINT ( 'NONE',  ( 20.99999999999999645, 6.646953231504538984, -7.453124999385467575 ) ) ;
#21500 = CARTESIAN_POINT ( 'NONE',  ( 21.00000000000000000, 244.0093750006145115, 6.646953231504538984 ) ) ;
#21501 = CARTESIAN_POINT ( 'NONE',  ( -12.53471296425194836, 21.62268628210144072, 2.311890736173176641 ) ) ;
#21502 = EDGE_CURVE ( 'NONE', #33575, #34897, #10454, .T. ) ;
#21503 = CARTESIAN_POINT ( 'NONE',  ( -43.66294563604516554, 214.6737587650350747, -4.842901733360248429 ) ) ;
#21504 = CARTESIAN_POINT ( 'NONE',  ( -53.36086230271183695, 213.1499508600178387, -5.686928522499747451 ) ) ;
#21505 = CARTESIAN_POINT ( 'NONE',  ( 30.57623723450533859, -6.928203230275506996, 159.4568924540549517 ) ) ;
#21506 = CARTESIAN_POINT ( 'NONE',  ( -11.48171059495408208, 88.71481371789855075, 4.944772684328421875 ) ) ;
#21507 = CARTESIAN_POINT ( 'NONE',  ( -42.08705436395490551, 206.7903428501026042, -3.378800118222489157 ) ) ;
#21508 = CARTESIAN_POINT ( 'NONE',  ( -59.50372103062156981, 216.5309553116391612, -1.626142955000564383 ) ) ;
#21509 = CARTESIAN_POINT ( 'NONE',  ( 15.24356964374999990, 3.323476615752268604, -7.490624999385497418 ) ) ;
#21510 = CYLINDRICAL_SURFACE ( 'NONE', #21642, 6.000000000000001776 ) ;
#21511 = CARTESIAN_POINT ( 'NONE',  ( 14.25334919248795451, 65.71481371789855075, -6.092822981423661410 ) ) ;
#21512 = CARTESIAN_POINT ( 'NONE',  ( -42.67336230271183695, 217.4189793300686233, 4.149950860017807663 ) ) ;
#21513 = CARTESIAN_POINT ( 'NONE',  ( 13.49999999999999645, 199.8499999999999943, -23.38268590217984766 ) ) ;
#21514 = CARTESIAN_POINT ( 'NONE',  ( 12.46528703574805874, 91.19768628210145778, 2.660918448318279950 ) ) ;
#21515 = CARTESIAN_POINT ( 'NONE',  ( -8.632099005475501130, 23.34768628210144570, -13.23911966647218996 ) ) ;
#21516 = DIRECTION ( 'NONE',  ( 1.000000000000000000, 0.000000000000000000, 0.000000000000000000 ) ) ;
#21517 = CARTESIAN_POINT ( 'NONE',  ( 15.00000000000000000, 244.2062500012290513, 0.000000000000000000 ) ) ;
#21518 = ORIENTED_EDGE ( 'NONE', *, *, #31251, .F. ) ;
#21519 = CARTESIAN_POINT ( 'NONE',  ( -13.04141134922759804, 41.17268628210143078, -8.927990412390657937 ) ) ;
#21520 = CARTESIAN_POINT ( 'NONE',  ( 27.24356964375000345, 197.3281250006145342, -3.336375036156643733E-15 ) ) ;
#21521 = CARTESIAN_POINT ( 'NONE',  ( 27.24356964375000700, 199.5968750006145456, 15.72908226750537075 ) ) ;
#21522 = DIRECTION ( 'NONE',  ( -0.000000000000000000, 1.000000000000000000, -0.000000000000000000 ) ) ;
#21523 = CARTESIAN_POINT ( 'NONE',  ( -38.32663769728824121, 204.3130714775002730, 3.149950860017883603 ) ) ;
#21524 = CARTESIAN_POINT ( 'NONE',  ( 25.36059234810526419, 3.464101615137711310, 168.6840780838932403 ) ) ;
#21525 = CARTESIAN_POINT ( 'NONE',  ( -10.49813415415989581, 22.77268628210143575, -7.228626920339068285 ) ) ;
#21526 = VECTOR ( 'NONE', #5094, 1000.000000000000000 ) ;
#21527 = CARTESIAN_POINT ( 'NONE',  ( 15.24356964374999990, 249.8218750006145399, -3.323476615752268604 ) ) ;
#21528 = CARTESIAN_POINT ( 'NONE',  ( -9.465287035748106703, 135.0023137178985166, 2.064181346179061460 ) ) ;
#21529 = CARTESIAN_POINT ( 'NONE',  ( 18.12178482187499640, 244.8343750006145285, -4.985214923628404904 ) ) ;
#21530 = VERTEX_POINT ( 'NONE', #11015 ) ;
#21531 = CARTESIAN_POINT ( 'NONE',  ( 20.99999999999999645, 185.0294372515228645, 0.000000000000000000 ) ) ;
#21532 = CARTESIAN_POINT ( 'NONE',  ( 10.49813415416005213, 139.0273137178985507, -7.228626920338837358 ) ) ;
#21533 = ADVANCED_FACE ( 'NONE', ( #30745 ), #36784, .F. ) ;
#21534 = CARTESIAN_POINT ( 'NONE',  ( 16.56230152254411081, 7.209453229046475009, -6.553124999385508964 ) ) ;
#21535 = CARTESIAN_POINT ( 'NONE',  ( 24.71676078210377625, 0.000000000000000000, 164.1196978580636028 ) ) ;
#21536 = CYLINDRICAL_SURFACE ( 'NONE', #21419, 27.00000000000000000 ) ;
#21537 = CARTESIAN_POINT ( 'NONE',  ( 13.49999999999999645, 197.1500000000000057, -23.38268590217984766 ) ) ;
#21538 = VERTEX_POINT ( 'NONE', #10829 ) ;
#21539 = CARTESIAN_POINT ( 'NONE',  ( 8.962234695871762469, 43.76018628210144357, -8.715434833791931624 ) ) ;
#21540 = ORIENTED_EDGE ( 'NONE', *, *, #3211, .T. ) ;
#21541 = EDGE_LOOP ( 'NONE', ( #33365, #9000, #4018, #34568 ) ) ;
#21542 = CARTESIAN_POINT ( 'NONE',  ( 15.24356964375000167, -3.323476615752272600, -1.453124999385472016 ) ) ;
#21543 = CARTESIAN_POINT ( 'NONE',  ( 26.99999999999999645, 249.4187500012290286, -3.464101615137755275 ) ) ;
#21544 = CARTESIAN_POINT ( 'NONE',  ( 36.75931086529713099, 7.347880794884117764E-16, 161.2874679718108553 ) ) ;
#21545 = CARTESIAN_POINT ( 'NONE',  ( 26.75643035624999655, -3.323476615752267715, -8.953124999385474680 ) ) ;
#21546 = CARTESIAN_POINT ( 'NONE',  ( -11.61527771782819940, 85.73518628210143788, 4.622313124798574258 ) ) ;
#21547 = CARTESIAN_POINT ( 'NONE',  ( 2.908627838312118019, 138.9226862821014663, 15.53471296425195369 ) ) ;
#21548 = EDGE_CURVE ( 'NONE', #28686, #22420, #13120, .T. ) ;
#21549 = CARTESIAN_POINT ( 'NONE',  ( -51.97544563604517265, 213.3788001182224718, 3.209657149897419348 ) ) ;
#21550 = AXIS2_PLACEMENT_3D ( 'NONE', #26162, #196, #3417 ) ;
#21551 = CARTESIAN_POINT ( 'NONE',  ( -4.500000000000001776, 227.8255434699758837, 2.500000000000000000 ) ) ;
#21552 = CARTESIAN_POINT ( 'NONE',  ( 34.19561101691670757, -5.196152422706629359, 166.4053843532510371 ) ) ;
#21553 = CARTESIAN_POINT ( 'NONE',  ( -10.49813415416004858, 134.4273137178985849, 7.228626920338839135 ) ) ;
#21554 = CARTESIAN_POINT ( 'NONE',  ( -50.59747103062156270, 213.3500491399821328, -5.571401726697985168 ) ) ;
#21555 = CARTESIAN_POINT ( 'NONE',  ( -54.15997103062156981, 217.3034525342668815, 4.350049139982096413 ) ) ;
#21556 = AXIS2_PLACEMENT_3D ( 'NONE', #15471, #863, #17572 ) ;
#21557 = ITEM_DEFINED_TRANSFORMATION ( 'NONE', 'NONE', #21446,  #17215 ) ;
#21558 = CARTESIAN_POINT ( 'NONE',  ( 26.75643035624999655, 3.323476615752271268, -0.4406249993854897129 ) ) ;
#21559 = CARTESIAN_POINT ( 'NONE',  ( 27.24356964375000700, 198.6406250006145058, 15.72908226750537075 ) ) ;
#21560 = CARTESIAN_POINT ( 'NONE',  ( 6.092822981423662299, 114.0148137178985763, 14.25334919248795096 ) ) ;
#21561 = CARTESIAN_POINT ( 'NONE',  ( -40.49627896937849414, 203.4690446883607535, -1.626142955000504209 ) ) ;
#21562 = VERTEX_POINT ( 'NONE', #13487 ) ;
#21563 = CARTESIAN_POINT ( 'NONE',  ( 7.228626920339068285, 34.27268628210144641, -10.49813415415989581 ) ) ;
#21564 = LINE ( 'NONE', #33109, #34088 ) ;
#21565 = DIRECTION ( 'NONE',  ( -1.000000000000000000, 0.000000000000000000, 0.000000000000000000 ) ) ;
#21566 = CARTESIAN_POINT ( 'NONE',  ( 37.52080268400803931, -3.604726614523238837, 167.1967110400642866 ) ) ;
#21567 = CARTESIAN_POINT ( 'NONE',  ( -13.23911966647218463, 103.8476862821014493, 8.632099005475506459 ) ) ;
#21568 = CARTESIAN_POINT ( 'NONE',  ( -56.33705436395489841, 205.3262412349647548, -4.842901733360204908 ) ) ;
#21569 = CARTESIAN_POINT ( 'NONE',  ( 22.80587116629411426, -3.604726614523235284, -3.103124999385563410 ) ) ;
#21570 = CARTESIAN_POINT ( 'NONE',  ( -6.840914352312096547, 39.16018628210144215, 6.594114490232313663 ) ) ;
#21571 = DIRECTION ( 'NONE',  ( 0.000000000000000000, 1.000000000000000000, 0.000000000000000000 ) ) ;
#21572 = CARTESIAN_POINT ( 'NONE',  ( -36.54538769728824121, 212.3930949314662371, -8.469044688360781947 ) ) ;
#21573 = CARTESIAN_POINT ( 'NONE',  ( 33.71516498491316582, -5.196152422706635576, 160.9138610787959465 ) ) ;
#21574 = CARTESIAN_POINT ( 'NONE',  ( 7.228626920339068285, 71.07268628210144357, -10.49813415415989581 ) ) ;
#21575 = CYLINDRICAL_SURFACE ( 'NONE', #34224, 4.899999999999999467 ) ;
#21576 = DIRECTION ( 'NONE',  ( -0.9925324990730152175, 0.1219804832088933616, 0.000000000000000000 ) ) ;
#21578 = VERTEX_POINT ( 'NONE', #24674 ) ;
#21577 = CARTESIAN_POINT ( 'NONE',  ( 8.843639120294328748, 44.33518628210144641, -3.474262827703334722 ) ) ;
#21579 = CARTESIAN_POINT ( 'NONE',  ( 26.99999999999999645, 7.347880794884117764E-16, -6.018749998770944742 ) ) ;
#21580 = VERTEX_POINT ( 'NONE', #33769 ) ;
#21581 = CARTESIAN_POINT ( 'NONE',  ( 20.00041297495047843, 5.668978411116867733, -10.14010147226207614 ) ) ;
#21582 = CARTESIAN_POINT ( 'NONE',  ( -69.00372103062157692, 216.5309553116391612, -1.626142955000564383 ) ) ;
#21583 = CARTESIAN_POINT ( 'NONE',  ( 24.59419801886489054, 0.000000000000000000, 162.7187990638720976 ) ) ;
#21584 = CARTESIAN_POINT ( 'NONE',  ( 24.81804784950121601, -3.464101615137761048, 162.4827660882720295 ) ) ;
#21585 = CARTESIAN_POINT ( 'NONE',  ( 23.99999999999999645, 246.2500000000000000, -5.196152422706631135 ) ) ;
#21586 = CARTESIAN_POINT ( 'NONE',  ( 0.000000000000000000, 200.0000000000000000, 0.000000000000000000 ) ) ;
#21587 = AXIS2_PLACEMENT_3D ( 'NONE', #27432, #27812, #36328 ) ;
#21588 = CARTESIAN_POINT ( 'NONE',  ( -4.622313124798826500, 78.36481371789855643, 11.61527771782809637 ) ) ;
#21589 = CARTESIAN_POINT ( 'NONE',  ( -7.228626920339070061, 103.2726862821014606, 10.49813415415989404 ) ) ;
#21590 = ORIENTED_EDGE ( 'NONE', *, *, #79, .F. ) ;
#21591 = ORIENTED_EDGE ( 'NONE', *, *, #31021, .T. ) ;
#21592 = CARTESIAN_POINT ( 'NONE',  ( -26.99999999999998934, 199.2500000012290116, 15.58845726811991561 ) ) ;
#21593 = CARTESIAN_POINT ( 'NONE',  ( -2.908627838312453306, 78.07731371789854791, 15.53471296425188797 ) ) ;
#21594 = CARTESIAN_POINT ( 'NONE',  ( 15.24356964375000167, -3.323476615752272600, -6.965624999385507721 ) ) ;
#21595 = CARTESIAN_POINT ( 'NONE',  ( 23.87821517812500005, 244.6093750006145342, 4.985214923628404016 ) ) ;
#21596 = CARTESIAN_POINT ( 'NONE',  ( -59.70163769728823411, 213.9548777149308592, -2.149950860017830756 ) ) ;
#21597 = CIRCLE ( 'NONE', #7062, 7.500000000000000000 ) ;
#21598 = CARTESIAN_POINT ( 'NONE',  ( 18.00000000000000355, -5.196152422706632912, -6.618749998770962151 ) ) ;
#21599 = CARTESIAN_POINT ( 'NONE',  ( 3.796722387233182339, 49.61481371789856354, 8.710071997420207879 ) ) ;
#21600 = CARTESIAN_POINT ( 'NONE',  ( 22.80587116629410360, 7.646167579472015790E-16, -7.565624999385539340 ) ) ;
#21601 = CARTESIAN_POINT ( 'NONE',  ( 9.465287035748106703, 121.2023137178985479, -2.064181346179063237 ) ) ;
#21602 = DIRECTION ( 'NONE',  ( 0.000000000000000000, 1.000000000000000000, 0.000000000000000000 ) ) ;
#21603 = CARTESIAN_POINT ( 'NONE',  ( 11.61527771782809637, 39.26481371789855501, 4.622313124798827388 ) ) ;
#21604 = CARTESIAN_POINT ( 'NONE',  ( 12.46528703574805874, 91.19768628210145778, 2.660918448318279950 ) ) ;
#21605 = CARTESIAN_POINT ( 'NONE',  ( 10.56230152254410903, 3.464101615137752166, -8.474999998771021836 ) ) ;
#21606 = CARTESIAN_POINT ( 'NONE',  ( 0.000000000000000000, 210.0000000000000284, 0.000000000000000000 ) ) ;
#21607 = CARTESIAN_POINT ( 'NONE',  ( 24.83115269446006934, 3.604726614523236616, 165.4272033993090076 ) ) ;
#21608 = CARTESIAN_POINT ( 'NONE',  ( 22.80587116629412847, -3.604726614523238837, -3.159374999385510474 ) ) ;
#21609 = CARTESIAN_POINT ( 'NONE',  ( 26.99999999999962341, -3.464101615137965773, -4.762500000000005507 ) ) ;
#21610 = CARTESIAN_POINT ( 'NONE',  ( -27.00000000000000355, 199.6625000012290343, 0.000000000000000000 ) ) ;
#21611 = CARTESIAN_POINT ( 'NONE',  ( 2.064181346179272847, 98.09768628210146346, -9.465287035748065847 ) ) ;
#21612 = CARTESIAN_POINT ( 'NONE',  ( 19.39230484541326049, 248.1638461906613884, -5.999999999999994671 ) ) ;
#21613 = CARTESIAN_POINT ( 'NONE',  ( -10.69584247140444866, 131.4476862821014436, 6.932735513423972762 ) ) ;
#21614 = CARTESIAN_POINT ( 'NONE',  ( 15.24356964375000167, 239.8843750006145399, 3.323476615752272600 ) ) ;
#21615 = VERTEX_POINT ( 'NONE', #10639 ) ;
#21616 = CARTESIAN_POINT ( 'NONE',  ( 30.96598682155142868, 7.209453229046475009, 163.9117506189718370 ) ) ;
#21617 = CARTESIAN_POINT ( 'NONE',  ( 23.87821517812499650, 4.985214923628404904, -3.890624999385472460 ) ) ;
#21618 = AXIS2_PLACEMENT_3D ( 'NONE', #13247, #27646, #4701 ) ;
#21619 = LINE ( 'NONE', #7215, #30178 ) ;
#21620 = DIRECTION ( 'NONE',  ( -0.000000000000000000, -0.000000000000000000, 1.000000000000000000 ) ) ;
#21621 = CARTESIAN_POINT ( 'NONE',  ( 28.35898146343970083, -5.196152422706638241, 168.5346827591855288 ) ) ;
#21622 = CARTESIAN_POINT ( 'NONE',  ( 13.50000000000001421, 199.3625000012290513, 23.38268590217984055 ) ) ;
#21623 = CARTESIAN_POINT ( 'NONE',  ( 23.87821517812499650, 242.9593750006145285, -4.985214923628404904 ) ) ;
#21624 = CARTESIAN_POINT ( 'NONE',  ( 13.44051670066911619, -5.407089921784859143, -1.415624999385550753 ) ) ;
#21625 = CARTESIAN_POINT ( 'NONE',  ( 9.534712964251900402, 11.37731371789854506, 1.715153634034445540 ) ) ;
#21626 = CARTESIAN_POINT ( 'NONE',  ( 5.778771075727756162E-15, 196.8218750006145683, 31.45816453501076637 ) ) ;
#21628 = VERTEX_POINT ( 'NONE', #22402 ) ;
#21627 = ORIENTED_EDGE ( 'NONE', *, *, #9607, .T. ) ;
#21629 = CARTESIAN_POINT ( 'NONE',  ( 18.12178482187500350, 247.1218750006145228, 4.985214923628407568 ) ) ;
#21630 = CARTESIAN_POINT ( 'NONE',  ( 10.49813415416005213, 28.62731371789854862, -7.228626920338837358 ) ) ;
#21631 = CARTESIAN_POINT ( 'NONE',  ( 15.24356964375000167, -3.323476615752272600, -1.003124999385444527 ) ) ;
#21632 = CARTESIAN_POINT ( 'NONE',  ( -10.83675517735179028, 124.9398137178985451, 11.08355503943118947 ) ) ;
#21633 = CARTESIAN_POINT ( 'NONE',  ( 26.99999999999999645, 7.347880794884117764E-16, -8.718749998770952914 ) ) ;
#21634 = ORIENTED_EDGE ( 'NONE', *, *, #36365, .F. ) ;
#21635 = CARTESIAN_POINT ( 'NONE',  ( 10.31873187879410736, 3.604726614523240613, -6.084374999385531169 ) ) ;
#21636 = ORIENTED_EDGE ( 'NONE', *, *, #6896, .F. ) ;
#21637 = CARTESIAN_POINT ( 'NONE',  ( -27.24356964374999990, 197.0656250006145171, -15.72908226750537786 ) ) ;
#21638 = CARTESIAN_POINT ( 'NONE',  ( 11.48171059495397728, 128.2851862821014493, 4.944772684328674117 ) ) ;
#21639 = CARTESIAN_POINT ( 'NONE',  ( 24.66936984698473623, 3.604726614523240613, 163.5780169909762094 ) ) ;
#21640 = CARTESIAN_POINT ( 'NONE',  ( -60.28794563604517975, 203.8621396198271043, 6.307003348498029460 ) ) ;
#21641 = CARTESIAN_POINT ( 'NONE',  ( 23.87821517812500005, 246.2968750006145058, 4.985214923628404016 ) ) ;
#21642 = AXIS2_PLACEMENT_3D ( 'NONE', #33054, #30212, #4237 ) ;
#21643 = CARTESIAN_POINT ( 'NONE',  ( 1.120210788295102201E-13, 196.7375000000000398, -27.00000000000000711 ) ) ;
#21644 = CARTESIAN_POINT ( 'NONE',  ( -48.21502896937850124, 213.8393509191290889, -2.350049139982142155 ) ) ;
#21645 = CARTESIAN_POINT ( 'NONE',  ( 36.63184559142159458, 7.347880794884125653E-16, 159.8305332246273167 ) ) ;
#21646 = CARTESIAN_POINT ( 'NONE',  ( 25.03052145599531997, 0.000000000000000000, 167.7059987711938902 ) ) ;
#21647 = ORIENTED_EDGE ( 'NONE', *, *, #6091, .F. ) ;
#21648 = CARTESIAN_POINT ( 'NONE',  ( -7.234628195640302017, 195.2549038117967086, 27.00000000000000711 ) ) ;
#21649 = CARTESIAN_POINT ( 'NONE',  ( 10.83675517735155225, 128.8601862821014663, 11.08355503943142573 ) ) ;
#21650 = CARTESIAN_POINT ( 'NONE',  ( -44.46205436395490551, 216.1378603801730094, 6.307003348497944195 ) ) ;
#21651 = CARTESIAN_POINT ( 'NONE',  ( 2.064181346179272847, 116.4976862821014549, -9.465287035748065847 ) ) ;
#21652 = FACE_OUTER_BOUND ( 'NONE', #8873, .T. ) ;
#21653 = CARTESIAN_POINT ( 'NONE',  ( 0.1745138560725515708, 15.01018628210143468, -12.50000000000000355 ) ) ;
#21654 = ADVANCED_FACE ( 'NONE', ( #7992 ), #19566, .F. ) ;
#21655 = CARTESIAN_POINT ( 'NONE',  ( 10.56230152254411436, -3.464101615137761048, -8.062500000000023093 ) ) ;
#21656 = ORIENTED_EDGE ( 'NONE', *, *, #5536, .F. ) ;
#21657 = CARTESIAN_POINT ( 'NONE',  ( -35.55580436395490551, 216.5000000000000000, 0.1155267958017343610 ) ) ;
#21658 = CARTESIAN_POINT ( 'NONE',  ( 0.1745138560725194299, 88.61018628210146630, -9.500000000000005329 ) ) ;
#21659 = DIRECTION ( 'NONE',  ( 0.08715574274765150453, 0.000000000000000000, 0.9961946980917461003 ) ) ;
#21660 = CARTESIAN_POINT ( 'NONE',  ( -9.534712964251895073, 135.5773137178985905, -1.715153634034446428 ) ) ;
#21661 = CARTESIAN_POINT ( 'NONE',  ( -13.62178482187498396, 198.0781250006145342, 23.59362340125808188 ) ) ;
#21662 = CARTESIAN_POINT ( 'NONE',  ( 15.00000000000000000, 245.0124999999999602, -3.464101615137752610 ) ) ;
#21663 = CARTESIAN_POINT ( 'NONE',  ( 27.24356964375000700, 198.2468750006145513, 15.72908226750537075 ) ) ;
#21664 = CARTESIAN_POINT ( 'NONE',  ( 19.56230152254412502, 5.196152422706637353, -5.550000000000054889 ) ) ;
#21665 = CARTESIAN_POINT ( 'NONE',  ( 20.99999999999999289, 244.0374999999999943, -5.999999999999997335 ) ) ;
#21666 = CARTESIAN_POINT ( 'NONE',  ( -8.843639120294245259, 71.46481371789856496, -3.474262827703533230 ) ) ;
#21667 = VERTEX_POINT ( 'NONE', #33397 ) ;
#21668 = CARTESIAN_POINT ( 'NONE',  ( 15.00000000000000000, 245.0687500012290627, -3.464101615137752166 ) ) ;
#21669 = CARTESIAN_POINT ( 'NONE',  ( -10.69584247140429412, 80.95231371789856212, -6.932735513424201024 ) ) ;
#21670 = CARTESIAN_POINT ( 'NONE',  ( 13.44051670066911441, -5.407089921784865361, -5.071874999385522997 ) ) ;
#21671 = CARTESIAN_POINT ( 'NONE',  ( -10.73304900139428675, 142.9999999999998010, 8.431259175847527487 ) ) ;
#21672 = CARTESIAN_POINT ( 'NONE',  ( 26.75643035624999655, 7.049594010296217766E-16, -5.428124999385497418 ) ) ;
#21673 = CARTESIAN_POINT ( 'NONE',  ( 4.622313124798831829, 46.16481371789854649, -11.61527771782809282 ) ) ;
#21674 = APPLICATION_CONTEXT ( 'automotive_design' ) ;
#21675 = ORIENTED_EDGE ( 'NONE', *, *, #25175, .T. ) ;
#21676 = CARTESIAN_POINT ( 'NONE',  ( 26.75643035624999655, 7.049594010296217766E-16, -7.115624999385477878 ) ) ;
#21677 = CARTESIAN_POINT ( 'NONE',  ( 15.24356964374999990, 245.2468750006145228, 0.000000000000000000 ) ) ;
#21678 = EDGE_CURVE ( 'NONE', #36019, #7808, #30414, .T. ) ;
#21679 = CARTESIAN_POINT ( 'NONE',  ( 4.944772684328679446, 24.78518628210143859, -11.48171059495397373 ) ) ;
#21680 =( BOUNDED_CURVE ( )  B_SPLINE_CURVE ( 2, ( #20122, #26167, #23335, #5888, #11396, #26540, #17466, #25983, #26352, #20502, #29002, #11579, #11954, #6070, #29191, #3233, #17847, #388, #23712, #23523, #6270, #29385, #31670, #3422, #5699, #570, #12137, #35253, #9307, #20879, #32418, #6462, #2672, #14247, #25796, #22968, #17279, #28820, #14428, #13, #21442, #15747, #12898, #32607, #9493, #24462, #3984, #21257, #36011, #32796, #35445, #12329, #18604, #7221, #21811, #18793, #21069, #30335, #10050, #6646, #6832, #3614, #29956, #24642, #30147, #15939, #29576, #4358, #13087, #24278, #18222, #15370, #23903, #33364, #3793, #15180, #26727, #15558, #7400, #18408, #29762, #21626, #761, #10236, #33177, #26920, #27487, #950, #12525, #1513, #12706, #27115, #24088, #35633, #1138, #35822, #9680, #36192, #9863, #32984, #7037, #4176, #27298, #1329, #10608, #1701, #36566, #28045, #25204, #5106, #22187, #33735, #16124, #22745, #30714, #19354, #34294, #2078, #27675, #19164, #22372, #13273, #16871, #36757, #7776, #25011, #24826, #7590, #10425, #36379, #30894, #4734, #13460, #21999, #31083 ),
 .UNSPECIFIED., .F., .F. ) 
 B_SPLINE_CURVE_WITH_KNOTS ( ( 3, 2, 2, 2, 2, 2, 2, 2, 2, 2, 2, 2, 2, 2, 2, 2, 2, 2, 2, 2, 2, 2, 2, 2, 2, 2, 2, 2, 2, 2, 2, 2, 2, 2, 2, 2, 2, 2, 2, 2, 2, 2, 2, 2, 2, 2, 2, 2, 2, 2, 2, 2, 2, 2, 2, 2, 2, 2, 2, 2, 2, 2, 2, 2, 2, 2, 2, 3 ),
 ( 0.000000000000000000, 0.01388888888888888812, 0.02777777777777777624, 0.04166666666666666435, 0.05555555555555555247, 0.06944444444444444753, 0.08333333333333332871, 0.09722222222222222376, 0.1111111111111111049, 0.1250000000000000000, 0.1388888888888888951, 0.1527777777777777901, 0.1666666666666666574, 0.1805555555555555525, 0.1944444444444444475, 0.2083333333333333426, 0.2222222222222222099, 0.2361111111111111049, 0.2500000000000000000, 0.2638888888888888951, 0.2777777777777777901, 0.2916666666666666852, 0.3055555555555555802, 0.3194444444444444198, 0.3333333333333333148, 0.3472222222222222099, 0.3611111111111111049, 0.3750000000000000000, 0.3888888888888888951, 0.4027777777777777901, 0.4166666666666666852, 0.4305555555555555802, 0.4444444444444444198, 0.4583333333333333148, 0.4722222222222222099, 0.4861111111111111049, 0.5000000000000000000, 0.5138888888888888395, 0.5277777777777777901, 0.5416666666666666297, 0.5555555555555555802, 0.5694444444444444198, 0.5833333333333333703, 0.5972222222222222099, 0.6111111111111111605, 0.6250000000000001110, 0.6388888888888888395, 0.6527777777777777901, 0.6666666666666666297, 0.6805555555555555802, 0.6944444444444444198, 0.7083333333333333703, 0.7222222222222222099, 0.7361111111111111605, 0.7500000000000000000, 0.7638888888888888395, 0.7777777777777777901, 0.7916666666666666297, 0.8055555555555555802, 0.8194444444444444198, 0.8333333333333333703, 0.8472222222222222099, 0.8611111111111111605, 0.8749999999999998890, 0.8888888888888888395, 0.9027777777777777901, 0.9166666666666666297, 0.9258785558164617235 ),
 .UNSPECIFIED. ) 
 CURVE ( )  GEOMETRIC_REPRESENTATION_ITEM ( )  RATIONAL_B_SPLINE_CURVE ( ( 1.000000000000000000, 0.8660254037844387076, 1.000000000000000000, 0.8660254037844387076, 1.000000000000000000, 0.8660254037844387076, 1.000000000000000000, 0.8660254037844387076, 1.000000000000000000, 0.8660254037844387076, 1.000000000000000000, 0.8660254037844387076, 1.000000000000000000, 0.8660254037844387076, 1.000000000000000000, 0.8660254037844387076, 1.000000000000000000, 0.8660254037844387076, 1.000000000000000000, 0.8660254037844387076, 1.000000000000000000, 0.8660254037844387076, 1.000000000000000000, 0.8660254037844387076, 1.000000000000000000, 0.8660254037844387076, 1.000000000000000000, 0.8660254037844387076, 1.000000000000000000, 0.8660254037844387076, 1.000000000000000000, 0.8660254037844387076, 1.000000000000000000, 0.8660254037844387076, 1.000000000000000000, 0.8660254037844387076, 1.000000000000000000, 0.8660254037844387076, 1.000000000000000000, 0.8660254037844387076, 1.000000000000000000, 0.8660254037844387076, 1.000000000000000000, 0.8660254037844387076, 1.000000000000000000, 0.8660254037844387076, 1.000000000000000000, 0.8660254037844387076, 1.000000000000000000, 0.8660254037844387076, 1.000000000000000000, 0.8660254037844387076, 1.000000000000000000, 0.8660254037844387076, 1.000000000000000000, 0.8660254037844387076, 1.000000000000000000, 0.8660254037844387076, 1.000000000000000000, 0.8660254037844387076, 1.000000000000000000, 0.8660254037844387076, 1.000000000000000000, 0.8660254037844387076, 1.000000000000000000, 0.8660254037844387076, 1.000000000000000000, 0.8660254037844387076, 1.000000000000000000, 0.8660254037844387076, 1.000000000000000000, 0.8660254037844387076, 1.000000000000000000, 0.8660254037844387076, 1.000000000000000000, 0.8660254037844387076, 1.000000000000000000, 0.8660254037844387076, 1.000000000000000000, 0.8660254037844387076, 1.000000000000000000, 0.8660254037844387076, 1.000000000000000000, 0.8660254037844387076, 1.000000000000000000, 0.8660254037844387076, 1.000000000000000000, 0.8660254037844387076, 1.000000000000000000, 0.8660254037844387076, 1.000000000000000000, 0.8660254037844387076, 1.000000000000000000, 0.8660254037844387076, 1.000000000000000000, 0.8660254037844387076, 1.000000000000000000, 0.8660254037844387076, 1.000000000000000000, 0.8660254037844387076, 1.000000000000000000, 0.8660254037844387076, 1.000000000000000000, 0.8660254037844387076, 1.000000000000000000, 0.8660254037844387076, 1.000000000000000000, 0.8660254037844387076, 1.000000000000000000, 0.8660254037844387076, 1.000000000000000000, 0.8660254037844387076, 1.000000000000000000, 0.8660254037844387076, 1.000000000000000000, 0.8660254037844387076, 1.000000000000000000, 0.8660254037844387076, 1.000000000000000000, 0.8660254037844387076, 1.000000000000000000, 0.8660254037844387076, 1.000000000000000000, 0.8660254037844387076, 1.000000000000000000, 0.8660254037844387076, 1.000000000000000000, 0.8660254037844387076, 1.000000000000000000, 0.8660254037844387076, 1.000000000000000000, 0.8660254037844387076, 1.000000000000000000, 0.9111405426957062126, 0.9401542251575389919 ) ) 
 REPRESENTATION_ITEM ( '' )  );
#21681 = CARTESIAN_POINT ( 'NONE',  ( -43.06919563604516554, 216.5000000000000000, -0.1155267958017906493 ) ) ;
#21682 = CARTESIAN_POINT ( 'NONE',  ( -53.95461230271181563, 208.1428034533959135, -6.469044688360754414 ) ) ;
#21683 = SHAPE_DEFINITION_REPRESENTATION ( #34665, #4304 ) ;
#21684 = CARTESIAN_POINT ( 'NONE',  ( 27.68897169117423829, 5.196152422706630247, 160.8764360188296223 ) ) ;
#21685 = CARTESIAN_POINT ( 'NONE',  ( -12.53471296425189152, 71.17731371789855643, -2.311890736173453753 ) ) ;
#21686 = CARTESIAN_POINT ( 'NONE',  ( -47.23288769728824121, 205.5309553116392465, -1.321298161741839117 ) ) ;
#21687 = CARTESIAN_POINT ( 'NONE',  ( -62.86830436395490551, 209.8844732041982581, 6.500000000000000888 ) ) ;
#21688 = VECTOR ( 'NONE', #20574, 1000.000000000000000 ) ;
#21689 = CARTESIAN_POINT ( 'NONE',  ( 27.00000000000047251, 3.464101615137479495, -6.937499999999990230 ) ) ;
#21690 = DIRECTION ( 'NONE',  ( -0.000000000000000000, -1.000000000000000000, -0.000000000000000000 ) ) ;
#21691 = CARTESIAN_POINT ( 'NONE',  ( 5.770363421894130873, 55.36481371789856354, -14.38691631536193860 ) ) ;
#21692 = CARTESIAN_POINT ( 'NONE',  ( -46.03794563604517975, 203.8621396198271043, 6.307003348498029460 ) ) ;
#21693 = CARTESIAN_POINT ( 'NONE',  ( 0.000000000000000000, 210.0000000000000284, 0.000000000000000000 ) ) ;
#21694 = CARTESIAN_POINT ( 'NONE',  ( 12.53471296425194836, 63.02268628210145351, -2.311890736173178418 ) ) ;
#21695 = CARTESIAN_POINT ( 'NONE',  ( 15.46528703574804986, 35.99768628210143362, 3.257655550457285720 ) ) ;
#21696 = CARTESIAN_POINT ( 'NONE',  ( 16.56230152254410726, 0.000000000000000000, -10.00000000000000000 ) ) ;
#21697 =( BOUNDED_CURVE ( )  B_SPLINE_CURVE ( 2, ( #6715, #20753, #27363, #21135, #18287, #32299, #1015 ),
 .UNSPECIFIED., .F., .F. ) 
 B_SPLINE_CURVE_WITH_KNOTS ( ( 3, 2, 2, 3 ),
 ( 0.2173913043478263030, 0.2246376811594205936, 0.2318840579710149119, 0.2391304347826092025 ),
 .UNSPECIFIED. ) 
 CURVE ( )  GEOMETRIC_REPRESENTATION_ITEM ( )  RATIONAL_B_SPLINE_CURVE ( ( 0.9999999999999958922, 0.8660254037844428154, 1.000000000000000000, 0.8660254037844387076, 1.000000000000000000, 0.8660254037844294928, 1.000000000000009326 ) ) 
 REPRESENTATION_ITEM ( '' )  );
#21698 = CYLINDRICAL_SURFACE ( 'NONE', #25246, 6.000000000000001776 ) ;
#21699 = VERTEX_POINT ( 'NONE', #25603 ) ;
#21700 = CIRCLE ( 'NONE', #31376, 7.500000000000000000 ) ;
#21701 = CARTESIAN_POINT ( 'NONE',  ( 3.257655550457285720, 24.49768628210144072, -15.46528703574804986 ) ) ;
#21702 = CARTESIAN_POINT ( 'NONE',  ( 27.24356964375000700, 198.1906250006145740, 15.72908226750537075 ) ) ;
#21703 = CARTESIAN_POINT ( 'NONE',  ( 10.56230152254410903, 0.000000000000000000, -0.7874999987710074034 ) ) ;
#21704 = CARTESIAN_POINT ( 'NONE',  ( 28.12366095802104127, -5.196152422706638241, 165.8449570743377990 ) ) ;
#21705 = CARTESIAN_POINT ( 'NONE',  ( -39.11830436395489841, 209.8844732041982581, 6.500000000000000888 ) ) ;
#21706 = CARTESIAN_POINT ( 'NONE',  ( -47.00000000000000711, 244.5000000000000000, 5.000000000000000000 ) ) ;
#21707 = CARTESIAN_POINT ( 'NONE',  ( 11.48171059495397728, 17.88518628210143646, 4.944772684328674117 ) ) ;
#21708 = CARTESIAN_POINT ( 'NONE',  ( -69.00000000000002842, 210.0000000000000000, 0.000000000000000000 ) ) ;
#21709 = CARTESIAN_POINT ( 'NONE',  ( -3.796722387233185003, 127.8148137178985735, -8.710071997420207879 ) ) ;
#21710 = CARTESIAN_POINT ( 'NONE',  ( 26.75643035624999655, 244.2343750006145342, -7.049594010296217766E-16 ) ) ;
#21711 = EDGE_LOOP ( 'NONE', ( #7493, #7048 ) ) ;
#21712 = CARTESIAN_POINT ( 'NONE',  ( 15.00000000000000000, 249.5687500012290627, -3.464101615137752610 ) ) ;
#21713 = CARTESIAN_POINT ( 'NONE',  ( 34.12043918868973691, 5.196152422706637353, 165.5461664249225748 ) ) ;
#21714 = CARTESIAN_POINT ( 'NONE',  ( 2.660918448318003282, 132.7023137178985621, 12.46528703574811558 ) ) ;
#21715 = CARTESIAN_POINT ( 'NONE',  ( 22.80587116629410716, 3.604726614523238837, -6.628124999385534899 ) ) ;
#21716 = CARTESIAN_POINT ( 'NONE',  ( 24.72002912245681117, -3.604726614523240613, 164.1570551592420486 ) ) ;
#21717 = FACE_OUTER_BOUND ( 'NONE', #29264, .T. ) ;
#21718 = CARTESIAN_POINT ( 'NONE',  ( -27.00000000000000355, 198.6500000000000341, 0.000000000000000000 ) ) ;
#21719 = ORIENTED_EDGE ( 'NONE', *, *, #18149, .F. ) ;
#21720 = CARTESIAN_POINT ( 'NONE',  ( 8.962234695871762469, 25.36018628210144499, -8.715434833791931624 ) ) ;
#21721 = VERTEX_POINT ( 'NONE', #6061 ) ;
#21722 = AXIS2_PLACEMENT_3D ( 'NONE', #2055, #22724, #10587 ) ;
#21723 = VERTEX_POINT ( 'NONE', #2480 ) ;
#21724 = DIRECTION ( 'NONE',  ( 1.000000000000000000, -0.000000000000000000, -0.000000000000000000 ) ) ;
#21725 = CARTESIAN_POINT ( 'NONE',  ( 26.75643035624999655, 3.323476615752271268, -0.7781249993854945091 ) ) ;
#21726 = CARTESIAN_POINT ( 'NONE',  ( 19.56230152254412147, -5.196152422706635576, -9.300000000000057554 ) ) ;
#21727 = CARTESIAN_POINT ( 'NONE',  ( 36.76257920564959392, 3.464101615138092782, 161.3248252729893579 ) ) ;
#21728 = CARTESIAN_POINT ( 'NONE',  ( 18.12178482187500350, -4.985214923628407568, -7.715624999385467753 ) ) ;
#21729 = CARTESIAN_POINT ( 'NONE',  ( -2.311890736173176641, 79.12268628210145494, -12.53471296425194836 ) ) ;
#21730 = CARTESIAN_POINT ( 'NONE',  ( 3.257655550457285720, 134.8976862821014606, -15.46528703574804986 ) ) ;
#21731 = CARTESIAN_POINT ( 'NONE',  ( 36.75604252494468227, -3.464101615137414214, 161.2501106706323242 ) ) ;
#21732 = CARTESIAN_POINT ( 'NONE',  ( 15.00000000000000000, 243.7187500012290968, -3.464101615137752610 ) ) ;
#21733 = CARTESIAN_POINT ( 'NONE',  ( -48.80877896937850124, 211.0902445701383101, -4.530955311639234040 ) ) ;
#21734 = CARTESIAN_POINT ( 'NONE',  ( 20.99999999999999645, 185.0294372515228645, 0.000000000000000000 ) ) ;
#21735 = CARTESIAN_POINT ( 'NONE',  ( 34.15639093268026016, -5.196152422706629359, 165.9570967391097440 ) ) ;
#21736 = CARTESIAN_POINT ( 'NONE',  ( -10.49813415416004858, 143.6273137178986019, 7.228626920338839135 ) ) ;
#21737 = CARTESIAN_POINT ( 'NONE',  ( -41.09747103062156981, 213.3500491399821328, -5.571401726697985168 ) ) ;
#21738 = CARTESIAN_POINT ( 'NONE',  ( -55.94122103062156981, 207.8379586601371329, -8.530955311639223382 ) ) ;
#21739 = EDGE_CURVE ( 'NONE', #7058, #32512, #5810, .T. ) ;
#21740 = CONTEXT_DEPENDENT_SHAPE_REPRESENTATION ( #26240, #11669 ) ;
#21741 = CARTESIAN_POINT ( 'NONE',  ( 26.75643035624999655, 7.049594010296217766E-16, -1.378124999385471616 ) ) ;
#21742 = CARTESIAN_POINT ( 'NONE',  ( -27.24356964375000345, 198.4531250006145342, 0.000000000000000000 ) ) ;
#21743 = CARTESIAN_POINT ( 'NONE',  ( 2.908627838312458636, 119.4773137178985678, -15.53471296425188442 ) ) ;
#21744 = CARTESIAN_POINT ( 'NONE',  ( -44.65252896937850835, 206.6499508600178387, -5.571401726697954970 ) ) ;
#21745 = EDGE_LOOP ( 'NONE', ( #37270, #3331, #34586, #27323 ) ) ;
#21746 = LINE ( 'NONE', #7337, #16233 ) ;
#21747 = DIRECTION ( 'NONE',  ( 0.08715574274765150453, 0.000000000000000000, 0.9961946980917461003 ) ) ;
#21748 = CARTESIAN_POINT ( 'NONE',  ( -4.694659320240884604E-14, 197.8625000000000114, 27.00000000000000000 ) ) ;
#21749 = CARTESIAN_POINT ( 'NONE',  ( 31.11796464796764994, 7.209453229046482114, 165.6488651237693261 ) ) ;
#21750 = CARTESIAN_POINT ( 'NONE',  ( -14.25334919248782306, 96.08518628210146062, -6.092822981423979378 ) ) ;
#21751 = CARTESIAN_POINT ( 'NONE',  ( -57.52455436395489130, 205.1570982666397640, 4.673758765035199048 ) ) ;
#21752 = ADVANCED_FACE ( 'NONE', ( #8367 ), #22773, .T. ) ;
#21753 = CARTESIAN_POINT ( 'NONE',  ( 19.68408634441910721, -5.407089921784855591, -3.140624999385555061 ) ) ;
#21754 = CARTESIAN_POINT ( 'NONE',  ( -3.796722387233375073, 38.58518628210143930, 8.710071997420127943 ) ) ;
#21755 = CARTESIAN_POINT ( 'NONE',  ( 19.56230152254412502, -5.196152422706635576, -7.500000000000062172 ) ) ;
#21756 = CARTESIAN_POINT ( 'NONE',  ( -32.38913769728823411, 205.8500491399820760, -7.418979330068584233 ) ) ;
#21757 = ADVANCED_FACE ( 'NONE', ( #191 ), #29182, .T. ) ;
#21758 = CYLINDRICAL_SURFACE ( 'NONE', #15303, 5.999999999999998224 ) ;
#21759 = CARTESIAN_POINT ( 'NONE',  ( -4.622313124798576922, 69.63518628210145778, -11.61527771782819762 ) ) ;
#21760 = CARTESIAN_POINT ( 'NONE',  ( 16.83757916490470663, -4.525028440652736350, -7.983280259209641905 ) ) ;
#21761 = CARTESIAN_POINT ( 'NONE',  ( 7.234628195640322446, 199.2325961894323711, 26.99999999999999645 ) ) ;
#21763 = CARTESIAN_POINT ( 'NONE',  ( 22.80587116629411781, 7.646167579472024665E-16, -0.4218749993855352987 ) ) ;
#21762 = CARTESIAN_POINT ( 'NONE',  ( -5.529263428287477744, 38.87268628210144072, 7.954856959092191815 ) ) ;
#21764 = CARTESIAN_POINT ( 'NONE',  ( 13.50000000000001421, 198.4625000012290172, 23.38268590217984055 ) ) ;
#21765 = ORIENTED_EDGE ( 'NONE', *, *, #26065, .T. ) ;
#21766 = CARTESIAN_POINT ( 'NONE',  ( 21.00000000000000000, 6.928203230275506996, -2.812499999999997335 ) ) ;
#21767 = CARTESIAN_POINT ( 'NONE',  ( 37.01420992928731835, 7.646167579472024665E-16, 161.4063293574060083 ) ) ;
#21768 = CARTESIAN_POINT ( 'NONE',  ( 27.77068019989305370, -5.196152422706638241, 161.8103685470662469 ) ) ;
#21769 = CARTESIAN_POINT ( 'NONE',  ( 23.99999999999999645, 244.9000000000000057, -5.196152422706631135 ) ) ;
#21770 = CARTESIAN_POINT ( 'NONE',  ( 3.306546357697853733E-15, 202.0000000000000000, 27.00000000000000000 ) ) ;
#21771 = EDGE_CURVE ( 'NONE', #1229, #13971, #29486, .T. ) ;
#21772 = CARTESIAN_POINT ( 'NONE',  ( 7.228626920338837358, 86.12731371789855928, 10.49813415416005036 ) ) ;
#21773 = CARTESIAN_POINT ( 'NONE',  ( 4.944772684328679446, 79.98518628210145209, -11.48171059495397373 ) ) ;
#21774 = VERTEX_POINT ( 'NONE', #37158 ) ;
#21775 = VERTEX_POINT ( 'NONE', #8917 ) ;
#21776 = CARTESIAN_POINT ( 'NONE',  ( -27.00000000000000355, 197.8250000012290286, -15.58845726811989429 ) ) ;
#21777 = CARTESIAN_POINT ( 'NONE',  ( 26.99999999999940314, 3.464101615138096335, -1.087499999999968825 ) ) ;
#21778 = CARTESIAN_POINT ( 'NONE',  ( 0.1745138560722461762, 59.38981371789856212, 15.50000000000000533 ) ) ;
#21779 = CARTESIAN_POINT ( 'NONE',  ( 21.00000000000000000, -6.646953231504538984, -7.340624999385477523 ) ) ;
#21780 = CARTESIAN_POINT ( 'NONE',  ( 23.87821517812500005, 245.0593750006145228, 4.985214923628404016 ) ) ;
#21781 = CARTESIAN_POINT ( 'NONE',  ( -52.18080436395490551, 205.4999999999999716, -0.1155267958017894420 ) ) ;
#21782 = CYLINDRICAL_SURFACE ( 'NONE', #13741, 7.500000000000000000 ) ;
#21783 = CARTESIAN_POINT ( 'NONE',  ( -6.594114490232462877, 60.53981371789856070, 6.840914352311949109 ) ) ;
#21784 = CARTESIAN_POINT ( 'NONE',  ( 19.68408634441910721, -5.407089921784855591, -7.640624999385531524 ) ) ;
#21785 = CARTESIAN_POINT ( 'NONE',  ( 8.843639120294245259, 122.0648137178985877, 3.474262827703527901 ) ) ;
#21786 = CARTESIAN_POINT ( 'NONE',  ( 13.62178482187499640, 199.7093750006145285, -23.59362340125807123 ) ) ;
#21787 = CARTESIAN_POINT ( 'NONE',  ( -6.932735513424201912, 32.65231371789854364, 10.69584247140429412 ) ) ;
#21788 = EDGE_CURVE ( 'NONE', #13971, #21667, #20239, .T. ) ;
#21789 = CARTESIAN_POINT ( 'NONE',  ( 4.944772684328679446, 89.18518628210145494, -11.48171059495397373 ) ) ;
#21790 = CARTESIAN_POINT ( 'NONE',  ( 10.56230152254410903, -3.464101615137757051, -7.499999998771006204 ) ) ;
#21791 = DIRECTION ( 'NONE',  ( 0.000000000000000000, 0.000000000000000000, 1.000000000000000000 ) ) ;
#21792 = CARTESIAN_POINT ( 'NONE',  ( 30.84832656884210067, 7.209453229046475009, 162.5668877765479863 ) ) ;
#21793 = CARTESIAN_POINT ( 'NONE',  ( 10.31873187879411091, 3.604726614523240613, -6.534374999385494043 ) ) ;
#21794 = CARTESIAN_POINT ( 'NONE',  ( -4.694659320240884604E-14, 197.8625000000000114, 27.00000000000000000 ) ) ;
#21795 = CARTESIAN_POINT ( 'NONE',  ( 20.99999999999999645, -6.928203230275506996, -3.881249998770961440 ) ) ;
#21796 = LINE ( 'NONE', #33349, #13932 ) ;
#21797 = CARTESIAN_POINT ( 'NONE',  ( -3.474262827703337830, 97.23518628210146630, -8.843639120294326972 ) ) ;
#21798 = DIRECTION ( 'NONE',  ( 0.08715574274765150453, 0.000000000000000000, 0.9961946980917461003 ) ) ;
#21799 = EDGE_CURVE ( 'NONE', #19165, #9189, #3999, .T. ) ;
#21800 = CARTESIAN_POINT ( 'NONE',  ( 4.944772684328679446, 135.1851862821014549, -11.48171059495397373 ) ) ;
#21801 = CARTESIAN_POINT ( 'NONE',  ( -10.41470757995802643, 142.9999999999999716, 3.937110085335259413 ) ) ;
#21802 = CARTESIAN_POINT ( 'NONE',  ( 15.24356964374999990, 240.7468750006144944, 0.000000000000000000 ) ) ;
#21803 = VERTEX_POINT ( 'NONE', #17790 ) ;
#21804 = CARTESIAN_POINT ( 'NONE',  ( 37.13677269252619340, 7.646167579472015790E-16, 162.8072281515975135 ) ) ;
#21805 = CARTESIAN_POINT ( 'NONE',  ( 15.24356964375000167, -3.323476615752272600, -5.053124999385469884 ) ) ;
#21806 = CARTESIAN_POINT ( 'NONE',  ( 13.62178482187499640, 197.4593750006145285, -23.59362340125807123 ) ) ;
#21807 = CARTESIAN_POINT ( 'NONE',  ( 25.36386068845838082, 0.000000000000000000, 168.7214353850716293 ) ) ;
#21808 = CARTESIAN_POINT ( 'NONE',  ( 36.66779733530574958, -3.464101615137326728, 160.2414635375900787 ) ) ;
#21809 = CARTESIAN_POINT ( 'NONE',  ( 18.12178482187500350, 242.7343750006145342, 4.985214923628407568 ) ) ;
#21810 = CARTESIAN_POINT ( 'NONE',  ( -8.962234695871565293, 136.4398137178985735, -8.715434833792128799 ) ) ;
#21811 = CARTESIAN_POINT ( 'NONE',  ( 27.24356964375000345, 197.8343750006145569, -3.336375036156643733E-15 ) ) ;
#21812 = VECTOR ( 'NONE', #977, 1000.000000000000000 ) ;
#21814 = VERTEX_POINT ( 'NONE', #29523 ) ;
#21813 = ORIENTED_EDGE ( 'NONE', *, *, #34811, .T. ) ;
#21815 = CARTESIAN_POINT ( 'NONE',  ( 26.75643035624999655, 243.6343750006145115, 3.323476615752267715 ) ) ;
#21816 = CARTESIAN_POINT ( 'NONE',  ( -11.61527771782809282, 34.66481371789854649, -4.622313124798832717 ) ) ;
#21817 = CARTESIAN_POINT ( 'NONE',  ( 21.00000000000000000, -6.646953231504538984, -4.078124999385484450 ) ) ;
#21818 = CARTESIAN_POINT ( 'NONE',  ( -14.25334919248795096, 107.1148137178985564, 6.092822981423662299 ) ) ;
#21819 = CARTESIAN_POINT ( 'NONE',  ( -47.00000000000000711, 244.5000000000000000, -2.499999999999997780 ) ) ;
#21820 = CARTESIAN_POINT ( 'NONE',  ( 23.99999999999999645, 5.196152422706631135, -8.643749998770960730 ) ) ;
#21821 = ORIENTED_EDGE ( 'NONE', *, *, #15154, .T. ) ;
#21822 = CARTESIAN_POINT ( 'NONE',  ( 10.31873187879410736, 0.000000000000000000, -6.046874999385526195 ) ) ;
#21823 = VERTEX_POINT ( 'NONE', #27063 ) ;
#21824 = CARTESIAN_POINT ( 'NONE',  ( 13.62178482187501416, 196.3531250006145115, 23.59362340125806767 ) ) ;
#21825 = CARTESIAN_POINT ( 'NONE',  ( 10.69584247140445221, 126.8476862821014635, -6.932735513423970097 ) ) ;
#21826 = CARTESIAN_POINT ( 'NONE',  ( 22.56230152254411792, 7.347880794884125653E-16, -6.525000000000058975 ) ) ;
#21827 = CARTESIAN_POINT ( 'NONE',  ( 24.51902619074504130, -3.604726614523244610, 161.8595811367679573 ) ) ;
#21828 = CARTESIAN_POINT ( 'NONE',  ( -49.79836230271183695, 202.5810206699313767, -4.149950860017804111 ) ) ;
#21829 = CARTESIAN_POINT ( 'NONE',  ( 23.87821517812500005, 246.7468750006145228, 4.985214923628404016 ) ) ;
#21830 = CARTESIAN_POINT ( 'NONE',  ( 26.99999999999999645, 240.3250000000000171, -7.347880794884117764E-16 ) ) ;
#21831 = CARTESIAN_POINT ( 'NONE',  ( -44.65252896937850835, 207.6499508600178387, -3.839350919129087547 ) ) ;
#21832 = CARTESIAN_POINT ( 'NONE',  ( 12.50000000000000355, 136.9101862821014777, 0.1745138560725507937 ) ) ;
#21833 = CARTESIAN_POINT ( 'NONE',  ( 10.56230152254411436, 3.464101615137752166, -0.8249999987710000537 ) ) ;
#21834 = EDGE_LOOP ( 'NONE', ( #14859, #17137, #6859, #18223 ) ) ;
#21835 = CARTESIAN_POINT ( 'NONE',  ( -26.99999999999999645, 195.2000000012290286, 15.58845726811991561 ) ) ;
#21836 = AXIS2_PLACEMENT_3D ( 'NONE', #34696, #8743, #32231 ) ;
#21837 =( NAMED_UNIT ( * ) PLANE_ANGLE_UNIT ( ) SI_UNIT ( $, .RADIAN. ) );
#21838 = CARTESIAN_POINT ( 'NONE',  ( 8.632099005475504683, 110.7476862821014691, 13.23911966647218996 ) ) ;
#21839 = CARTESIAN_POINT ( 'NONE',  ( -8.843639120294326972, 113.3351862821014606, 3.474262827703335166 ) ) ;
#21840 = CARTESIAN_POINT ( 'NONE',  ( 23.99999999999999645, 242.7062500012290513, -5.196152422706631135 ) ) ;
#21841 = CARTESIAN_POINT ( 'NONE',  ( 4.944772684328679446, 6.385186282101440014, -11.48171059495397373 ) ) ;
#21842 = CARTESIAN_POINT ( 'NONE',  ( 22.56230152254412147, 3.464101615137759271, -9.637499999999990408 ) ) ;
#21843 = ORIENTED_EDGE ( 'NONE', *, *, #2504, .F. ) ;
#21844 = DIRECTION ( 'NONE',  ( 0.000000000000000000, 0.000000000000000000, 1.000000000000000000 ) ) ;
#21845 = CARTESIAN_POINT ( 'NONE',  ( -9.465287035748065847, 86.59768628210143504, -2.064181346179273735 ) ) ;
#21846 = DIRECTION ( 'NONE',  ( 0.000000000000000000, 0.000000000000000000, 1.000000000000000000 ) ) ;
#21847 = CARTESIAN_POINT ( 'NONE',  ( -8.710071997420207879, 125.5148137178985763, 3.796722387233182339 ) ) ;
#21848 = CARTESIAN_POINT ( 'NONE',  ( 13.62178482187501416, 196.8031250006145285, 23.59362340125806767 ) ) ;
#21849 = CYLINDRICAL_SURFACE ( 'NONE', #25624, 5.999999999999994671 ) ;
#21850 = CARTESIAN_POINT ( 'NONE',  ( 27.24356964375000700, 198.6968750006145115, 15.72908226750537075 ) ) ;
#21851 = LINE ( 'NONE', #16534, #8943 ) ;
#21852 = CARTESIAN_POINT ( 'NONE',  ( 26.99999999999999645, 243.9625000000000057, -3.464101615137755275 ) ) ;
#21853 = CARTESIAN_POINT ( 'NONE',  ( 0.1745138560723095977, 59.38981371789856212, 9.500000000000005329 ) ) ;
#21854 = ORIENTED_EDGE ( 'NONE', *, *, #20078, .T. ) ;
#21855 = CARTESIAN_POINT ( 'NONE',  ( 15.00000000000000178, 244.6937500012290627, 3.464101615137757051 ) ) ;
#21856 = CARTESIAN_POINT ( 'NONE',  ( -11.61527771782809282, 80.66481371789856780, -4.622313124798832717 ) ) ;
#21857 = CARTESIAN_POINT ( 'NONE',  ( 10.31873187879411091, 3.604726614523240613, -5.184374999385507721 ) ) ;
#21858 = CARTESIAN_POINT ( 'NONE',  ( 25.44230085693126497, 0.000000000000000000, 169.6180106133541869 ) ) ;
#21859 = CARTESIAN_POINT ( 'NONE',  ( 26.75643035624999655, 7.049594010296217766E-16, -8.128124999385477167 ) ) ;
#21860 = CARTESIAN_POINT ( 'NONE',  ( -2.311890736173448424, 41.27731371789855075, 12.53471296425189330 ) ) ;
#21861 = VERTEX_POINT ( 'NONE', #32745 ) ;
#21862 = CARTESIAN_POINT ( 'NONE',  ( 26.75643035624999655, 7.049594010296217766E-16, -6.665624999385472371 ) ) ;
#21863 = CARTESIAN_POINT ( 'NONE',  ( 10.49813415415989581, 27.37268628210144783, 7.228626920339068285 ) ) ;
#21864 = EDGE_CURVE ( 'NONE', #25338, #21070, #33296, .T. ) ;
#21865 = CARTESIAN_POINT ( 'NONE',  ( -30.60044563604516199, 205.1570982666397072, -4.673758765035155527 ) ) ;
#21866 = CARTESIAN_POINT ( 'NONE',  ( -54.35044563604515133, 205.1570982666397072, -4.673758765035155527 ) ) ;
#21867 = CARTESIAN_POINT ( 'NONE',  ( 27.57131143846490673, 5.196152422706630247, 159.5315731764057716 ) ) ;
#21868 = CARTESIAN_POINT ( 'NONE',  ( -12.46528703574811558, 70.60231371789856780, 2.660918448318003726 ) ) ;
#21869 = CARTESIAN_POINT ( 'NONE',  ( -45.25372103062157692, 214.5309553116392749, -1.090244570138262148 ) ) ;
#21870 = CARTESIAN_POINT ( 'NONE',  ( -56.33705436395489841, 205.3262412349647263, -4.842901733360204020 ) ) ;
#21871 = CARTESIAN_POINT ( 'NONE',  ( -13.49999999999998401, 196.9250000000000114, 23.38268590217985476 ) ) ;
#21872 = CARTESIAN_POINT ( 'NONE',  ( -13.45723662585736591, 216.2569280196711645, -5.070466603772765701 ) ) ;
#21873 = CARTESIAN_POINT ( 'NONE',  ( 15.46528703574811736, 38.40231371789853654, -3.257655550456947768 ) ) ;
#21874 = CARTESIAN_POINT ( 'NONE',  ( -47.22544563604517265, 216.3070033484980854, 6.137860380172893926 ) ) ;
#21875 = DIRECTION ( 'NONE',  ( 0.08715574274765150453, 0.000000000000000000, 0.9961946980917461003 ) ) ;
#21876 = CARTESIAN_POINT ( 'NONE',  ( 0.1745138560725515708, 70.21018628210144641, -12.50000000000000355 ) ) ;
#21877 = CARTESIAN_POINT ( 'NONE',  ( -14.38691631536207183, 30.53518628210144570, 5.770363421893814682 ) ) ;
#21878 = EDGE_CURVE ( 'NONE', #25851, #1984, #29905, .T. ) ;
#21879 = CARTESIAN_POINT ( 'NONE',  ( 10.56230152254410903, 0.000000000000000000, -2.700000000000063238 ) ) ;
#21880 = CARTESIAN_POINT ( 'NONE',  ( -28.88589706552147263, 202.4236885276250746, -2.582340647126037059 ) ) ;
#21881 = CIRCLE ( 'NONE', #23690, 2.649999999999985700 ) ;
#21882 = VERTEX_POINT ( 'NONE', #9814 ) ;
#21883 = CARTESIAN_POINT ( 'NONE',  ( 0.1745138560725837118, 24.21018628210144996, -15.50000000000000533 ) ) ;
#21884 = CARTESIAN_POINT ( 'NONE',  ( 5.778771075727756162E-15, 197.2156250006145513, 31.45816453501076637 ) ) ;
#21885 = CARTESIAN_POINT ( 'NONE',  ( 10.56230152254383903, -3.464101615137598067, -0.7499999987710416205 ) ) ;
#21886 = CARTESIAN_POINT ( 'NONE',  ( 24.85726793373807908, -3.464101615138005741, 162.9310537024133225 ) ) ;
#21887 = DIRECTION ( 'NONE',  ( -0.000000000000000000, 1.000000000000000000, -0.000000000000000000 ) ) ;
#21888 = CARTESIAN_POINT ( 'NONE',  ( 26.99999999999999645, 7.347880794884117764E-16, -7.818749998770941012 ) ) ;
#21889 = ADVANCED_FACE ( 'NONE', ( #21391 ), #32933, .T. ) ;
#21890 = CARTESIAN_POINT ( 'NONE',  ( 11.61527771782819940, 7.535186282101452804, -4.622313124798573369 ) ) ;
#21891 = CARTESIAN_POINT ( 'NONE',  ( 26.75643035624999655, 247.7968750006145342, 3.323476615752267715 ) ) ;
#21892 = CARTESIAN_POINT ( 'NONE',  ( 1.715153634034445762, 128.6773137178985280, -9.534712964251895073 ) ) ;
#21893 = CARTESIAN_POINT ( 'NONE',  ( 15.24356964374999990, 243.5218750006145569, -3.323476615752268604 ) ) ;
#21894 = EDGE_LOOP ( 'NONE', ( #33366, #34936, #667, #1971 ) ) ;
#21895 = LINE ( 'NONE', #5002, #11145 ) ;
#21896 = LINE ( 'NONE', #33444, #36209 ) ;
#21897 = CARTESIAN_POINT ( 'NONE',  ( -12.50000000000000355, 135.2898137178985678, 0.1745138560722786503 ) ) ;
#21898 = CARTESIAN_POINT ( 'NONE',  ( 22.80587116629411071, 3.604726614523238837, -5.728124999385511451 ) ) ;
#21899 = CARTESIAN_POINT ( 'NONE',  ( 34.17721086063072988, -5.407089921784855591, 164.7977454806546120 ) ) ;
#21900 =( BOUNDED_CURVE ( )  B_SPLINE_CURVE ( 2, ( #15089, #23434, #6370, #2776, #37450, #31589, #17941 ),
 .UNSPECIFIED., .F., .F. ) 
 B_SPLINE_CURVE_WITH_KNOTS ( ( 3, 2, 2, 3 ),
 ( 0.5434782608695640782, 0.5507246376811584243, 0.5579710144927527704, 0.5652173913043470055 ),
 .UNSPECIFIED. ) 
 CURVE ( )  GEOMETRIC_REPRESENTATION_ITEM ( )  RATIONAL_B_SPLINE_CURVE ( ( 1.000000000000020428, 0.8660254037844181685, 1.000000000000000000, 0.8660254037844387076, 1.000000000000000000, 0.8660254037844530295, 0.9999999999999856781 ) ) 
 REPRESENTATION_ITEM ( '' )  );
#21901 = CARTESIAN_POINT ( 'NONE',  ( 15.00000000000000000, 0.000000000000000000, -5.399999999999987921 ) ) ;
#21902 = CARTESIAN_POINT ( 'NONE',  ( 13.49999999999999645, 198.5000000000000000, -23.38268590217984766 ) ) ;
#21903 = ORIENTED_EDGE ( 'NONE', *, *, #26608, .F. ) ;
#21904 = CARTESIAN_POINT ( 'NONE',  ( -11.61527771782819940, 39.73518628210144499, 4.622313124798574258 ) ) ;
#21905 = ORIENTED_EDGE ( 'NONE', *, *, #18128, .F. ) ;
#21906 = ORIENTED_EDGE ( 'NONE', *, *, #195, .F. ) ;
#21907 = CARTESIAN_POINT ( 'NONE',  ( 15.00000000000000178, -3.464101615137757051, -4.856249998770946874 ) ) ;
#21908 = LINE ( 'NONE', #18887, #6829 ) ;
#21909 = CARTESIAN_POINT ( 'NONE',  ( 20.99999999999997868, 245.1625000000000227, 5.999999999999999112 ) ) ;
#21910 = CARTESIAN_POINT ( 'NONE',  ( 21.00000000000000000, -6.646953231504538984, -9.028124999385470417 ) ) ;
#21911 = CIRCLE ( 'NONE', #32171, 28.99999999999999645 ) ;
#21912 = CARTESIAN_POINT ( 'NONE',  ( 11.61527771782819940, 71.93518628210145494, -4.622313124798573369 ) ) ;
#21913 = CARTESIAN_POINT ( 'NONE',  ( 2.908627838312458636, 9.077313717898549683, -15.53471296425188442 ) ) ;
#21914 = CARTESIAN_POINT ( 'NONE',  ( 16.56230152254411436, -6.928203230275514990, -5.737500000000049560 ) ) ;
#21915 = CARTESIAN_POINT ( 'NONE',  ( 19.06670604969872329, 215.1554505341390211, 5.693556627485715893 ) ) ;
#21916 = CARTESIAN_POINT ( 'NONE',  ( -60.68377896937850835, 208.9097554298617183, 4.530955311639234040 ) ) ;
#21917 = AXIS2_PLACEMENT_3D ( 'NONE', #21198, #21571, #892 ) ;
#21918 = CARTESIAN_POINT ( 'NONE',  ( 37.19073179189800271, 7.347880794884117764E-16, 166.2186317273649934 ) ) ;
#21919 = CARTESIAN_POINT ( 'NONE',  ( -6.932735513424201912, 124.6523137178985650, 10.69584247140429412 ) ) ;
#21920 = EDGE_CURVE ( 'NONE', #3698, #22652, #22789, .T. ) ;
#21921 = CARTESIAN_POINT ( 'NONE',  ( -43.86830436395490551, 209.8844732041982581, 6.500000000000000888 ) ) ;
#21922 = CARTESIAN_POINT ( 'NONE',  ( -56.53497103062156270, 202.6965474657331185, -4.350049139982091084 ) ) ;
#21923 =( BOUNDED_SURFACE ( )  B_SPLINE_SURFACE ( 1, 2, ( 
 ( #16781, #25486, #28326, #2364, #33649, #36480, #25301, #16965, #10522, #25672, #8250, #4831, #36853, #22100, #13937, #22660, #7688, #19269, #37226, #30809, #11272, #16411, #13755, #22285, #1989, #36672, #22843, #31361, #8062, #13561, #34205, #25114, #19824, #33839, #19450, #7876, #31544, #5385, #28508, #31000, #5019, #28143, #34389, #2551, #10897, #22469, #2173, #34017, #14118, #19638, #5569, #26042, #11822, #31731, #2915, #443, #11635, #23392, #23580, #20742, #6131, #5759, #32284, #34572, #5945, #20937, #23767, #26596, #17708, #14671, #3102, #8612, #26221, #35124, #34939, #6328, #69, #8984, #17337, #14486, #12008, #23209, #20556, #9173, #17899, #29249, #28881, #29443, #20182, #17524, #32471, #35308, #34758, #29631, #3290, #6516, #257, #3667, #627, #8801, #18091, #25856, #37405, #20371, #29059, #11455, #3479, #15048, #12195, #31915, #23024, #9362, #32099, #14862, #26409, #3852, #15237, #18845, #35501, #26787, #21677, #12765, #26977, #33231, #1383, #9549, #7269, #12955, #33043, #18469, #27167, #4040, #21123, #30390, #30010, #18275, #4412, #15995, #24333, #35874, #4226, #35687, #24145, #9917, #1003, #9740, #21311, #15612, #32847, #818, #1190, #23958, #24515, #21500, #7090, #18660, #30199, #32662, #27542, #15803, #36064, #12389, #6703, #29817, #6894, #27353, #15428, #10107, #12578, #15358, #34684, #749, #26912, #12320, #11569, #26340, #34874, #23142, #11755, #23893, #6448, #20673, #8729, #560, #20302, #23701, #17455, #32029, #3033, #21058, #12126, #35244, #31843, #29752, #6059, #14605, #32408, #9106, #5876, #3783, #23512, #35058, #28992, #29373, #9482, #26156, #17646, #189, #23323, #6636, #18021, #3222, #26717, #32596, #32221, #6260, #8915, #20490, #29180, #14794, #376, #11943, #18210, #29566, #17837, #3411, #14980, #26529, #9297, #20869, #3603, #35434, #15169, #10227, #1689, #18783, #35623, #30701, #13078, #21246, #21802, #1502, #24267, #4166, #24450, #21990, #18397, #940, #33165, #36000, #27476, #7390, #19153, #24632, #9669, #29946, #32786, #36182, #18592, #3974, #10037, #36368, #13264, #21614, #10415, #6821, #32972, #1129, #18963 ),
 ( #4348, #1317, #12885, #33354, #27665, #21432, #27286, #33537, #16113, #30517, #15927, #7577, #7211, #30323, #12695, #4537, #24816, #7025, #12514, #4721, #15547, #27105, #16298, #24078, #30135, #35811, #9853, #15736, #722, #6424, #17808, #9083, #29350, #32199, #28973, #29727, #20653, #11734, #15334, #26886, #26505, #12102, #29541, #14773, #3197, #919, #3013, #355, #12487, #26693, #3580, #9456, #26318, #35600, #17998, #8892, #35038, #21033, #32009, #20282, #3760, #14583, #31822, #32570, #14959, #6039, #6611, #12295, #23867, #35407, #15142, #3389, #6234, #536, #23676, #26135, #24054, #35221, #23306, #5857, #17434, #9271, #20842, #18185, #11920, #23487, #32384, #17626, #169, #34852, #20470, #29155, #24973, #18758, #21222, #16091, #15905, #36160, #27452, #13056, #6798, #27826, #35978, #27642, #13425, #36345, #18942, #15526, #10015, #9645, #4326, #24611, #32761, #18372, #10390, #29919, #21966, #3951, #24429, #32947, #27081, #9830, #33512, #4517, #30300, #1106, #10206, #12674, #21780, #24242, #30113, #35788, #19132, #33330, #7370, #21408, #1856, #4143, #7556, #1481, #21595, #33145, #7002, #7189, #30494, #1671, #13245, #18571, #24794, #15715, #27266, #30679, #1291, #4698, #16279, #12863, #16835, #4885, #5434, #7739, #16652, #31596, #34440, #13620, #2782, #13985, #5619, #25355, #14355, #11322, #19503, #17203, #36532, #28742, #25723, #8480, #2597, #22892, #36723, #37089, #2041, #19871, #34069, #10576, #22154, #10949, #22523, #33701, #28376, #20049, #30860, #5071, #19323, #28009, #16465, #31415, #28196, #14168, #25171, #8118, #19690, #10764, #22335, #7929, #33887, #36901, #31050, #2226, #17016, #13806, #31230, #5258, #2413, #25537, #11137, #22714, #37276, #34257, #8300, #28556, #6188, #23073, #18140, #493, #8664, #35175, #26459, #11688, #29110, #11871, #9412, #5811, #25909, #20609, #23440, #14910, #32338, #6565, #12059, #34619, #17392, #20233, #23633, #5998, #28933, #34993, #23819, #26648, #9037, #35361, #31776, #20423, #26092, #6376, #8849, #9222, #20795, #23261, #17761, #17578, #34805, #17951, #29302, #26273, #306, #29494, #15098, #31967, #14725 ) ),
 .UNSPECIFIED., .F., .F., .F. ) 
 B_SPLINE_SURFACE_WITH_KNOTS ( ( 2, 2 ),
 ( 3, 2, 2, 2, 2, 2, 2, 2, 2, 2, 2, 2, 2, 2, 2, 2, 2, 2, 2, 2, 2, 2, 2, 2, 2, 2, 2, 2, 2, 2, 2, 2, 2, 2, 2, 2, 2, 2, 2, 2, 2, 2, 2, 2, 2, 2, 2, 2, 2, 2, 2, 2, 2, 2, 2, 2, 2, 2, 2, 2, 2, 2, 2, 2, 2, 2, 2, 2, 2, 2, 2, 2, 2, 2, 2, 2, 2, 2, 2, 2, 2, 2, 2, 2, 2, 2, 2, 2, 2, 2, 2, 2, 2, 2, 2, 2, 2, 2, 2, 2, 2, 2, 2, 2, 2, 2, 2, 2, 2, 2, 2, 2, 2, 2, 2, 2, 2, 2, 2, 2, 2, 2, 2, 2, 2, 2, 2, 2, 2, 2, 2, 2, 2, 2, 3 ),
 ( 0.000000000000000000, 1.000000000000000000 ),
 ( 0.000000000000000000, 0.007246376811594202987, 0.01449275362318840597, 0.02173913043478260809, 0.02898550724637681195, 0.03623188405797101580, 0.04347826086956521618, 0.05072463768115942351, 0.05797101449275362389, 0.06521739130434782428, 0.07246376811594203160, 0.07971014492753622505, 0.08695652173913043237, 0.09420289855072463969, 0.1014492753623188470, 0.1086956521739130405, 0.1159420289855072478, 0.1231884057971014551, 0.1304347826086956486, 0.1376811594202898559, 0.1449275362318840632, 0.1521739130434782705, 0.1594202898550724501, 0.1666666666666666574, 0.1739130434782608647, 0.1811594202898550721, 0.1884057971014492794, 0.1956521739130434867, 0.2028985507246376940, 0.2101449275362318736, 0.2173913043478260809, 0.2246376811594202882, 0.2318840579710144956, 0.2391304347826087029, 0.2463768115942029102, 0.2536231884057971175, 0.2608695652173912971, 0.2681159420289855322, 0.2753623188405797118, 0.2826086956521738913, 0.2898550724637681264, 0.2971014492753623060, 0.3043478260869565410, 0.3115942028985507206, 0.3188405797101449002, 0.3260869565217391353, 0.3333333333333333148, 0.3405797101449275499, 0.3478260869565217295, 0.3550724637681159646, 0.3623188405797101441, 0.3695652173913043237, 0.3768115942028985588, 0.3840579710144927383, 0.3913043478260869734, 0.3985507246376811530, 0.4057971014492753881, 0.4130434782608695676, 0.4202898550724637472, 0.4275362318840579823, 0.4347826086956521618, 0.4420289855072463969, 0.4492753623188405765, 0.4565217391304347561, 0.4637681159420289911, 0.4710144927536231707, 0.4782608695652174058, 0.4855072463768115854, 0.4927536231884058204, 0.5000000000000000000, 0.5072463768115942351, 0.5144927536231883591, 0.5217391304347825942, 0.5289855072463768293, 0.5362318840579710644, 0.5434782608695651884, 0.5507246376811594235, 0.5579710144927536586, 0.5652173913043477826, 0.5724637681159420177, 0.5797101449275362528, 0.5869565217391304879, 0.5942028985507246119, 0.6014492753623188470, 0.6086956521739130821, 0.6159420289855072062, 0.6231884057971014412, 0.6304347826086956763, 0.6376811594202898004, 0.6449275362318840354, 0.6521739130434782705, 0.6594202898550725056, 0.6666666666666666297, 0.6739130434782608647, 0.6811594202898550998, 0.6884057971014492239, 0.6956521739130434590, 0.7028985507246376940, 0.7101449275362319291, 0.7173913043478260532, 0.7246376811594202882, 0.7318840579710145233, 0.7391304347826086474, 0.7463768115942028825, 0.7536231884057971175, 0.7608695652173913526, 0.7681159420289854767, 0.7753623188405797118, 0.7826086956521739468, 0.7898550724637680709, 0.7971014492753623060, 0.8043478260869565410, 0.8115942028985507761, 0.8188405797101449002, 0.8260869565217391353, 0.8333333333333333703, 0.8405797101449274944, 0.8478260869565217295, 0.8550724637681159646, 0.8623188405797101996, 0.8695652173913043237, 0.8768115942028985588, 0.8840579710144927938, 0.8913043478260869179, 0.8985507246376811530, 0.9057971014492753881, 0.9130434782608695121, 0.9202898550724637472, 0.9275362318840579823, 0.9347826086956522174, 0.9420289855072463414, 0.9492753623188405765, 0.9565217391304348116, 0.9637681159420289356, 0.9662082973083875315 ),
 .UNSPECIFIED. ) 
 GEOMETRIC_REPRESENTATION_ITEM ( )  RATIONAL_B_SPLINE_SURFACE ( (
 ( 1.000000000000000000, 0.8660254037844387076, 1.000000000000000000, 0.8660254037844387076, 1.000000000000000000, 0.8660254037844387076, 1.000000000000000000, 0.8660254037844387076, 1.000000000000000000, 0.8660254037844387076, 1.000000000000000000, 0.8660254037844387076, 1.000000000000000000, 0.8660254037844387076, 1.000000000000000000, 0.8660254037844387076, 1.000000000000000000, 0.8660254037844387076, 1.000000000000000000, 0.8660254037844387076, 1.000000000000000000, 0.8660254037844387076, 1.000000000000000000, 0.8660254037844387076, 1.000000000000000000, 0.8660254037844387076, 1.000000000000000000, 0.8660254037844387076, 1.000000000000000000, 0.8660254037844387076, 1.000000000000000000, 0.8660254037844387076, 1.000000000000000000, 0.8660254037844387076, 1.000000000000000000, 0.8660254037844387076, 1.000000000000000000, 0.8660254037844387076, 1.000000000000000000, 0.8660254037844387076, 1.000000000000000000, 0.8660254037844387076, 1.000000000000000000, 0.8660254037844387076, 1.000000000000000000, 0.8660254037844387076, 1.000000000000000000, 0.8660254037844387076, 1.000000000000000000, 0.8660254037844387076, 1.000000000000000000, 0.8660254037844387076, 1.000000000000000000, 0.8660254037844387076, 1.000000000000000000, 0.8660254037844387076, 1.000000000000000000, 0.8660254037844387076, 1.000000000000000000, 0.8660254037844387076, 1.000000000000000000, 0.8660254037844387076, 1.000000000000000000, 0.8660254037844387076, 1.000000000000000000, 0.8660254037844387076, 1.000000000000000000, 0.8660254037844387076, 1.000000000000000000, 0.8660254037844387076, 1.000000000000000000, 0.8660254037844387076, 1.000000000000000000, 0.8660254037844387076, 1.000000000000000000, 0.8660254037844387076, 1.000000000000000000, 0.8660254037844387076, 1.000000000000000000, 0.8660254037844387076, 1.000000000000000000, 0.8660254037844387076, 1.000000000000000000, 0.8660254037844387076, 1.000000000000000000, 0.8660254037844387076, 1.000000000000000000, 0.8660254037844387076, 1.000000000000000000, 0.8660254037844387076, 1.000000000000000000, 0.8660254037844387076, 1.000000000000000000, 0.8660254037844387076, 1.000000000000000000, 0.8660254037844387076, 1.000000000000000000, 0.8660254037844387076, 1.000000000000000000, 0.8660254037844387076, 1.000000000000000000, 0.8660254037844387076, 1.000000000000000000, 0.8660254037844387076, 1.000000000000000000, 0.8660254037844387076, 1.000000000000000000, 0.8660254037844387076, 1.000000000000000000, 0.8660254037844387076, 1.000000000000000000, 0.8660254037844387076, 1.000000000000000000, 0.8660254037844387076, 1.000000000000000000, 0.8660254037844387076, 1.000000000000000000, 0.8660254037844387076, 1.000000000000000000, 0.8660254037844387076, 1.000000000000000000, 0.8660254037844387076, 1.000000000000000000, 0.8660254037844387076, 1.000000000000000000, 0.8660254037844387076, 1.000000000000000000, 0.8660254037844387076, 1.000000000000000000, 0.8660254037844387076, 1.000000000000000000, 0.8660254037844387076, 1.000000000000000000, 0.8660254037844387076, 1.000000000000000000, 0.8660254037844387076, 1.000000000000000000, 0.8660254037844387076, 1.000000000000000000, 0.8660254037844387076, 1.000000000000000000, 0.8660254037844387076, 1.000000000000000000, 0.8660254037844387076, 1.000000000000000000, 0.8660254037844387076, 1.000000000000000000, 0.8660254037844387076, 1.000000000000000000, 0.8660254037844387076, 1.000000000000000000, 0.8660254037844387076, 1.000000000000000000, 0.8660254037844387076, 1.000000000000000000, 0.8660254037844387076, 1.000000000000000000, 0.8660254037844387076, 1.000000000000000000, 0.8660254037844387076, 1.000000000000000000, 0.8660254037844387076, 1.000000000000000000, 0.8660254037844387076, 1.000000000000000000, 0.8660254037844387076, 1.000000000000000000, 0.8660254037844387076, 1.000000000000000000, 0.8660254037844387076, 1.000000000000000000, 0.8660254037844387076, 1.000000000000000000, 0.8660254037844387076, 1.000000000000000000, 0.8660254037844387076, 1.000000000000000000, 0.8660254037844387076, 1.000000000000000000, 0.8660254037844387076, 1.000000000000000000, 0.8660254037844387076, 1.000000000000000000, 0.8660254037844387076, 1.000000000000000000, 0.8660254037844387076, 1.000000000000000000, 0.8660254037844387076, 1.000000000000000000, 0.8660254037844387076, 1.000000000000000000, 0.8660254037844387076, 1.000000000000000000, 0.8660254037844387076, 1.000000000000000000, 0.8660254037844387076, 1.000000000000000000, 0.8660254037844387076, 1.000000000000000000, 0.8660254037844387076, 1.000000000000000000, 0.8660254037844387076, 1.000000000000000000, 0.8660254037844387076, 1.000000000000000000, 0.8660254037844387076, 1.000000000000000000, 0.8660254037844387076, 1.000000000000000000, 0.8660254037844387076, 1.000000000000000000, 0.8660254037844387076, 1.000000000000000000, 0.8660254037844387076, 1.000000000000000000, 0.8660254037844387076, 1.000000000000000000, 0.8660254037844387076, 1.000000000000000000, 0.8660254037844387076, 1.000000000000000000, 0.8660254037844387076, 1.000000000000000000, 0.8660254037844387076, 1.000000000000000000, 0.8660254037844387076, 1.000000000000000000, 0.8660254037844387076, 1.000000000000000000, 0.8660254037844387076, 1.000000000000000000, 0.8660254037844387076, 1.000000000000000000, 0.8660254037844387076, 1.000000000000000000, 0.8660254037844387076, 1.000000000000000000, 0.8660254037844387076, 1.000000000000000000, 0.8660254037844387076, 1.000000000000000000, 0.8660254037844387076, 1.000000000000000000, 0.8660254037844387076, 1.000000000000000000, 0.8660254037844387076, 1.000000000000000000, 0.8660254037844387076, 1.000000000000000000, 0.8660254037844387076, 1.000000000000000000, 0.8660254037844387076, 1.000000000000000000, 0.8660254037844387076, 1.000000000000000000, 0.8660254037844387076, 1.000000000000000000, 0.8660254037844387076, 1.000000000000000000, 0.8660254037844387076, 1.000000000000000000, 0.8660254037844387076, 1.000000000000000000, 0.8660254037844387076, 1.000000000000000000, 0.8660254037844387076, 1.000000000000000000, 0.9548847207714133978, 0.9401541335272454170),
 ( 1.000000000000000000, 0.8660254037844387076, 1.000000000000000000, 0.8660254037844387076, 1.000000000000000000, 0.8660254037844387076, 1.000000000000000000, 0.8660254037844387076, 1.000000000000000000, 0.8660254037844387076, 1.000000000000000000, 0.8660254037844387076, 1.000000000000000000, 0.8660254037844387076, 1.000000000000000000, 0.8660254037844387076, 1.000000000000000000, 0.8660254037844387076, 1.000000000000000000, 0.8660254037844387076, 1.000000000000000000, 0.8660254037844387076, 1.000000000000000000, 0.8660254037844387076, 1.000000000000000000, 0.8660254037844387076, 1.000000000000000000, 0.8660254037844387076, 1.000000000000000000, 0.8660254037844387076, 1.000000000000000000, 0.8660254037844387076, 1.000000000000000000, 0.8660254037844387076, 1.000000000000000000, 0.8660254037844387076, 1.000000000000000000, 0.8660254037844387076, 1.000000000000000000, 0.8660254037844387076, 1.000000000000000000, 0.8660254037844387076, 1.000000000000000000, 0.8660254037844387076, 1.000000000000000000, 0.8660254037844387076, 1.000000000000000000, 0.8660254037844387076, 1.000000000000000000, 0.8660254037844387076, 1.000000000000000000, 0.8660254037844387076, 1.000000000000000000, 0.8660254037844387076, 1.000000000000000000, 0.8660254037844387076, 1.000000000000000000, 0.8660254037844387076, 1.000000000000000000, 0.8660254037844387076, 1.000000000000000000, 0.8660254037844387076, 1.000000000000000000, 0.8660254037844387076, 1.000000000000000000, 0.8660254037844387076, 1.000000000000000000, 0.8660254037844387076, 1.000000000000000000, 0.8660254037844387076, 1.000000000000000000, 0.8660254037844387076, 1.000000000000000000, 0.8660254037844387076, 1.000000000000000000, 0.8660254037844387076, 1.000000000000000000, 0.8660254037844387076, 1.000000000000000000, 0.8660254037844387076, 1.000000000000000000, 0.8660254037844387076, 1.000000000000000000, 0.8660254037844387076, 1.000000000000000000, 0.8660254037844387076, 1.000000000000000000, 0.8660254037844387076, 1.000000000000000000, 0.8660254037844387076, 1.000000000000000000, 0.8660254037844387076, 1.000000000000000000, 0.8660254037844387076, 1.000000000000000000, 0.8660254037844387076, 1.000000000000000000, 0.8660254037844387076, 1.000000000000000000, 0.8660254037844387076, 1.000000000000000000, 0.8660254037844387076, 1.000000000000000000, 0.8660254037844387076, 1.000000000000000000, 0.8660254037844387076, 1.000000000000000000, 0.8660254037844387076, 1.000000000000000000, 0.8660254037844387076, 1.000000000000000000, 0.8660254037844387076, 1.000000000000000000, 0.8660254037844387076, 1.000000000000000000, 0.8660254037844387076, 1.000000000000000000, 0.8660254037844387076, 1.000000000000000000, 0.8660254037844387076, 1.000000000000000000, 0.8660254037844387076, 1.000000000000000000, 0.8660254037844387076, 1.000000000000000000, 0.8660254037844387076, 1.000000000000000000, 0.8660254037844387076, 1.000000000000000000, 0.8660254037844387076, 1.000000000000000000, 0.8660254037844387076, 1.000000000000000000, 0.8660254037844387076, 1.000000000000000000, 0.8660254037844387076, 1.000000000000000000, 0.8660254037844387076, 1.000000000000000000, 0.8660254037844387076, 1.000000000000000000, 0.8660254037844387076, 1.000000000000000000, 0.8660254037844387076, 1.000000000000000000, 0.8660254037844387076, 1.000000000000000000, 0.8660254037844387076, 1.000000000000000000, 0.8660254037844387076, 1.000000000000000000, 0.8660254037844387076, 1.000000000000000000, 0.8660254037844387076, 1.000000000000000000, 0.8660254037844387076, 1.000000000000000000, 0.8660254037844387076, 1.000000000000000000, 0.8660254037844387076, 1.000000000000000000, 0.8660254037844387076, 1.000000000000000000, 0.8660254037844387076, 1.000000000000000000, 0.8660254037844387076, 1.000000000000000000, 0.8660254037844387076, 1.000000000000000000, 0.8660254037844387076, 1.000000000000000000, 0.8660254037844387076, 1.000000000000000000, 0.8660254037844387076, 1.000000000000000000, 0.8660254037844387076, 1.000000000000000000, 0.8660254037844387076, 1.000000000000000000, 0.8660254037844387076, 1.000000000000000000, 0.8660254037844387076, 1.000000000000000000, 0.8660254037844387076, 1.000000000000000000, 0.8660254037844387076, 1.000000000000000000, 0.8660254037844387076, 1.000000000000000000, 0.8660254037844387076, 1.000000000000000000, 0.8660254037844387076, 1.000000000000000000, 0.8660254037844387076, 1.000000000000000000, 0.8660254037844387076, 1.000000000000000000, 0.8660254037844387076, 1.000000000000000000, 0.8660254037844387076, 1.000000000000000000, 0.8660254037844387076, 1.000000000000000000, 0.8660254037844387076, 1.000000000000000000, 0.8660254037844387076, 1.000000000000000000, 0.8660254037844387076, 1.000000000000000000, 0.8660254037844387076, 1.000000000000000000, 0.8660254037844387076, 1.000000000000000000, 0.8660254037844387076, 1.000000000000000000, 0.8660254037844387076, 1.000000000000000000, 0.8660254037844387076, 1.000000000000000000, 0.8660254037844387076, 1.000000000000000000, 0.8660254037844387076, 1.000000000000000000, 0.8660254037844387076, 1.000000000000000000, 0.8660254037844387076, 1.000000000000000000, 0.8660254037844387076, 1.000000000000000000, 0.8660254037844387076, 1.000000000000000000, 0.8660254037844387076, 1.000000000000000000, 0.8660254037844387076, 1.000000000000000000, 0.8660254037844387076, 1.000000000000000000, 0.8660254037844387076, 1.000000000000000000, 0.8660254037844387076, 1.000000000000000000, 0.8660254037844387076, 1.000000000000000000, 0.8660254037844387076, 1.000000000000000000, 0.8660254037844387076, 1.000000000000000000, 0.8660254037844387076, 1.000000000000000000, 0.8660254037844387076, 1.000000000000000000, 0.8660254037844387076, 1.000000000000000000, 0.8660254037844387076, 1.000000000000000000, 0.8660254037844387076, 1.000000000000000000, 0.8660254037844387076, 1.000000000000000000, 0.8660254037844387076, 1.000000000000000000, 0.8660254037844387076, 1.000000000000000000, 0.8660254037844387076, 1.000000000000000000, 0.8660254037844387076, 1.000000000000000000, 0.9548847207714133978, 0.9401541335272454170) ) ) 
 REPRESENTATION_ITEM ( '' )  SURFACE ( )  );
#21924 = CONTEXT_DEPENDENT_SHAPE_REPRESENTATION ( #13917, #475 ) ;
#21925 = CARTESIAN_POINT ( 'NONE',  ( 15.24356964374999990, 0.000000000000000000, -1.603124999385474592 ) ) ;
#21926 = CARTESIAN_POINT ( 'NONE',  ( -13.62178482187498396, 195.8281250006145342, 23.59362340125808188 ) ) ;
#21927 = CARTESIAN_POINT ( 'NONE',  ( 15.50000000000000533, 93.88981371789856212, -0.1745138560722452326 ) ) ;
#21928 = CARTESIAN_POINT ( 'NONE',  ( -42.27752896937850124, 213.3500491399821613, 5.571401726697954970 ) ) ;
#21929 = ADVANCED_FACE ( 'NONE', ( #1273 ), #7354, .F. ) ;
#21930 = ORIENTED_EDGE ( 'NONE', *, *, #15239, .T. ) ;
#21931 = CARTESIAN_POINT ( 'NONE',  ( 25.40308077269482112, 0.000000000000000000, 169.1697229992128939 ) ) ;
#21932 = CARTESIAN_POINT ( 'NONE',  ( 7.228626920339068285, 126.2726862821014606, -10.49813415415989581 ) ) ;
#21933 = CARTESIAN_POINT ( 'NONE',  ( -14.38691631536207183, 76.53518628210146346, 5.770363421893814682 ) ) ;
#21934 = CARTESIAN_POINT ( 'NONE',  ( 0.000000000000000000, 0.000000000000000000, 3.000000000000000000 ) ) ;
#21935 = CARTESIAN_POINT ( 'NONE',  ( 30.98069435314010178, -7.209453229046482114, 164.0798584742748574 ) ) ;
#21936 = CARTESIAN_POINT ( 'NONE',  ( -13.04141134922759804, 77.97268628210142083, -8.927990412390657937 ) ) ;
#21937 = AXIS2_PLACEMENT_3D ( 'NONE', #25556, #10782, #24813 ) ;
#21938 = CARTESIAN_POINT ( 'NONE',  ( -58.11830436395490551, 209.8844732041982581, 6.500000000000000888 ) ) ;
#21939 = ADVANCED_FACE ( 'NONE', ( #27993 ), #4309, .F. ) ;
#21940 = CARTESIAN_POINT ( 'NONE',  ( 19.68408634441910721, -5.407089921784855591, -3.590624999385533478 ) ) ;
#21941 = CARTESIAN_POINT ( 'NONE',  ( -5.233372021372430183, 41.74768628210143362, -8.152565276336710909 ) ) ;
#21942 = CYLINDRICAL_SURFACE ( 'NONE', #23724, 27.00000000000000000 ) ;
#21943 = CARTESIAN_POINT ( 'NONE',  ( -37.53497103062155560, 202.6965474657331185, -4.350049139982091084 ) ) ;
#21944 = DIRECTION ( 'NONE',  ( 0.000000000000000000, 0.000000000000000000, -1.000000000000000000 ) ) ;
#21945 = CARTESIAN_POINT ( 'NONE',  ( 10.49813415415989581, 54.97268628210144925, 7.228626920339068285 ) ) ;
#21946 = CARTESIAN_POINT ( 'NONE',  ( 21.00000000000000355, 0.000000000000000000, 50.00000000000001421 ) ) ;
#21947 = CARTESIAN_POINT ( 'NONE',  ( 22.56230152254410015, 7.347880794884117764E-16, -7.762499998770988618 ) ) ;
#21949 = CARTESIAN_POINT ( 'NONE',  ( 13.44051670066911086, 5.407089921784862696, -0.7218749993855300140 ) ) ;
#21948 = CARTESIAN_POINT ( 'NONE',  ( 7.954856959092191815, 36.57268628210144357, 5.529263428287477744 ) ) ;
#21950 = CARTESIAN_POINT ( 'NONE',  ( 3.306546357697853733E-15, 210.0000000000000284, 27.00000000000000000 ) ) ;
#21951 = EDGE_LOOP ( 'NONE', ( #10630, #29764, #35685, #21518 ) ) ;
#21952 = CARTESIAN_POINT ( 'NONE',  ( 24.00000000000000000, -5.196152422706629359, -1.200000000000006617 ) ) ;
#21953 = CARTESIAN_POINT ( 'NONE',  ( 37.09265009776020605, 7.646167579472024665E-16, 162.3029045856885659 ) ) ;
#21954 = CARTESIAN_POINT ( 'NONE',  ( 24.70038759679188800, -3.464101615137761048, 161.1379032458482072 ) ) ;
#21955 = CARTESIAN_POINT ( 'NONE',  ( 18.00000000000000355, 246.9250000000000114, 5.196152422706632912 ) ) ;
#21956 = CARTESIAN_POINT ( 'NONE',  ( 16.56230152254411081, 6.928203230275506996, -4.049999998770996257 ) ) ;
#21957 = EDGE_CURVE ( 'NONE', #15760, #16220, #19031, .T. ) ;
#21958 = CARTESIAN_POINT ( 'NONE',  ( 12.50000000000000355, 84.68981371789854506, -0.1745138560722771515 ) ) ;
#21959 = CARTESIAN_POINT ( 'NONE',  ( -0.1745138560725500443, 93.21018628210146062, 12.50000000000000355 ) ) ;
#21960 = ORIENTED_EDGE ( 'NONE', *, *, #17958, .T. ) ;
#21961 = ORIENTED_EDGE ( 'NONE', *, *, #5707, .T. ) ;
#21962 = CARTESIAN_POINT ( 'NONE',  ( -13.49999999999998401, 197.4875000012290229, 23.38268590217985476 ) ) ;
#21963 = DIRECTION ( 'NONE',  ( 0.000000000000000000, 0.000000000000000000, 1.000000000000000000 ) ) ;
#21964 = CARTESIAN_POINT ( 'NONE',  ( 15.46528703574811736, 66.00231371789855928, -3.257655550456947768 ) ) ;
#21965 = CARTESIAN_POINT ( 'NONE',  ( 26.75643035624999655, 7.049594010296217766E-16, -5.878124999385475391 ) ) ;
#21966 = CARTESIAN_POINT ( 'NONE',  ( 23.87821517812500005, 245.5093750006145399, 4.985214923628404016 ) ) ;
#21967 = CARTESIAN_POINT ( 'NONE',  ( -57.92038769728823411, 208.6787018382581778, 4.469044688360752637 ) ) ;
#21968 =( BOUNDED_CURVE ( )  B_SPLINE_CURVE ( 2, ( #12414, #30035, #10316, #16020, #12789, #21148, #30608 ),
 .UNSPECIFIED., .F., .F. ) 
 B_SPLINE_CURVE_WITH_KNOTS ( ( 3, 2, 2, 3 ),
 ( 0.6956521739130446802, 0.7028985507246381381, 0.7101449275362314850, 0.7173913043478248319 ),
 .UNSPECIFIED. ) 
 CURVE ( )  GEOMETRIC_REPRESENTATION_ITEM ( )  RATIONAL_B_SPLINE_CURVE ( ( 0.9999999999999774625, 0.8660254037844612451, 1.000000000000000000, 0.8660254037844387076, 1.000000000000000000, 0.8660254037844612451, 0.9999999999999774625 ) ) 
 REPRESENTATION_ITEM ( '' )  );
#21969 = CARTESIAN_POINT ( 'NONE',  ( 0.000000000000000000, 148.0000000000000000, 0.000000000000000000 ) ) ;
#21970 = EDGE_CURVE ( 'NONE', #32379, #14644, #33495, .T. ) ;
#21971 = CARTESIAN_POINT ( 'NONE',  ( 9.465287035748106703, 47.60231371789853938, -2.064181346179063237 ) ) ;
#21972 = CARTESIAN_POINT ( 'NONE',  ( 22.80587116629410360, 7.646167579472015790E-16, -7.115624999385533833 ) ) ;
#21973 = CIRCLE ( 'NONE', #25599, 2.649999999999992806 ) ;
#21974 = CARTESIAN_POINT ( 'NONE',  ( -5.233372021372612259, 97.05231371789855643, 8.152565276336593669 ) ) ;
#21975 = CARTESIAN_POINT ( 'NONE',  ( -27.24356964375000345, 198.5093750006145399, 0.000000000000000000 ) ) ;
#21976 = CARTESIAN_POINT ( 'NONE',  ( -8.715434833792127023, 23.73981371789854578, 8.962234695871568846 ) ) ;
#21977 = CARTESIAN_POINT ( 'NONE',  ( -12.53471296425194836, 76.82268628210145778, 2.311890736173176641 ) ) ;
#21978 = CARTESIAN_POINT ( 'NONE',  ( 16.56230152254411081, -6.928203230275506996, -9.224999998771027165 ) ) ;
#21979 = DIRECTION ( 'NONE',  ( -0.000000000000000000, -1.000000000000000000, -0.000000000000000000 ) ) ;
#21980 = CARTESIAN_POINT ( 'NONE',  ( 27.62402916835064559, 5.407089921784856479, 161.5314637101514279 ) ) ;
#21981 = FACE_OUTER_BOUND ( 'NONE', #30461, .T. ) ;
#21982 = AXIS2_PLACEMENT_3D ( 'NONE', #21356, #32896, #35356 ) ;
#21983 = CARTESIAN_POINT ( 'NONE',  ( 13.44051670066911086, 5.407089921784862696, -6.121874999385518379 ) ) ;
#21984 = FILL_AREA_STYLE_COLOUR ( '', #9737 ) ;
#21985 = DIRECTION ( 'NONE',  ( 0.000000000000000000, 1.000000000000000000, 0.000000000000000000 ) ) ;
#21986 = CARTESIAN_POINT ( 'NONE',  ( 8.843639120294328748, 99.53518628210146346, -3.474262827703334722 ) ) ;
#21987 = CARTESIAN_POINT ( 'NONE',  ( 6.500000000000000000, 244.5000000000000000, 1.000000000000000000 ) ) ;
#21988 = CARTESIAN_POINT ( 'NONE',  ( -8.715434833791929847, 124.2601862821014578, -8.962234695871762469 ) ) ;
#21989 = CARTESIAN_POINT ( 'NONE',  ( 10.56230152254410903, 0.000000000000000000, -4.500000000000031974 ) ) ;
#21990 = CARTESIAN_POINT ( 'NONE',  ( 26.75643035624999655, 240.5593750006145513, -3.323476615752271712 ) ) ;
#21991 = ORIENTED_EDGE ( 'NONE', *, *, #8615, .T. ) ;
#21992 = CARTESIAN_POINT ( 'NONE',  ( 27.87242303518145548, -5.407089921784859143, 164.3706185997128841 ) ) ;
#21993 = CARTESIAN_POINT ( 'NONE',  ( 21.00000000000000000, 6.646953231504538984, -5.653124999385485516 ) ) ;
#21994 = CARTESIAN_POINT ( 'NONE',  ( 13.62178482187501416, 198.6593750006145456, 23.59362340125806767 ) ) ;
#21995 = CARTESIAN_POINT ( 'NONE',  ( 37.29858702344112231, 7.347880794884125653E-16, 167.4514226650291562 ) ) ;
#21996 = CARTESIAN_POINT ( 'NONE',  ( 36.67106567565804198, 7.347880794884125653E-16, 160.2788208387686097 ) ) ;
#21997 = CARTESIAN_POINT ( 'NONE',  ( 26.75643035624999655, 241.9468750006145683, 3.323476615752267715 ) ) ;
#21998 = CARTESIAN_POINT ( 'NONE',  ( 0.1745138560722779009, 132.9898137178985564, 12.50000000000000355 ) ) ;
#21999 = CARTESIAN_POINT ( 'NONE',  ( -27.24356964375000700, 194.8857344423842619, -9.915847606754345733 ) ) ;
#22001 = ORIENTED_EDGE ( 'NONE', *, *, #8440, .T. ) ;
#22000 = ORIENTED_EDGE ( 'NONE', *, *, #27303, .T. ) ;
#22002 = CARTESIAN_POINT ( 'NONE',  ( 26.75643035624999655, 244.1218750006145228, -7.049594010296217766E-16 ) ) ;
#22003 = LINE ( 'NONE', #37129, #15936 ) ;
#22004 = CARTESIAN_POINT ( 'NONE',  ( 26.75643035624999655, 7.049594010296217766E-16, -4.865624999385476102 ) ) ;
#22005 = CARTESIAN_POINT ( 'NONE',  ( -2.908627838312453306, 105.6773137178985706, 15.53471296425188797 ) ) ;
#22006 = CARTESIAN_POINT ( 'NONE',  ( 11.28998163430637725, -3.344369132205555317, -9.999999999999998224 ) ) ;
#22007 = CARTESIAN_POINT ( 'NONE',  ( 26.99999999999999645, 7.347880794884117764E-16, -9.618749998770963927 ) ) ;
#22008 = CARTESIAN_POINT ( 'NONE',  ( 13.44051670066910908, 5.407089921784862696, -9.271874999385531169 ) ) ;
#22009 = VERTEX_POINT ( 'NONE', #1655 ) ;
#22010 = CARTESIAN_POINT ( 'NONE',  ( 5.778771075727756162E-15, 194.9656250006145228, 31.45816453501075927 ) ) ;
#22011 = CARTESIAN_POINT ( 'NONE',  ( -12.46528703574805697, 123.3976862821014606, -2.660918448318280838 ) ) ;
#22012 = CARTESIAN_POINT ( 'NONE',  ( 19.68408634441910721, 5.407089921784857367, -0.2906249993855358760 ) ) ;
#22013 = CARTESIAN_POINT ( 'NONE',  ( 33.78010750773675852, -5.407089921784861808, 160.2588333874741124 ) ) ;
#22014 = EDGE_CURVE ( 'NONE', #23018, #20125, #25729, .T. ) ;
#22015 = CARTESIAN_POINT ( 'NONE',  ( -53.55877896937850124, 212.1620413398627534, -8.530955311639255356 ) ) ;
#22016 = CARTESIAN_POINT ( 'NONE',  ( 15.24356964374999990, 245.6968750006145115, 0.000000000000000000 ) ) ;
#22017 = PRODUCT_RELATED_PRODUCT_CATEGORY ( 'part', '', ( #28601 ) ) ;
#22018 = CARTESIAN_POINT ( 'NONE',  ( 13.56230152254411259, -5.196152422706632912, -2.962499998771017662 ) ) ;
#22019 = CARTESIAN_POINT ( 'NONE',  ( -65.63169563604516554, 210.1155267958017703, 6.500000000000000888 ) ) ;
#22020 = CARTESIAN_POINT ( 'NONE',  ( -7.228626920339069173, 130.8726862821014834, 10.49813415415989581 ) ) ;
#22021 = CARTESIAN_POINT ( 'NONE',  ( 19.56230152254410370, 5.196152422706631135, -2.287499998770980980 ) ) ;
#22022 = ORIENTED_EDGE ( 'NONE', *, *, #26383, .F. ) ;
#22023 = DIRECTION ( 'NONE',  ( 0.000000000000000000, 0.000000000000000000, 1.000000000000000000 ) ) ;
#22024 = DIRECTION ( 'NONE',  ( 0.9961946980917461003, 0.000000000000000000, -0.08715574274765142126 ) ) ;
#22025 = CARTESIAN_POINT ( 'NONE',  ( -8.632099005475501130, 124.5476862821014663, -13.23911966647218996 ) ) ;
#22026 = CARTESIAN_POINT ( 'NONE',  ( 7.234628195640295800, 197.8825961894323484, 27.00000000000001066 ) ) ;
#22027 = CARTESIAN_POINT ( 'NONE',  ( 10.49813415415989581, 18.17268628210144854, 7.228626920339068285 ) ) ;
#22028 = CARTESIAN_POINT ( 'NONE',  ( 13.56230152254411614, -5.196152422706638241, -9.825000000000056133 ) ) ;
#22029 = EDGE_LOOP ( 'NONE', ( #34517, #17885, #5942, #9864 ) ) ;
#22030 = DIRECTION ( 'NONE',  ( -0.000000000000000000, -1.000000000000000000, -0.000000000000000000 ) ) ;
#22031 = CARTESIAN_POINT ( 'NONE',  ( -2.064181346179269738, 84.29768628210146630, 9.465287035748067623 ) ) ;
#22032 =( GEOMETRIC_REPRESENTATION_CONTEXT ( 3 ) GLOBAL_UNCERTAINTY_ASSIGNED_CONTEXT ( ( #24495 ) ) GLOBAL_UNIT_ASSIGNED_CONTEXT ( ( #13895, #34347, #8945 ) ) REPRESENTATION_CONTEXT ( 'NONE', 'WORKASPACE' ) );
#22033 = DIRECTION ( 'NONE',  ( 1.000000000000000000, 0.000000000000000000, 0.000000000000000000 ) ) ;
#22034 = CARTESIAN_POINT ( 'NONE',  ( -9.534712964251895073, 126.3773137178985309, -1.715153634034446428 ) ) ;
#22035 = CARTESIAN_POINT ( 'NONE',  ( 13.62178482187499640, 195.6031250006145115, -23.59362340125807123 ) ) ;
#22036 = CARTESIAN_POINT ( 'NONE',  ( 20.99999999999999645, 0.000000000000000000, -8.000000000000000000 ) ) ;
#22037 = CARTESIAN_POINT ( 'NONE',  ( 27.24356964375000345, 198.2843750006145456, -3.336375036156643733E-15 ) ) ;
#22038 = CARTESIAN_POINT ( 'NONE',  ( 25.01414827068380475, -3.464101615137975543, 164.7242041589784947 ) ) ;
#22039 = VECTOR ( 'NONE', #36882, 1000.000000000000000 ) ;
#22040 = CARTESIAN_POINT ( 'NONE',  ( 20.99999999999999289, 242.2374999999999545, -5.999999999999997335 ) ) ;
#22041 = CARTESIAN_POINT ( 'NONE',  ( -6.840914352311947333, 53.63981371789855501, -6.594114490232462877 ) ) ;
#22042 = CARTESIAN_POINT ( 'NONE',  ( 37.14170668649535401, 7.347880794884125653E-16, 165.6582722084640125 ) ) ;
#22043 = ORIENTED_EDGE ( 'NONE', *, *, #19586, .F. ) ;
#22044 = CARTESIAN_POINT ( 'NONE',  ( 23.99999999999999645, 240.4562500012290513, -5.196152422706631135 ) ) ;
#22045 = CARTESIAN_POINT ( 'NONE',  ( 0.1745138560722779009, 59.38981371789856212, 12.50000000000000355 ) ) ;
#22046 = CARTESIAN_POINT ( 'NONE',  ( 19.68408634441911431, 5.407089921784862696, -6.646874999385543603 ) ) ;
#22047 = CARTESIAN_POINT ( 'NONE',  ( -13.62178482187500528, 198.3781250006145171, -23.59362340125807123 ) ) ;
#22048 = CARTESIAN_POINT ( 'NONE',  ( 18.12178482187499640, 4.985214923628404904, -6.628124999385476279 ) ) ;
#22049 = CARTESIAN_POINT ( 'NONE',  ( 12.46528703574811558, 38.40231371789855075, -2.660918448318005503 ) ) ;
#22050 = ORIENTED_EDGE ( 'NONE', *, *, #18769, .T. ) ;
#22051 = CARTESIAN_POINT ( 'NONE',  ( -10.49813415415989581, 13.57268628210145600, -7.228626920339068285 ) ) ;
#22052 = CARTESIAN_POINT ( 'NONE',  ( 37.60251119283397259, 7.646167579472024665E-16, 168.1306435695252901 ) ) ;
#22053 = CARTESIAN_POINT ( 'NONE',  ( -52.96502896937850124, 215.5714017266979567, -3.350049139982168800 ) ) ;
#22054 =( NAMED_UNIT ( * ) SI_UNIT ( $, .STERADIAN. ) SOLID_ANGLE_UNIT ( ) );
#22055 = PRODUCT_DEFINITION_FORMATION_WITH_SPECIFIED_SOURCE ( 'ANY', '', #23177, .NOT_KNOWN. ) ;
#22056 = CARTESIAN_POINT ( 'NONE',  ( 13.56230152254410548, 5.196152422706636465, -9.525000000000034106 ) ) ;
#22057 = CARTESIAN_POINT ( 'NONE',  ( -4.622313124798826500, 69.16481371789855359, 11.61527771782809637 ) ) ;
#22058 = CARTESIAN_POINT ( 'NONE',  ( -67.01711230271185116, 214.4690446883608104, -1.321298161741814914 ) ) ;
#22059 = COLOUR_RGB ( '',0.8941176470588234615, 0.8941176470588234615, 0.8941176470588234615 ) ;
#22060 = CARTESIAN_POINT ( 'NONE',  ( -55.14955436395487709, 214.8429017333601792, -4.673758765035196383 ) ) ;
#22061 = ADVANCED_FACE ( 'NONE', ( #30283 ), #4499, .T. ) ;
#22062 = CARTESIAN_POINT ( 'NONE',  ( 13.56230152254410548, 5.196152422706630247, -1.762499998771011045 ) ) ;
#22063 = PLANE ( 'NONE',  #20425 ) ;
#22064 = CARTESIAN_POINT ( 'NONE',  ( 0.1745138560722461762, 31.78981371789855004, 15.50000000000000533 ) ) ;
#22065 = CARTESIAN_POINT ( 'NONE',  ( -42.27752896937850835, 214.3500491399821897, 7.303452534266821949 ) ) ;
#22066 = LINE ( 'NONE', #33617, #31663 ) ;
#22067 = CARTESIAN_POINT ( 'NONE',  ( 7.228626920339068285, 71.07268628210144357, -10.49813415415989581 ) ) ;
#22068 = CARTESIAN_POINT ( 'NONE',  ( -3.257655550457281723, 10.69768628210143646, 15.46528703574804986 ) ) ;
#22069 = CARTESIAN_POINT ( 'NONE',  ( 16.56230152254411436, 6.928203230275514990, -1.462500000000010125 ) ) ;
#22070 = CARTESIAN_POINT ( 'NONE',  ( -27.99288911131838731, 207.4183503646231941, -7.576574741737489127 ) ) ;
#22071 = ORIENTED_EDGE ( 'NONE', *, *, #2863, .T. ) ;
#22072 = CARTESIAN_POINT ( 'NONE',  ( 15.53471296425195369, 26.22268628210144925, -2.908627838312120684 ) ) ;
#22073 = CARTESIAN_POINT ( 'NONE',  ( -13.62178482187500528, 195.6781250006145569, -23.59362340125807123 ) ) ;
#22074 = CARTESIAN_POINT ( 'NONE',  ( 27.24356964375000345, 199.1843750006145228, -3.336375036156643733E-15 ) ) ;
#22075 = CARTESIAN_POINT ( 'NONE',  ( 20.99999999999998579, 247.6374999999999886, -5.999999999999997335 ) ) ;
#22076 = CARTESIAN_POINT ( 'NONE',  ( 7.234628195640363302, 195.4799038117967029, -26.99999999999996803 ) ) ;
#22077 = EDGE_CURVE ( 'NONE', #22146, #11399, #22899, .T. ) ;
#22078 = FACE_OUTER_BOUND ( 'NONE', #29860, .T. ) ;
#22079 = CARTESIAN_POINT ( 'NONE',  ( 2.311890736173175753, 10.12268628210144428, 12.53471296425194836 ) ) ;
#22080 = CARTESIAN_POINT ( 'NONE',  ( 15.24356964374999990, 246.6718750006145342, -3.323476615752268604 ) ) ;
#22081 = CARTESIAN_POINT ( 'NONE',  ( 3.796722387233182339, 114.0148137178985763, 8.710071997420207879 ) ) ;
#22082 = CARTESIAN_POINT ( 'NONE',  ( 15.24356964374999990, 245.3218750006145399, -3.323476615752268604 ) ) ;
#22083 = EDGE_CURVE ( 'NONE', #12855, #15992, #19113, .T. ) ;
#22084 = ORIENTED_EDGE ( 'NONE', *, *, #27303, .F. ) ;
#22085 = CARTESIAN_POINT ( 'NONE',  ( 19.39230484541326049, 249.5138461906614111, -5.999999999999995559 ) ) ;
#22086 = CARTESIAN_POINT ( 'NONE',  ( 26.99999999999999645, 249.3437500012290400, 3.464101615137751278 ) ) ;
#22087 = CARTESIAN_POINT ( 'NONE',  ( -11.61527771782809282, 135.8648137178985849, -4.622313124798832717 ) ) ;
#22088 = CARTESIAN_POINT ( 'NONE',  ( 10.31873187879411091, 3.604726614523236616, -9.628124999385549998 ) ) ;
#22089 = CARTESIAN_POINT ( 'NONE',  ( 37.29692136982500728, 3.604726614523238837, 164.6377359093410746 ) ) ;
#22090 = CARTESIAN_POINT ( 'NONE',  ( 22.60769515458672885, 240.7388461906613770, 5.999999999999997335 ) ) ;
#22091 = CARTESIAN_POINT ( 'NONE',  ( -27.00000000000000355, 196.8125000000000000, -15.58845726811989429 ) ) ;
#22092 = EDGE_LOOP ( 'NONE', ( #8112, #18242, #25000, #18421 ) ) ;
#22093 = CARTESIAN_POINT ( 'NONE',  ( 4.622313124798573369, 28.23518628210144854, 11.61527771782819940 ) ) ;
#22094 = EDGE_LOOP ( 'NONE', ( #24967, #13137, #377, #10008 ) ) ;
#22095 = ORIENTED_EDGE ( 'NONE', *, *, #26724, .F. ) ;
#22096 = CARTESIAN_POINT ( 'NONE',  ( 18.00000000000000000, 5.196152422706630247, -4.968749998770949361 ) ) ;
#22097 = CARTESIAN_POINT ( 'NONE',  ( 15.24356964375000167, -3.323476615752272600, -0.5531249993854806535 ) ) ;
#22098 = CARTESIAN_POINT ( 'NONE',  ( 15.00000000000000000, 0.000000000000000000, -1.349999999999990097 ) ) ;
#22099 = CARTESIAN_POINT ( 'NONE',  ( 20.99999999999999645, 185.0294372515228645, -5.999999999999999112 ) ) ;
#22100 = CARTESIAN_POINT ( 'NONE',  ( 15.24356964374999990, 249.2593750006145115, -3.323476615752268604 ) ) ;
#22101 = CARTESIAN_POINT ( 'NONE',  ( 7.228626920339068285, 71.07268628210144357, -10.49813415415989581 ) ) ;
#22102 = CARTESIAN_POINT ( 'NONE',  ( 15.53471296425195369, 136.6226862821014549, -2.908627838312120684 ) ) ;
#22103 = CARTESIAN_POINT ( 'NONE',  ( -67.01711230271183695, 216.4690446883607535, -1.857196546604089393 ) ) ;
#22104 = CARTESIAN_POINT ( 'NONE',  ( 14.06542688028853405, 216.9345731196990243, 0.01200585063896637480 ) ) ;
#22105 = CARTESIAN_POINT ( 'NONE',  ( -53.95461230271185116, 208.6787018382582346, -4.469044688360757966 ) ) ;
#22106 = CARTESIAN_POINT ( 'NONE',  ( 7.234628195640363302, 197.1674038105676914, -26.99999999999996803 ) ) ;
#22107 = CARTESIAN_POINT ( 'NONE',  ( 37.03058311459920304, -3.464101615137751278, 164.3881239696214038 ) ) ;
#22108 = CARTESIAN_POINT ( 'NONE',  ( -8.715434833792127023, 115.7398137178985706, 8.962234695871568846 ) ) ;
#22109 = CARTESIAN_POINT ( 'NONE',  ( -69.39955436395489130, 213.3788001182225003, -3.209657149897400252 ) ) ;
#22110 = CARTESIAN_POINT ( 'NONE',  ( -62.47247103062156981, 205.6499508600178956, 7.303452534266880569 ) ) ;
#22111 = EDGE_CURVE ( 'NONE', #11470, #3008, #20468, .T. ) ;
#22112 = CARTESIAN_POINT ( 'NONE',  ( 23.87821517812500005, -4.985214923628404016, -2.353124999385475036 ) ) ;
#22113 = CARTESIAN_POINT ( 'NONE',  ( 13.62178482187499640, 195.1531250006145513, -23.59362340125807123 ) ) ;
#22114 = CARTESIAN_POINT ( 'NONE',  ( 15.46528703574811736, 93.60231371789855359, -3.257655550456947768 ) ) ;
#22115 = CARTESIAN_POINT ( 'NONE',  ( -43.06919563604516554, 216.5000000000000000, -0.1155267958017906493 ) ) ;
#22116 = VERTEX_POINT ( 'NONE', #19485 ) ;
#22117 = VECTOR ( 'NONE', #25705, 1000.000000000000000 ) ;
#22118 = CARTESIAN_POINT ( 'NONE',  ( 2.660918448318279950, 125.6976862821014578, -12.46528703574805697 ) ) ;
#22119 = CARTESIAN_POINT ( 'NONE',  ( -10.83675517735155047, 59.86018628210145209, -11.08355503943142750 ) ) ;
#22120 = VECTOR ( 'NONE', #26115, 1000.000000000000000 ) ;
#22121 = CARTESIAN_POINT ( 'NONE',  ( 17.00000000000002132, 2.343145750507694913, 50.17464377163449285 ) ) ;
#22122 = CARTESIAN_POINT ( 'NONE',  ( 28.01132750018552287, 5.407089921784862696, 165.9583038997966185 ) ) ;
#22123 = CARTESIAN_POINT ( 'NONE',  ( -13.04141134922759804, 87.17268628210142367, -8.927990412390657937 ) ) ;
#22124 = CARTESIAN_POINT ( 'NONE',  ( -50.20163769728823411, 215.6869285224996986, -3.149950860017881382 ) ) ;
#22125 = CARTESIAN_POINT ( 'NONE',  ( 10.31873187879410914, 0.000000000000000000, -5.540624999385540761 ) ) ;
#22126 =( BOUNDED_CURVE ( )  B_SPLINE_CURVE ( 2, ( #300, #29485, #29295, #34987, #3333 ),
 .UNSPECIFIED., .F., .F. ) 
 B_SPLINE_CURVE_WITH_KNOTS ( ( 3, 2, 3 ),
 ( 0.9565217391304334793, 0.9637681159420286026, 0.9662082966761268432 ),
 .UNSPECIFIED. ) 
 CURVE ( )  GEOMETRIC_REPRESENTATION_ITEM ( )  RATIONAL_B_SPLINE_CURVE ( ( 1.000000000000024647, 0.8660254037844140607, 1.000000000000000000, 0.9548847324609615050, 0.9401541411607547971 ) ) 
 REPRESENTATION_ITEM ( '' )  );
#22127 = CARTESIAN_POINT ( 'NONE',  ( 3.796722387233379514, 43.18518628210144072, -8.710071997420127943 ) ) ;
#22128 = CARTESIAN_POINT ( 'NONE',  ( 10.56230152254410726, 0.000000000000000000, -7.650000000000045652 ) ) ;
#22129 = CARTESIAN_POINT ( 'NONE',  ( -60.69122103062155560, 208.3738570449993404, -6.530955311639226935 ) ) ;
#22130 = EDGE_CURVE ( 'NONE', #30675, #28137, #15699, .T. ) ;
#22131 = CARTESIAN_POINT ( 'NONE',  ( -7.234628195640316228, 198.6700961906613543, -27.00000000000000000 ) ) ;
#22132 = CARTESIAN_POINT ( 'NONE',  ( 11.48171059495397728, 54.68518628210144783, 4.944772684328674117 ) ) ;
#22133 = CARTESIAN_POINT ( 'NONE',  ( -27.00000000000000355, 199.0999999999999943, 0.000000000000000000 ) ) ;
#22134 = CARTESIAN_POINT ( 'NONE',  ( 19.56230152254412147, 5.196152422706637353, -6.900000000000044764 ) ) ;
#22136 = CARTESIAN_POINT ( 'NONE',  ( 19.68408634441912142, -5.407089921784861808, -1.846874999385544891 ) ) ;
#22135 = CARTESIAN_POINT ( 'NONE',  ( 8.152565276336714462, 34.84768628210143504, -5.233372021372432847 ) ) ;
#22137 = DIRECTION ( 'NONE',  ( -0.000000000000000000, -1.000000000000000000, -0.000000000000000000 ) ) ;
#22138 = ORIENTED_EDGE ( 'NONE', *, *, #23847, .F. ) ;
#22139 = CARTESIAN_POINT ( 'NONE',  ( 26.99999999999999645, 3.464101615137755275, -2.437499999999996003 ) ) ;
#22140 = CARTESIAN_POINT ( 'NONE',  ( 24.74781001545762393, 3.604726614523240613, 164.4745922192587670 ) ) ;
#22141 = CARTESIAN_POINT ( 'NONE',  ( 30.66448242393021673, 6.928203230275514990, 160.4655395846485249 ) ) ;
#22142 = CARTESIAN_POINT ( 'NONE',  ( 26.99999999999999645, 244.3750000000000000, -7.347880794884117764E-16 ) ) ;
#22143 = FACE_BOUND ( 'NONE', #32871, .T. ) ;
#22144 = CARTESIAN_POINT ( 'NONE',  ( -12.50000000000000355, 89.28981371789855359, 0.1745138560722786503 ) ) ;
#22145 = CARTESIAN_POINT ( 'NONE',  ( -12.50000000000000355, 86.31018628210145494, -0.1745138560725492671 ) ) ;
#22146 = VERTEX_POINT ( 'NONE', #24411 ) ;
#22147 = ORIENTED_EDGE ( 'NONE', *, *, #30201, .T. ) ;
#22148 = AXIS2_PLACEMENT_3D ( 'NONE', #23707, #17651, #9302 ) ;
#22149 = CARTESIAN_POINT ( 'NONE',  ( -27.00000000000000355, 198.7625000012290286, 0.000000000000000000 ) ) ;
#22150 = CARTESIAN_POINT ( 'NONE',  ( 18.00000000000000355, 248.7812500012290400, 5.196152422706632912 ) ) ;
#22151 = CARTESIAN_POINT ( 'NONE',  ( -11.08355503943118592, 53.63981371789855501, -10.83675517735179383 ) ) ;
#22152 = CARTESIAN_POINT ( 'NONE',  ( 15.24356964375000167, -3.323476615752272600, -9.665624999385482141 ) ) ;
#22153 = VECTOR ( 'NONE', #29623, 1000.000000000000000 ) ;
#22154 = CARTESIAN_POINT ( 'NONE',  ( 23.87821517812499650, 242.9593750006145285, -4.985214923628404904 ) ) ;
#22155 =( BOUNDED_CURVE ( )  B_SPLINE_CURVE ( 2, ( #35273, #9328, #591, #6861, #408, #18436, #11973, #15204, #15582 ),
 .UNSPECIFIED., .F., .F. ) 
 B_SPLINE_CURVE_WITH_KNOTS ( ( 3, 2, 2, 2, 3 ),
 ( 0.1195652173913043653, 0.1231884057971014551, 0.1304347826086956486, 0.1376811594202898559, 0.1413043478260869457 ),
 .UNSPECIFIED. ) 
 CURVE ( )  GEOMETRIC_REPRESENTATION_ITEM ( )  RATIONAL_B_SPLINE_CURVE ( ( 0.9330127018922194093, 0.9330127018922196314, 1.000000000000000000, 0.8660254037844387076, 1.000000000000000000, 0.8660254037844387076, 1.000000000000000000, 0.9330127018922196314, 0.9330127018922194093 ) ) 
 REPRESENTATION_ITEM ( '' )  );
#22156 = CARTESIAN_POINT ( 'NONE',  ( -59.89955436395489841, 213.3788001182225003, -3.209657149897400252 ) ) ;
#22157 = EDGE_CURVE ( 'NONE', #21280, #149, #17371, .T. ) ;
#22158 = CARTESIAN_POINT ( 'NONE',  ( 22.56230152254411792, 7.347880794884125653E-16, -1.575000000000048583 ) ) ;
#22159 = CARTESIAN_POINT ( 'NONE',  ( 3.474262827703532341, 46.16481371789854649, -8.843639120294245259 ) ) ;
#22160 = CARTESIAN_POINT ( 'NONE',  ( 10.31873187879411091, 3.604726614523236616, -7.378124999385538452 ) ) ;
#22161 = CARTESIAN_POINT ( 'NONE',  ( -7.954856959092309943, 88.42731371789855643, 5.529263428287300108 ) ) ;
#22162 = CARTESIAN_POINT ( 'NONE',  ( -27.24356964375000345, 198.9593750006145285, 0.000000000000000000 ) ) ;
#22163 = CARTESIAN_POINT ( 'NONE',  ( -2.660918448318004614, 8.502313717898557499, -12.46528703574811558 ) ) ;
#22164 = CARTESIAN_POINT ( 'NONE',  ( 11.61527771782819940, 71.93518628210145494, -4.622313124798573369 ) ) ;
#22165 = CARTESIAN_POINT ( 'NONE',  ( 16.56230152254411436, 6.928203230275506996, -7.649999998770994125 ) ) ;
#22166 = CARTESIAN_POINT ( 'NONE',  ( -4.500000000000000888, 210.0000000000000000, 0.000000000000000000 ) ) ;
#22167 = CARTESIAN_POINT ( 'NONE',  ( 24.52066036092156054, 0.000000000000000000, 161.8782597873571660 ) ) ;
#22168 = CARTESIAN_POINT ( 'NONE',  ( 2.999999999999997335, 244.5000000000000000, 2.500000000000000000 ) ) ;
#22169 = CARTESIAN_POINT ( 'NONE',  ( 19.68408634441911431, 5.407089921784862696, -7.096874999385549998 ) ) ;
#22170 = DIRECTION ( 'NONE',  ( 0.000000000000000000, 0.000000000000000000, 1.000000000000000000 ) ) ;
#22171 = CARTESIAN_POINT ( 'NONE',  ( 37.29858702344112231, 7.347880794884125653E-16, 167.4514226650291562 ) ) ;
#22172 = CARTESIAN_POINT ( 'NONE',  ( -8.710071997420127943, 86.88518628210145778, -3.796722387233380402 ) ) ;
#22173 = LINE ( 'NONE', #10967, #4947 ) ;
#22174 = CIRCLE ( 'NONE', #35459, 8.000000000000000000 ) ;
#22175 = CARTESIAN_POINT ( 'NONE',  ( 4.622313124798573369, 120.2351862821014663, 11.61527771782819940 ) ) ;
#22176 = CARTESIAN_POINT ( 'NONE',  ( 23.99999999999999645, 248.5562500012290457, -5.196152422706631135 ) ) ;
#22177 = EDGE_LOOP ( 'NONE', ( #19948, #17103, #29439, #22281 ) ) ;
#22178 = CARTESIAN_POINT ( 'NONE',  ( 31.08364707426076023, 7.209453229046475009, 165.2566134613956876 ) ) ;
#22179 = CARTESIAN_POINT ( 'NONE',  ( 23.87821517812499650, 4.985214923628404904, -6.140624999385474680 ) ) ;
#22180 = CARTESIAN_POINT ( 'NONE',  ( 13.62178482187499640, 197.9093750006145456, -23.59362340125807123 ) ) ;
#22181 = DIRECTION ( 'NONE',  ( -1.000000000000000000, 0.000000000000000000, -0.000000000000000000 ) ) ;
#22182 = CARTESIAN_POINT ( 'NONE',  ( 28.31976137920325698, -5.196152422706638241, 168.0863951450442642 ) ) ;
#22183 = DIRECTION ( 'NONE',  ( 0.000000000000000000, 0.000000000000000000, -1.000000000000000000 ) ) ;
#22184 = CARTESIAN_POINT ( 'NONE',  ( 18.12178482187500350, 242.2843750006145456, 4.985214923628407568 ) ) ;
#22185 = CARTESIAN_POINT ( 'NONE',  ( 29.49159713443669162, 6.148716367659647020, 159.4989838507731008 ) ) ;
#22186 = CARTESIAN_POINT ( 'NONE',  ( 12.53471296425189330, 140.1773137178985849, 2.311890736173451977 ) ) ;
#22187 = CARTESIAN_POINT ( 'NONE',  ( -13.62178482187500528, 195.7343750006145626, -23.59362340125807123 ) ) ;
#22189 = EDGE_LOOP ( 'NONE', ( #24463, #5066, #32610, #2592 ) ) ;
#22188 = ORIENTED_EDGE ( 'NONE', *, *, #22471, .F. ) ;
#22190 =( BOUNDED_CURVE ( )  B_SPLINE_CURVE ( 2, ( #11246, #14096, #13915, #2529, #10498, #34183, #25466, #19247, #28121 ),
 .UNSPECIFIED., .F., .F. ) 
 B_SPLINE_CURVE_WITH_KNOTS ( ( 3, 2, 2, 2, 3 ),
 ( 0.7708333333333333703, 0.7777777777777777901, 0.7916666666666666297, 0.8055555555555555802, 0.8125000000000000000 ),
 .UNSPECIFIED. ) 
 CURVE ( )  GEOMETRIC_REPRESENTATION_ITEM ( )  RATIONAL_B_SPLINE_CURVE ( ( 0.9330127018922192983, 0.9330127018922198534, 1.000000000000000000, 0.8660254037844387076, 1.000000000000000000, 0.8660254037844387076, 1.000000000000000000, 0.9330127018922194093, 0.9330127018922194093 ) ) 
 REPRESENTATION_ITEM ( '' )  );
#22191 = CARTESIAN_POINT ( 'NONE',  ( 18.12178482187499640, 244.7218750006145171, -4.985214923628404904 ) ) ;
#22192 = AXIS2_PLACEMENT_3D ( 'NONE', #8576, #31691, #13900 ) ;
#22193 = CARTESIAN_POINT ( 'NONE',  ( 3.306546357697853733E-15, 210.0000000000000284, 27.00000000000000000 ) ) ;
#22194 = CARTESIAN_POINT ( 'NONE',  ( 15.24356964375000167, -3.323476615752272600, -5.053124999385469884 ) ) ;
#22195 = CARTESIAN_POINT ( 'NONE',  ( -2.908627838312453306, 114.8773137178985735, 15.53471296425188797 ) ) ;
#22196 = CARTESIAN_POINT ( 'NONE',  ( 22.60769515458672885, 244.2825961894323541, 5.999999999999997335 ) ) ;
#22197 = CARTESIAN_POINT ( 'NONE',  ( 21.00000000000000000, -6.928203230275506996, -10.18124999877096570 ) ) ;
#22198 = CARTESIAN_POINT ( 'NONE',  ( 16.56230152254411436, 7.209453229046482114, -8.409374999385503813 ) ) ;
#22199 = ORIENTED_EDGE ( 'NONE', *, *, #2054, .T. ) ;
#22200 = CARTESIAN_POINT ( 'NONE',  ( 13.49999999999999645, 198.1625000012290343, -23.38268590217984766 ) ) ;
#22201 = CARTESIAN_POINT ( 'NONE',  ( 8.962234695871762469, 108.1601862821014635, -8.715434833791931624 ) ) ;
#22202 = CARTESIAN_POINT ( 'NONE',  ( 10.31873187879410914, 0.000000000000000000, -1.040624999385536542 ) ) ;
#22203 = CARTESIAN_POINT ( 'NONE',  ( -46.82961230271182984, 212.3930949314663792, 8.469044688360751749 ) ) ;
#22204 = CARTESIAN_POINT ( 'NONE',  ( 26.75643035624999655, 243.1843750006145513, 3.323476615752267271 ) ) ;
#22205 = CARTESIAN_POINT ( 'NONE',  ( -27.00000000000000355, 197.3750000012290400, -15.58845726811989429 ) ) ;
#22206 = CARTESIAN_POINT ( 'NONE',  ( -35.15252896937850124, 207.6499508600178387, -3.839350919129087547 ) ) ;
#22207 = CARTESIAN_POINT ( 'NONE',  ( -11.48171059495397373, 114.4851862821014521, -4.944772684328680334 ) ) ;
#22208 = CARTESIAN_POINT ( 'NONE',  ( 13.56230152254411614, -5.196152422706632912, -1.162499998771021614 ) ) ;
#22209 = ORIENTED_EDGE ( 'NONE', *, *, #20954, .F. ) ;
#22210 = CARTESIAN_POINT ( 'NONE',  ( -38.52455436395488420, 205.1570982666397356, 4.673758765035198159 ) ) ;
#22211 = CARTESIAN_POINT ( 'NONE',  ( 0.000000000000000000, 148.0000000000000000, 0.000000000000000000 ) ) ;
#22212 = CARTESIAN_POINT ( 'NONE',  ( 15.46528703574804986, 118.7976862821014521, 3.257655550457285720 ) ) ;
#22213 = CIRCLE ( 'NONE', #21618, 2.649999999999994582 ) ;
#22214 = DIRECTION ( 'NONE',  ( 0.000000000000000000, 1.000000000000000000, 0.000000000000000000 ) ) ;
#22215 = CARTESIAN_POINT ( 'NONE',  ( 12.50000000000000355, 17.31018628210144428, 0.1745138560725507937 ) ) ;
#22216 = CARTESIAN_POINT ( 'NONE',  ( 10.56230152254410903, 3.464101615137757051, -9.037500000000038725 ) ) ;
#22217 = EDGE_LOOP ( 'NONE', ( #2125, #429 ) ) ;
#22218 = CARTESIAN_POINT ( 'NONE',  ( 6.840914352312096547, 80.56018628210146915, -6.594114490232313663 ) ) ;
#22219 = CARTESIAN_POINT ( 'NONE',  ( 7.954856959092311719, 129.8273137178985905, -5.529263428287300108 ) ) ;
#22220 = EDGE_CURVE ( 'NONE', #18566, #20367, #37072, .T. ) ;
#22221 = CARTESIAN_POINT ( 'NONE',  ( 5.778771075727756162E-15, 196.3156250006145171, 31.45816453501075927 ) ) ;
#22222 = CARTESIAN_POINT ( 'NONE',  ( 24.61867908796596183, 0.000000000000000000, 160.2039707163872038 ) ) ;
#22223 = CARTESIAN_POINT ( 'NONE',  ( 27.24356964375000700, 197.7968750006145342, 15.72908226750537075 ) ) ;
#22224 = DIRECTION ( 'NONE',  ( -0.000000000000000000, -1.000000000000000000, -0.000000000000000000 ) ) ;
#22225 = EDGE_CURVE ( 'NONE', #31527, #7301, #8387, .T. ) ;
#22226 = CARTESIAN_POINT ( 'NONE',  ( 27.66282496834995186, -5.196152422706632912, 160.5775776094020557 ) ) ;
#22227 = CARTESIAN_POINT ( 'NONE',  ( 3.796722387233182339, 58.81481371789855217, 8.710071997420207879 ) ) ;
#22228 = CARTESIAN_POINT ( 'NONE',  ( 15.00000000000000000, 0.000000000000000000, -8.550000000000002487 ) ) ;
#22229 = ORIENTED_EDGE ( 'NONE', *, *, #17031, .T. ) ;
#22230 = VECTOR ( 'NONE', #9937, 1000.000000000000000 ) ;
#22231 = CARTESIAN_POINT ( 'NONE',  ( 18.00000000000000355, 241.5812500012290513, 5.196152422706632912 ) ) ;
#22232 = CARTESIAN_POINT ( 'NONE',  ( -7.228626920338836470, 63.12731371789855217, -10.49813415416005213 ) ) ;
#22233 = CARTESIAN_POINT ( 'NONE',  ( 22.80587116629411781, -3.604726614523238837, -5.859374999385517313 ) ) ;
#22234 = CARTESIAN_POINT ( 'NONE',  ( 13.62178482187499640, 198.3031250006145285, -23.59362340125807123 ) ) ;
#22235 = CARTESIAN_POINT ( 'NONE',  ( 26.75643035624999655, 7.049594010296217766E-16, -7.678124999385471661 ) ) ;
#22236 = CARTESIAN_POINT ( 'NONE',  ( 7.228626920338837358, 30.92731371789854222, 10.49813415416005036 ) ) ;
#22237 = EDGE_CURVE ( 'NONE', #33229, #17991, #35293, .T. ) ;
#22238 = ORIENTED_EDGE ( 'NONE', *, *, #32869, .T. ) ;
#22239 = UNCERTAINTY_MEASURE_WITH_UNIT (LENGTH_MEASURE( 1.000000000000000082E-05 ), #8806, 'distance_accuracy_value', 'NONE');
#22240 = CARTESIAN_POINT ( 'NONE',  ( 22.80587116629411426, 3.604726614523243278, -2.184374999385525040 ) ) ;
#22241 = CIRCLE ( 'NONE', #8907, 7.500000000000000000 ) ;
#22242 = CARTESIAN_POINT ( 'NONE',  ( -10.69584247140444866, 11.84768628210144925, 6.932735513423972762 ) ) ;
#22243 = CARTESIAN_POINT ( 'NONE',  ( 31.37289519550453321, -7.209453229046482114, 168.5627346156876740 ) ) ;
#22244 = CARTESIAN_POINT ( 'NONE',  ( -47.22544563604515844, 214.8429017333602360, 4.673758765035156415 ) ) ;
#22245 = CARTESIAN_POINT ( 'NONE',  ( -13.50000000000000533, 196.3249999999999886, -23.38268590217984411 ) ) ;
#22246 = CARTESIAN_POINT ( 'NONE',  ( -4.944772684328424539, 63.41481371789856070, -11.48171059495408031 ) ) ;
#22247 = CARTESIAN_POINT ( 'NONE',  ( -40.50372103062156981, 214.5309553116392749, -1.090244570138262148 ) ) ;
#22248 = CARTESIAN_POINT ( 'NONE',  ( -53.56622103062157692, 211.6261429550005744, 6.530955311639227823 ) ) ;
#22249 = CARTESIAN_POINT ( 'NONE',  ( -3.253724281355068545E-15, 195.9500000012290002, -27.00000000000000000 ) ) ;
#22250 = CARTESIAN_POINT ( 'NONE',  ( 24.82458453031440726, 0.000000000000000000, 162.5574806918533000 ) ) ;
#22251 = CARTESIAN_POINT ( 'NONE',  ( -14.38691631536193860, 43.86481371789854933, -5.770363421894132649 ) ) ;
#22252 = CARTESIAN_POINT ( 'NONE',  ( -34.36086230271182984, 214.1499508600178387, -7.418979330068641964 ) ) ;
#22253 = CARTESIAN_POINT ( 'NONE',  ( -12.50000000000000355, 21.91018628210143859, -0.1745138560725492671 ) ) ;
#22254 = DIRECTION ( 'NONE',  ( 0.000000000000000000, -1.000000000000000000, 0.000000000000000000 ) ) ;
#22255 = CARTESIAN_POINT ( 'NONE',  ( 6.932735513423970097, 73.94768628210145778, 10.69584247140445044 ) ) ;
#22256 = CARTESIAN_POINT ( 'NONE',  ( 15.53471296425195369, 7.822686282101448896, -2.908627838312120684 ) ) ;
#22257 = CARTESIAN_POINT ( 'NONE',  ( 19.56230152254412502, -5.196152422706635576, -2.100000000000074252 ) ) ;
#22258 = CARTESIAN_POINT ( 'NONE',  ( 18.00000000000000355, 244.2812500012290400, 5.196152422706632912 ) ) ;
#22259 = ORIENTED_EDGE ( 'NONE', *, *, #18430, .F. ) ;
#22260 = CARTESIAN_POINT ( 'NONE',  ( 13.04141134922759804, 36.57268628210144357, 8.927990412390657937 ) ) ;
#22261 = CARTESIAN_POINT ( 'NONE',  ( 27.24356964374999279, 195.5656250006145171, -15.72908226750539207 ) ) ;
#22262 = CARTESIAN_POINT ( 'NONE',  ( 27.24356964375000700, 197.3468750006145740, 15.72908226750537075 ) ) ;
#22263 = FACE_OUTER_BOUND ( 'NONE', #33582, .T. ) ;
#22264 = CARTESIAN_POINT ( 'NONE',  ( 16.56230152254410726, 0.000000000000000000, -10.00000000000000000 ) ) ;
#22265 = CARTESIAN_POINT ( 'NONE',  ( 7.234628195640269155, 196.1950961906613600, 27.00000000000003197 ) ) ;
#22266 = CARTESIAN_POINT ( 'NONE',  ( 26.75643035624999655, 248.6968750006145115, 3.323476615752267715 ) ) ;
#22267 = CARTESIAN_POINT ( 'NONE',  ( -1.715153634034442431, 114.8773137178985735, 9.534712964251900402 ) ) ;
#22268 = CARTESIAN_POINT ( 'NONE',  ( 26.75643035624999655, 240.6343750006145115, -7.049594010296217766E-16 ) ) ;
#22269 = VERTEX_POINT ( 'NONE', #611 ) ;
#22270 = CARTESIAN_POINT ( 'NONE',  ( -61.48288769728821990, 203.5309553116391612, -1.857196546604028775 ) ) ;
#22271 = PRESENTATION_STYLE_ASSIGNMENT (( #10693 ) ) ;
#22272 = CARTESIAN_POINT ( 'NONE',  ( 26.99999999999999645, 248.0312500012290400, -7.347880794884117764E-16 ) ) ;
#22273 = CARTESIAN_POINT ( 'NONE',  ( -6.932735513424201912, 124.6523137178985650, 10.69584247140429412 ) ) ;
#22274 = CARTESIAN_POINT ( 'NONE',  ( 10.31873187879411091, 3.604726614523236616, -8.728124999385524774 ) ) ;
#22275 = CARTESIAN_POINT ( 'NONE',  ( 27.63710252976279591, -5.407089921784859143, 161.6808929148651828 ) ) ;
#22276 = CARTESIAN_POINT ( 'NONE',  ( 15.24356964375000167, -3.323476615752272600, -0.6656249993855035685 ) ) ;
#22277 = CARTESIAN_POINT ( 'NONE',  ( 27.00000000000001066, 196.5875000000000341, 15.58845726811988897 ) ) ;
#22278 = ORIENTED_EDGE ( 'NONE', *, *, #23148, .T. ) ;
#22279 = CARTESIAN_POINT ( 'NONE',  ( -2.660918448318275509, 38.29768628210145209, 12.46528703574805874 ) ) ;
#22280 = ORIENTED_EDGE ( 'NONE', *, *, #17949, .F. ) ;
#22281 = ORIENTED_EDGE ( 'NONE', *, *, #10401, .T. ) ;
#22282 = CARTESIAN_POINT ( 'NONE',  ( 26.99999999999999645, 7.347880794884117764E-16, -3.768749998770942966 ) ) ;
#22283 = CARTESIAN_POINT ( 'NONE',  ( 23.87821517812500005, -4.985214923628404016, -3.590624999385477523 ) ) ;
#22284 = DIRECTION ( 'NONE',  ( 0.000000000000000000, 0.000000000000000000, 1.000000000000000000 ) ) ;
#22285 = CARTESIAN_POINT ( 'NONE',  ( 15.24356964375000167, 248.8843750006145399, 3.323476615752272600 ) ) ;
#22286 = CARTESIAN_POINT ( 'NONE',  ( 8.715434833791931624, 64.46018628210146062, 8.962234695871760692 ) ) ;
#22287 = CARTESIAN_POINT ( 'NONE',  ( -65.82961230271182274, 211.8571965466040581, 6.469044688360755302 ) ) ;
#22288 = CARTESIAN_POINT ( 'NONE',  ( 6.017554903305191161, 215.6184169112603968, 2.114697272285289475 ) ) ;
#22289 = CARTESIAN_POINT ( 'NONE',  ( -57.71502896937850835, 213.8393509191290889, -2.350049139982142155 ) ) ;
#22290 = PRESENTATION_STYLE_ASSIGNMENT (( #18897 ) ) ;
#22291 = CARTESIAN_POINT ( 'NONE',  ( 36.95541128647934670, 7.347880794884117764E-16, 163.5289060425172636 ) ) ;
#22292 = CARTESIAN_POINT ( 'NONE',  ( -10.49813415416004858, 116.0273137178985650, 7.228626920338839135 ) ) ;
#22293 = CARTESIAN_POINT ( 'NONE',  ( -69.20163769728823411, 213.9548777149308592, -2.149950860017830756 ) ) ;
#22294 = CARTESIAN_POINT ( 'NONE',  ( -62.86830436395490551, 209.8844732041983150, 8.500000000000003553 ) ) ;
#22295 = CARTESIAN_POINT ( 'NONE',  ( 18.12178482187499640, 4.985214923628404904, -2.128124999385472282 ) ) ;
#22296 = CARTESIAN_POINT ( 'NONE',  ( 13.62178482187501416, 195.9031250006145513, 23.59362340125806767 ) ) ;
#22297 = VECTOR ( 'NONE', #10460, 1000.000000000000114 ) ;
#22298 = CARTESIAN_POINT ( 'NONE',  ( 15.53471296425188797, 103.3773137178985451, 2.908627838312457747 ) ) ;
#22299 = CARTESIAN_POINT ( 'NONE',  ( -34.36086230271183695, 213.1499508600178387, -5.686928522499747451 ) ) ;
#22300 = ORIENTED_EDGE ( 'NONE', *, *, #24256, .F. ) ;
#22301 = CARTESIAN_POINT ( 'NONE',  ( 36.83121435295620927, 3.464101615138126977, 162.1093285965122277 ) ) ;
#22302 = CARTESIAN_POINT ( 'NONE',  ( -6.932735513423968321, 115.3476862821014635, -10.69584247140445221 ) ) ;
#22303 = CARTESIAN_POINT ( 'NONE',  ( 14.38691631536207538, 62.73518628210145920, -5.770363421893813793 ) ) ;
#22304 = DIRECTION ( 'NONE',  ( 0.08715574274765150453, 0.000000000000000000, 0.9961946980917461003 ) ) ;
#22305 = CARTESIAN_POINT ( 'NONE',  ( 34.21152843433763024, -5.407089921784861808, 165.1899971430282505 ) ) ;
#22306 = CARTESIAN_POINT ( 'NONE',  ( -0.1745138560725817967, 84.01018628210145778, 15.50000000000000533 ) ) ;
#22307 = CARTESIAN_POINT ( 'NONE',  ( -43.47247103062156981, 206.6499508600178672, 5.571401726697986057 ) ) ;
#22308 = CARTESIAN_POINT ( 'NONE',  ( 19.68408634441910721, 5.407089921784857367, -7.490624999385548044 ) ) ;
#22309 = CARTESIAN_POINT ( 'NONE',  ( -7.954856959092191815, 13.57268628210145422, -5.529263428287477744 ) ) ;
#22310 = CARTESIAN_POINT ( 'NONE',  ( 0.000000000000000000, 210.0000000000000284, 0.000000000000000000 ) ) ;
#22311 = CARTESIAN_POINT ( 'NONE',  ( -57.52455436395488420, 205.1570982666397356, 4.673758765035198159 ) ) ;
#22312 = PRESENTATION_STYLE_ASSIGNMENT (( #8456 ) ) ;
#22313 = CARTESIAN_POINT ( 'NONE',  ( -4.944772684328673229, 66.18518628210144072, 11.48171059495397728 ) ) ;
#22314 = CARTESIAN_POINT ( 'NONE',  ( -13.49999999999998401, 196.9250000000000114, 23.38268590217985476 ) ) ;
#22315 = CARTESIAN_POINT ( 'NONE',  ( 20.99999999999999645, 185.0294372515228645, -5.999999999999999112 ) ) ;
#22317 = CARTESIAN_POINT ( 'NONE',  ( 22.80587116629411071, -3.604726614523238837, -1.359374999385495775 ) ) ;
#22316 = CARTESIAN_POINT ( 'NONE',  ( 3.474262827703335166, 19.03518628210144570, 8.843639120294326972 ) ) ;
#22318 = CARTESIAN_POINT ( 'NONE',  ( 18.00000000000000000, 241.8250000000000171, -5.196152422706630247 ) ) ;
#22319 = ORIENTED_EDGE ( 'NONE', *, *, #27087, .T. ) ;
#22320 = CARTESIAN_POINT ( 'NONE',  ( 15.00000000000000000, 0.000000000000000000, -2.700000000000008171 ) ) ;
#22321 = CARTESIAN_POINT ( 'NONE',  ( 26.78253581145591511, -0.6185957445801392174, -8.000000000000005329 ) ) ;
#22322 = CARTESIAN_POINT ( 'NONE',  ( 27.57990657358465114, 5.407089921784862696, 161.0271401442424803 ) ) ;
#22323 = CARTESIAN_POINT ( 'NONE',  ( 13.44051670066911264, 5.407089921784856479, -1.565624999385561988 ) ) ;
#22324 = CARTESIAN_POINT ( 'NONE',  ( 24.66116751255544060, -3.464101615137761048, 160.6896156317069426 ) ) ;
#22325 = CARTESIAN_POINT ( 'NONE',  ( 18.00000000000000355, 242.4250000000000114, 5.196152422706632912 ) ) ;
#22326 = FACE_OUTER_BOUND ( 'NONE', #7391, .T. ) ;
#22327 = CARTESIAN_POINT ( 'NONE',  ( -7.228626920338836470, 81.52731371789855075, -10.49813415416005213 ) ) ;
#22328 = CARTESIAN_POINT ( 'NONE',  ( 11.48171059495397728, 82.28518628210146346, 4.944772684328674117 ) ) ;
#22329 = VERTEX_POINT ( 'NONE', #804 ) ;
#22330 = ORIENTED_EDGE ( 'NONE', *, *, #28590, .F. ) ;
#22331 = CARTESIAN_POINT ( 'NONE',  ( 13.50000000000001421, 197.1125000012290513, 23.38268590217984055 ) ) ;
#22332 = CARTESIAN_POINT ( 'NONE',  ( 15.00000000000054712, 3.464101615138070134, -0.9375000000000270894 ) ) ;
#22333 = CARTESIAN_POINT ( 'NONE',  ( -2.908627838312453306, 50.47731371789854649, 15.53471296425188797 ) ) ;
#22334 = CARTESIAN_POINT ( 'NONE',  ( 23.87821517812500005, -4.985214923628404016, -9.103124999385482141 ) ) ;
#22335 = CARTESIAN_POINT ( 'NONE',  ( 18.12178482187500350, 242.2843750006145456, 4.985214923628407568 ) ) ;
#22336 = CARTESIAN_POINT ( 'NONE',  ( -62.67038769728824121, 208.6787018382581778, 4.469044688360752637 ) ) ;
#22337 = CARTESIAN_POINT ( 'NONE',  ( -27.00000000000000355, 199.6625000012290343, 0.000000000000000000 ) ) ;
#22338 = CARTESIAN_POINT ( 'NONE',  ( -0.1745138560723084320, 45.58981371789855785, -9.500000000000005329 ) ) ;
#22339 = CARTESIAN_POINT ( 'NONE',  ( 13.44051670066911619, -5.407089921784859143, -9.965624999385552130 ) ) ;
#22340 = EDGE_CURVE ( 'NONE', #15182, #1464, #29618, .T. ) ;
#22341 = CARTESIAN_POINT ( 'NONE',  ( 2.064181346179061460, 86.70231371789851949, 9.465287035748106703 ) ) ;
#22342 = CARTESIAN_POINT ( 'NONE',  ( -27.24356964374999635, 197.6468750006145285, 15.72908226750539384 ) ) ;
#22343 = CARTESIAN_POINT ( 'NONE',  ( -11.61527771782809282, 7.064813717898549505, -4.622313124798832717 ) ) ;
#22344 =( BOUNDED_CURVE ( )  B_SPLINE_CURVE ( 2, ( #35269, #29784, #6481, #12349, #18053, #29595, #3632, #15201, #35464 ),
 .UNSPECIFIED., .F., .F. ) 
 B_SPLINE_CURVE_WITH_KNOTS ( ( 3, 2, 2, 2, 3 ),
 ( 0.5208333333333333703, 0.5277777777777777901, 0.5416666666666666297, 0.5555555555555555802, 0.5625000000000000000 ),
 .UNSPECIFIED. ) 
 CURVE ( )  GEOMETRIC_REPRESENTATION_ITEM ( )  RATIONAL_B_SPLINE_CURVE ( ( 0.9330127018922192983, 0.9330127018922198534, 1.000000000000000000, 0.8660254037844387076, 1.000000000000000000, 0.8660254037844387076, 1.000000000000000000, 0.9330127018922194093, 0.9330127018922194093 ) ) 
 REPRESENTATION_ITEM ( '' )  );
#22345 = CARTESIAN_POINT ( 'NONE',  ( -10.49813415415989581, 59.57268628210145778, -7.228626920339068285 ) ) ;
#22346 = CARTESIAN_POINT ( 'NONE',  ( 13.56230152254410370, 5.196152422706630247, -7.612499998771005139 ) ) ;
#22347 = EDGE_CURVE ( 'NONE', #13899, #26761, #23376, .T. ) ;
#22348 = CARTESIAN_POINT ( 'NONE',  ( 25.08605175844997248, 3.464101615137603396, 165.5460647849041607 ) ) ;
#22349 = CARTESIAN_POINT ( 'NONE',  ( 36.90472052746056875, 3.604726614523238837, 160.1548597679282295 ) ) ;
#22350 = CARTESIAN_POINT ( 'NONE',  ( 37.15478004801428824, 3.464101615137938683, 165.8077014144021177 ) ) ;
#22351 = CARTESIAN_POINT ( 'NONE',  ( 22.80587116629411426, 7.646167579472024665E-16, -7.171874999385541294 ) ) ;
#22352 = CARTESIAN_POINT ( 'NONE',  ( -26.99999999999999645, 197.7874999999999943, 15.58845726811991561 ) ) ;
#22353 = CARTESIAN_POINT ( 'NONE',  ( 36.68413903717654279, 3.464101615138184265, 160.4282500447067434 ) ) ;
#22354 = CARTESIAN_POINT ( 'NONE',  ( -2.064181346179269738, 75.09768628210143504, 9.465287035748067623 ) ) ;
#22355 = FACE_OUTER_BOUND ( 'NONE', #17096, .T. ) ;
#22356 = EDGE_CURVE ( 'NONE', #34685, #25286, #35110, .T. ) ;
#22357 = CARTESIAN_POINT ( 'NONE',  ( 0.1745138560725515708, 107.0101862821014578, -12.50000000000000355 ) ) ;
#22358 = CARTESIAN_POINT ( 'NONE',  ( 22.56230152254410370, 0.000000000000000000, -10.00000000000000000 ) ) ;
#22359 = CARTESIAN_POINT ( 'NONE',  ( 10.49999999999999467, 215.7563705986615901, 5.555555555555558911 ) ) ;
#22360 = ORIENTED_EDGE ( 'NONE', *, *, #13190, .F. ) ;
#22361 = CARTESIAN_POINT ( 'NONE',  ( 34.21643094486717729, -5.407089921784855591, 165.2460330947959051 ) ) ;
#22362 = CARTESIAN_POINT ( 'NONE',  ( 23.87821517812499650, 4.985214923628404904, -4.340624999385478411 ) ) ;
#22363 = ADVANCED_FACE ( 'NONE', ( #23944, #32269 ), #29234, .F. ) ;
#22364 = CARTESIAN_POINT ( 'NONE',  ( 27.24356964374999279, 197.4218750006145342, -15.72908226750539207 ) ) ;
#22365 = CARTESIAN_POINT ( 'NONE',  ( 15.15508984909395451, -1.204559016176377728, -8.000000000000001776 ) ) ;
#22366 = CARTESIAN_POINT ( 'NONE',  ( 25.36059234810534235, 3.464101615137757051, 168.6840780838931835 ) ) ;
#22367 = CYLINDRICAL_SURFACE ( 'NONE', #5316, 5.999999999999998224 ) ;
#22368 = CARTESIAN_POINT ( 'NONE',  ( 18.12178482187500350, 240.9343750006145513, 4.985214923628407568 ) ) ;
#22369 = CARTESIAN_POINT ( 'NONE',  ( 10.56230152254410726, 0.000000000000000000, -7.087499998771007448 ) ) ;
#22370 =( BOUNDED_CURVE ( )  B_SPLINE_CURVE ( 3, ( #10159, #4468, #22425, #33285 ),
 .UNSPECIFIED., .F., .T. ) 
 B_SPLINE_CURVE_WITH_KNOTS ( ( 4, 4 ),
 ( 0.000000000000000000, 3.141592653589793116 ),
 .UNSPECIFIED. ) 
 CURVE ( )  GEOMETRIC_REPRESENTATION_ITEM ( )  RATIONAL_B_SPLINE_CURVE ( ( 1.000000000000000000, 0.3333333333333333703, 0.3333333333333333703, 1.000000000000000000 ) ) 
 REPRESENTATION_ITEM ( '' )  );
#22371 = CARTESIAN_POINT ( 'NONE',  ( -7.228626920338836470, 136.7273137178985678, -10.49813415416005213 ) ) ;
#22372 = CARTESIAN_POINT ( 'NONE',  ( -27.24356964375000345, 195.3593750006145342, 0.000000000000000000 ) ) ;
#22374 = EDGE_LOOP ( 'NONE', ( #1099, #13552, #1162, #27075 ) ) ;
#22373 = EDGE_LOOP ( 'NONE', ( #22772, #30540, #7473, #1515, #3179 ) ) ;
#22375 = CARTESIAN_POINT ( 'NONE',  ( 23.87821517812499650, 245.0968750006145171, -4.985214923628404904 ) ) ;
#22376 = CARTESIAN_POINT ( 'NONE',  ( 0.1745138560722779009, 13.38981371789854613, 12.50000000000000355 ) ) ;
#22377 = CARTESIAN_POINT ( 'NONE',  ( 15.24356964374999990, 0.000000000000000000, -5.090624999385479299 ) ) ;
#22378 = CARTESIAN_POINT ( 'NONE',  ( -15.50000000000000533, 116.8898137178985621, 0.1745138560722471477 ) ) ;
#22379 = CARTESIAN_POINT ( 'NONE',  ( 20.99999999999999289, 244.4874999999999829, -5.999999999999997335 ) ) ;
#22380 = CARTESIAN_POINT ( 'NONE',  ( 21.00000000000000000, -6.646953231504538984, -2.390624999385460470 ) ) ;
#22381 = CARTESIAN_POINT ( 'NONE',  ( 13.44051670066911264, -5.407089921784865361, -7.771874999385531169 ) ) ;
#22382 = CARTESIAN_POINT ( 'NONE',  ( -13.62178482187500528, 195.2281250006145399, -23.59362340125807123 ) ) ;
#22383 = CARTESIAN_POINT ( 'NONE',  ( 4.622313124798573369, 111.0351862821014635, 11.61527771782819940 ) ) ;
#22384 = CARTESIAN_POINT ( 'NONE',  ( 10.31873187879411091, 0.000000000000000000, -2.390624999385526639 ) ) ;
#22385 = CARTESIAN_POINT ( 'NONE',  ( -39.90252896937850124, 205.6499508600178103, -7.303452534266820173 ) ) ;
#22386 = CARTESIAN_POINT ( 'NONE',  ( 18.12178482187500350, 244.8718750006145228, 4.985214923628407568 ) ) ;
#22387 = ADVANCED_FACE ( 'NONE', ( #17506 ), #32650, .F. ) ;
#22388 = CARTESIAN_POINT ( 'NONE',  ( -37.92336230271182984, 213.9548777149308023, 2.149950860017852960 ) ) ;
#22389 = CARTESIAN_POINT ( 'NONE',  ( 0.1745138560725515708, 125.4101862821014635, -12.50000000000000355 ) ) ;
#22390 = CARTESIAN_POINT ( 'NONE',  ( 10.56230152254410726, 3.464101615137752166, -0.3749999987710042615 ) ) ;
#22391 = EDGE_CURVE ( 'NONE', #4778, #20196, #50, .T. ) ;
#22392 =( REPRESENTATION_RELATIONSHIP ('NONE','NONE', #4304, #8404 ) REPRESENTATION_RELATIONSHIP_WITH_TRANSFORMATION ( #18720 )SHAPE_REPRESENTATION_RELATIONSHIP( ) );
#22393 = CARTESIAN_POINT ( 'NONE',  ( -46.83705436395489841, 205.3262412349647263, -4.842901733360204020 ) ) ;
#22394 = CYLINDRICAL_SURFACE ( 'NONE', #5260, 6.000000000000001776 ) ;
#22395 = CARTESIAN_POINT ( 'NONE',  ( 13.04141134922759804, 128.5726862821014436, 8.927990412390657937 ) ) ;
#22396 = EDGE_CURVE ( 'NONE', #4196, #30479, #18076, .T. ) ;
#22397 = CARTESIAN_POINT ( 'NONE',  ( 26.99999999999999645, 242.6687500012290570, -3.464101615137755275 ) ) ;
#22398 = CARTESIAN_POINT ( 'NONE',  ( 12.46528703574805874, 17.59768628210143859, 2.660918448318279950 ) ) ;
#22399 = CARTESIAN_POINT ( 'NONE',  ( 16.56230152254411436, -6.928203230275514990, -8.437500000000024869 ) ) ;
#22401 = VERTEX_POINT ( 'NONE', #9536 ) ;
#22400 = VECTOR ( 'NONE', #8774, 1000.000000000000000 ) ;
#22402 = CARTESIAN_POINT ( 'NONE',  ( 20.99999999999999645, 248.7624999999999886, 5.999999999999998224 ) ) ;
#22403 = CARTESIAN_POINT ( 'NONE',  ( -8.843639120294326972, 76.53518628210146346, 3.474262827703335166 ) ) ;
#22404 =( BOUNDED_CURVE ( )  B_SPLINE_CURVE ( 2, ( #23559, #11987, #9722, #17689, #3834, #21106, #26387, #35286, #29613 ),
 .UNSPECIFIED., .F., .F. ) 
 B_SPLINE_CURVE_WITH_KNOTS ( ( 3, 2, 2, 2, 3 ),
 ( 0.2708333333333333703, 0.2777777777777777901, 0.2916666666666666852, 0.3055555555555555802, 0.3125000000000000000 ),
 .UNSPECIFIED. ) 
 CURVE ( )  GEOMETRIC_REPRESENTATION_ITEM ( )  RATIONAL_B_SPLINE_CURVE ( ( 0.9330127018922194093, 0.9330127018922196314, 1.000000000000000000, 0.8660254037844387076, 1.000000000000000000, 0.8660254037844387076, 1.000000000000000000, 0.9330127018922194093, 0.9330127018922194093 ) ) 
 REPRESENTATION_ITEM ( '' )  );
#22405 = EDGE_CURVE ( 'NONE', #10385, #16763, #29041, .T. ) ;
#22406 = CARTESIAN_POINT ( 'NONE',  ( -27.24356964375000345, 196.6531250006145513, 0.000000000000000000 ) ) ;
#22407 = LINE ( 'NONE', #22777, #32280 ) ;
#22408 = CARTESIAN_POINT ( 'NONE',  ( -13.62178482187500528, 197.5343750006145456, -23.59362340125807123 ) ) ;
#22409 = CARTESIAN_POINT ( 'NONE',  ( 19.39230484541326049, 249.9075961894323541, -5.999999999999997335 ) ) ;
#22410 = DIRECTION ( 'NONE',  ( 0.9961946980917462113, 0.000000000000000000, -0.08715574274765118534 ) ) ;
#22411 = CARTESIAN_POINT ( 'NONE',  ( -8.710071997420207879, 61.11481371789854933, 3.796722387233182339 ) ) ;
#22412 = CARTESIAN_POINT ( 'NONE',  ( 15.00000000000000000, 0.000000000000000000, -9.899999999999991473 ) ) ;
#22413 = ORIENTED_EDGE ( 'NONE', *, *, #30266, .F. ) ;
#22414 = CARTESIAN_POINT ( 'NONE',  ( 21.00000000000000000, 242.2937500012290570, -6.928203230275506996 ) ) ;
#22415 = VECTOR ( 'NONE', #11434, 1000.000000000000000 ) ;
#22416 = CARTESIAN_POINT ( 'NONE',  ( 2.660918448318003282, 68.30231371789855643, 12.46528703574811558 ) ) ;
#22417 = CARTESIAN_POINT ( 'NONE',  ( 16.56230152254411436, -7.209453229046482114, -5.484374999385515537 ) ) ;
#22418 = CARTESIAN_POINT ( 'NONE',  ( 15.24356964375000167, -3.323476615752272600, -6.065624999385484273 ) ) ;
#22419 = CARTESIAN_POINT ( 'NONE',  ( -4.944772684328424539, 35.81481371789854506, -11.48171059495408031 ) ) ;
#22420 = VERTEX_POINT ( 'NONE', #29806 ) ;
#22421 = CARTESIAN_POINT ( 'NONE',  ( 19.68408634441912142, -5.407089921784861808, -2.296874999385551064 ) ) ;
#22422 = LINE ( 'NONE', #4970, #14326 ) ;
#22423 = CARTESIAN_POINT ( 'NONE',  ( -31.19419563604516910, 203.5000000000000000, 0.1155267958017914542 ) ) ;
#22424 = CARTESIAN_POINT ( 'NONE',  ( -47.81919563604517265, 216.5000000000000000, -0.1155267958017906493 ) ) ;
#22425 = CARTESIAN_POINT ( 'NONE',  ( 27.00000000000001776, -11.99999999999999822, 49.73803434254939759 ) ) ;
#22426 = FILL_AREA_STYLE_COLOUR ( '', #14719 ) ;
#22427 = CARTESIAN_POINT ( 'NONE',  ( 24.00000000000000000, -5.196152422706629359, -7.500000000000007105 ) ) ;
#22428 = CARTESIAN_POINT ( 'NONE',  ( 12.50000000000000355, 75.48981371789855643, -0.1745138560722771515 ) ) ;
#22429 = EDGE_CURVE ( 'NONE', #37490, #26027, #29407, .T. ) ;
#22430 = CARTESIAN_POINT ( 'NONE',  ( -40.10788769728823411, 214.4690446883608104, 1.321298161741840893 ) ) ;
#22431 = CARTESIAN_POINT ( 'NONE',  ( -50.20163769728823411, 215.6869285224996986, -3.149950860017881382 ) ) ;
#22432 = DIRECTION ( 'NONE',  ( 0.000000000000000000, 0.000000000000000000, 1.000000000000000000 ) ) ;
#22433 = CARTESIAN_POINT ( 'NONE',  ( -14.08244204927778576, 215.9517727336253756, -5.357269300704888160 ) ) ;
#22434 = CARTESIAN_POINT ( 'NONE',  ( -0.1745138560722442889, 45.58981371789855785, -15.50000000000000533 ) ) ;
#22435 = CARTESIAN_POINT ( 'NONE',  ( -67.22247103062156270, 205.6499508600178956, 7.303452534266880569 ) ) ;
#22437 = CARTESIAN_POINT ( 'NONE',  ( -4.622313124798576922, 23.63518628210144357, -11.61527771782819762 ) ) ;
#22436 = AXIS2_PLACEMENT_3D ( 'NONE', #2175, #13376, #13757 ) ;
#22438 = CARTESIAN_POINT ( 'NONE',  ( -2.660918448318275509, 75.09768628210143504, 12.46528703574805874 ) ) ;
#22439 = CARTESIAN_POINT ( 'NONE',  ( 14.38691631536207538, 16.73518628210143788, -5.770363421893813793 ) ) ;
#22440 = CARTESIAN_POINT ( 'NONE',  ( 10.56230152254410548, 3.464101615137757051, -2.287500000000039613 ) ) ;
#22441 = CARTESIAN_POINT ( 'NONE',  ( 20.99999999999999645, 0.000000000000000000, -8.000000000000000000 ) ) ;
#22442 = EDGE_LOOP ( 'NONE', ( #22084, #28993, #32882, #24652 ) ) ;
#22443 = CARTESIAN_POINT ( 'NONE',  ( -8.632099005475501130, 23.34768628210144570, -13.23911966647218996 ) ) ;
#22444 = CARTESIAN_POINT ( 'NONE',  ( 13.62178482187501416, 196.3531250006145115, 23.59362340125806767 ) ) ;
#22445 = CARTESIAN_POINT ( 'NONE',  ( -27.24356964374999990, 198.4718750006145171, -15.72908226750537786 ) ) ;
#22446 = CARTESIAN_POINT ( 'NONE',  ( 52.59268362704444399, 124.7349959275252615, 2.500000000000000000 ) ) ;
#22447 = LINE ( 'NONE', #19246, #32327 ) ;
#22448 = DIRECTION ( 'NONE',  ( -0.000000000000000000, 1.000000000000000000, -0.000000000000000000 ) ) ;
#22449 = CARTESIAN_POINT ( 'NONE',  ( 19.39230484541326760, 247.8424038105676459, 5.999999999999999112 ) ) ;
#22450 = CARTESIAN_POINT ( 'NONE',  ( 23.87821517812500005, 247.7593750006145399, 4.985214923628404016 ) ) ;
#22451 = CARTESIAN_POINT ( 'NONE',  ( -3.474262827703527901, 115.1648137178985678, 8.843639120294245259 ) ) ;
#22452 = CARTESIAN_POINT ( 'NONE',  ( 18.12178482187500350, 242.2843750006145456, 4.985214923628407568 ) ) ;
#22453 = VERTEX_POINT ( 'NONE', #26962 ) ;
#22454 = CARTESIAN_POINT ( 'NONE',  ( -67.22247103062156270, 206.6499508600178672, 5.571401726697986057 ) ) ;
#22455 = FILL_AREA_STYLE_COLOUR ( '', #28689 ) ;
#22456 = CARTESIAN_POINT ( 'NONE',  ( 26.99999999999999645, 247.5812500012290513, -7.347880794884117764E-16 ) ) ;
#22457 = CARTESIAN_POINT ( 'NONE',  ( -2.660918448318005058, 118.9023137178985507, -12.46528703574811558 ) ) ;
#22458 = CARTESIAN_POINT ( 'NONE',  ( 19.68408634441910721, -5.407089921784855591, -8.090624999385564564 ) ) ;
#22459 = CARTESIAN_POINT ( 'NONE',  ( 24.63505227327785363, 3.604726614523236616, 163.1857653286025709 ) ) ;
#22460 = CARTESIAN_POINT ( 'NONE',  ( 26.75643035624999655, 7.049594010296217766E-16, -0.9281249993854934210 ) ) ;
#22461 = CARTESIAN_POINT ( 'NONE',  ( 26.99999999999999645, 195.7625000000000171, -15.58845726811990495 ) ) ;
#22462 = ORIENTED_EDGE ( 'NONE', *, *, #15902, .T. ) ;
#22463 = EDGE_LOOP ( 'NONE', ( #25819, #15371, #25985, #6271 ) ) ;
#22464 = ORIENTED_EDGE ( 'NONE', *, *, #28651, .T. ) ;
#22465 = CARTESIAN_POINT ( 'NONE',  ( 18.00000000000000355, -5.196152422706632912, -5.718749998770950249 ) ) ;
#22466 = CARTESIAN_POINT ( 'NONE',  ( 20.99999999999999645, 6.646953231504538984, -1.603124999385460159 ) ) ;
#22467 = CARTESIAN_POINT ( 'NONE',  ( 13.56230152254411792, -5.196152422706638241, -4.425000000000068212 ) ) ;
#22468 = CYLINDRICAL_SURFACE ( 'NONE', #28695, 5.999999999999999112 ) ;
#22469 = CARTESIAN_POINT ( 'NONE',  ( 21.00000000000000000, 248.0593750006145228, 6.646953231504538984 ) ) ;
#22470 = CARTESIAN_POINT ( 'NONE',  ( -4.944772684328673229, 56.98518628210144499, 11.48171059495397728 ) ) ;
#22471 = EDGE_CURVE ( 'NONE', #33186, #25843, #4914, .T. ) ;
#22472 = CARTESIAN_POINT ( 'NONE',  ( -60.68377896937849414, 208.3738570449995109, 6.530955311639247363 ) ) ;
#22473 = CARTESIAN_POINT ( 'NONE',  ( 14.34881165084055965, 216.6511883491515675, -0.6450403596498489600 ) ) ;
#22474 =( BOUNDED_CURVE ( )  B_SPLINE_CURVE ( 2, ( #25609, #37166, #17092, #17653, #34327, #5508, #28631 ),
 .UNSPECIFIED., .F., .F. ) 
 B_SPLINE_CURVE_WITH_KNOTS ( ( 3, 2, 2, 3 ),
 ( 0.8043478260869593166, 0.8115942028985527745, 0.8188405797101460104, 0.8260869565217394683 ),
 .UNSPECIFIED. ) 
 CURVE ( )  GEOMETRIC_REPRESENTATION_ITEM ( )  RATIONAL_B_SPLINE_CURVE ( ( 0.9999999999999487077, 0.8660254037844899999, 1.000000000000000000, 0.8660254037844387076, 1.000000000000000000, 0.8660254037844326014, 1.000000000000006217 ) ) 
 REPRESENTATION_ITEM ( '' )  );
#22475 = CARTESIAN_POINT ( 'NONE',  ( -46.82961230271182984, 211.3212981617417938, 4.469044688360757966 ) ) ;
#22476 = ADVANCED_FACE ( 'NONE', ( #25008 ), #21301, .F. ) ;
#22477 = FILL_AREA_STYLE ('',( #10902 ) ) ;
#22478 = CARTESIAN_POINT ( 'NONE',  ( 34.07795076420737246, -5.196152422706629359, 165.0605215108271864 ) ) ;
#22479 = CARTESIAN_POINT ( 'NONE',  ( 4.944772684328420986, 114.0148137178985621, 11.48171059495408208 ) ) ;
#22480 = CARTESIAN_POINT ( 'NONE',  ( -38.52455436395488420, 205.1570982666397356, 4.673758765035198159 ) ) ;
#22482 = EDGE_CURVE ( 'NONE', #10335, #35545, #10796, .T. ) ;
#22481 = CARTESIAN_POINT ( 'NONE',  ( -50.79538769728824121, 212.3930949314662371, -8.469044688360781947 ) ) ;
#22483 = CONTEXT_DEPENDENT_SHAPE_REPRESENTATION ( #17799, #11048 ) ;
#22484 = VECTOR ( 'NONE', #9961, 1000.000000000000000 ) ;
#22485 = CARTESIAN_POINT ( 'NONE',  ( 20.99999999999999645, -6.646953231504538984, -1.490624999385500749 ) ) ;
#22486 = CARTESIAN_POINT ( 'NONE',  ( -27.24356964374999990, 195.7156250006145513, -15.72908226750537786 ) ) ;
#22487 = CARTESIAN_POINT ( 'NONE',  ( 14.25334919248795451, 102.5148137178985621, -6.092822981423661410 ) ) ;
#22488 = CARTESIAN_POINT ( 'NONE',  ( -66.62127896937849414, 218.5309553116392465, 2.162041339862725842 ) ) ;
#22489 = ORIENTED_EDGE ( 'NONE', *, *, #27094, .F. ) ;
#22490 = CARTESIAN_POINT ( 'NONE',  ( 12.53471296425194836, 118.2226862821014635, -2.311890736173178418 ) ) ;
#22491 = CARTESIAN_POINT ( 'NONE',  ( -14.38691631536207183, 58.13518628210145067, 5.770363421893814682 ) ) ;
#22492 = CARTESIAN_POINT ( 'NONE',  ( 22.56230152254411792, 7.347880794884125653E-16, -0.6750000000000366818 ) ) ;
#22493 = CARTESIAN_POINT ( 'NONE',  ( 24.55824627498148160, -3.604726614523244610, 162.3078687509092788 ) ) ;
#22494 = CARTESIAN_POINT ( 'NONE',  ( 14.25334919248782661, 82.28518628210146346, 6.092822981423971385 ) ) ;
#22495 = CARTESIAN_POINT ( 'NONE',  ( -45.84747103062156981, 213.3500491399821328, -5.571401726697985168 ) ) ;
#22496 = CARTESIAN_POINT ( 'NONE',  ( 10.31873187879411091, -3.604726614523240613, -5.953124999385525307 ) ) ;
#22497 = CARTESIAN_POINT ( 'NONE',  ( 8.843639120294328748, 16.73518628210143788, -3.474262827703334722 ) ) ;
#22498 = CARTESIAN_POINT ( 'NONE',  ( 33.68574992184294103, -5.196152422706629359, 160.5776453694143129 ) ) ;
#22499 = CARTESIAN_POINT ( 'NONE',  ( -67.22247103062156270, 206.6499508600178672, 5.571401726697986057 ) ) ;
#22500 = CARTESIAN_POINT ( 'NONE',  ( 19.39230484541326760, 249.1924038105676686, 5.999999999999998224 ) ) ;
#22501 = CARTESIAN_POINT ( 'NONE',  ( -11.61527771782819940, 58.13518628210144357, 4.622313124798574258 ) ) ;
#22502 = CARTESIAN_POINT ( 'NONE',  ( 13.50000000000001421, 198.8000000000000114, 23.38268590217984055 ) ) ;
#22503 = DIRECTION ( 'NONE',  ( -0.000000000000000000, -0.000000000000000000, 1.000000000000000000 ) ) ;
#22505 = CARTESIAN_POINT ( 'NONE',  ( 22.80587116629411426, 3.604726614523243278, -2.184374999385525040 ) ) ;
#22504 = CARTESIAN_POINT ( 'NONE',  ( 1.715153634034233487, 28.52268628210144286, 9.534712964251941258 ) ) ;
#22506 = CARTESIAN_POINT ( 'NONE',  ( 23.87821517812500005, 249.5593750006145228, 4.985214923628404016 ) ) ;
#22507 = EDGE_LOOP ( 'NONE', ( #27698, #21905, #34465, #1330 ) ) ;
#22508 = CARTESIAN_POINT ( 'NONE',  ( 18.00000000000000355, -5.196152422706632912, -1.274999999999998357 ) ) ;
#22509 = CARTESIAN_POINT ( 'NONE',  ( 26.71249821599011653, 0.8257047527043690494, -7.999999999999998224 ) ) ;
#22510 = CARTESIAN_POINT ( 'NONE',  ( 33.79318086914889818, 5.407089921784862696, 160.4082625921878673 ) ) ;
#22511 = CARTESIAN_POINT ( 'NONE',  ( 10.31873187879411091, -3.604726614523240613, -2.353124999385527882 ) ) ;
#22512 = CARTESIAN_POINT ( 'NONE',  ( 28.26462387754589045, -5.407089921784859143, 168.8534947411257576 ) ) ;
#22513 = CARTESIAN_POINT ( 'NONE',  ( 15.00000000000000000, 243.6999999999999886, 0.000000000000000000 ) ) ;
#22514 = CARTESIAN_POINT ( 'NONE',  ( 16.56230152254410726, 0.000000000000000000, -10.00000000000000000 ) ) ;
#22515 = CARTESIAN_POINT ( 'NONE',  ( -10.69584247140444866, 94.64768628210146062, 6.932735513423972762 ) ) ;
#22516 = ORIENTED_EDGE ( 'NONE', *, *, #17525, .T. ) ;
#22517 = VERTEX_POINT ( 'NONE', #10605 ) ;
#22518 = VECTOR ( 'NONE', #15691, 1000.000000000000000 ) ;
#22519 = CARTESIAN_POINT ( 'NONE',  ( 26.99999999999999645, 195.8750000012290400, -15.58845726811990495 ) ) ;
#22520 = CARTESIAN_POINT ( 'NONE',  ( 37.22014685496823461, 7.347880794884125653E-16, 166.5548474367465985 ) ) ;
#22521 = CARTESIAN_POINT ( 'NONE',  ( 14.38691631536194393, 48.46481371789856496, 5.770363421894124656 ) ) ;
#22522 = CARTESIAN_POINT ( 'NONE',  ( 15.24356964374999990, 3.323476615752268604, -9.290624999385480365 ) ) ;
#22523 = CARTESIAN_POINT ( 'NONE',  ( 26.75643035624999655, 242.8843750006145115, -7.049594010296217766E-16 ) ) ;
#22524 = CARTESIAN_POINT ( 'NONE',  ( -37.73288769728823411, 205.5309553116392465, -1.321298161741839117 ) ) ;
#22525 = CARTESIAN_POINT ( 'NONE',  ( 15.02283181144952628, 7.347880794884122694E-16, 50.52293445648592751 ) ) ;
#22526 = CARTESIAN_POINT ( 'NONE',  ( -5.529263428287297444, 35.52731371789855075, -7.954856959092311719 ) ) ;
#22527 = CARTESIAN_POINT ( 'NONE',  ( -69.59747103062156270, 213.3500491399821328, -5.571401726697985168 ) ) ;
#22528 = CARTESIAN_POINT ( 'NONE',  ( -9.534712964251895073, 89.57731371789856212, -1.715153634034446428 ) ) ;
#22529 = CARTESIAN_POINT ( 'NONE',  ( -27.24356964374999990, 198.0218750006145569, -15.72908226750537786 ) ) ;
#22530 = CARTESIAN_POINT ( 'NONE',  ( -14.25334919248795096, 143.9148137178985678, 6.092822981423662299 ) ) ;
#22531 = AXIS2_PLACEMENT_3D ( 'NONE', #36742, #14004, #18959 ) ;
#22532 = CARTESIAN_POINT ( 'NONE',  ( -7.228626920339069173, 66.47268628210144925, 10.49813415415989581 ) ) ;
#22533 = CARTESIAN_POINT ( 'NONE',  ( 38.04237167757703020, 114.1383727779938511, 7.500000000000000000 ) ) ;
#22534 = CARTESIAN_POINT ( 'NONE',  ( 20.99999999999999645, 185.0294372515228645, 5.999999999999999112 ) ) ;
#22535 = CARTESIAN_POINT ( 'NONE',  ( 36.94067227134398479, 7.646167579472015790E-16, 160.5657900808910767 ) ) ;
#22536 = CARTESIAN_POINT ( 'NONE',  ( 15.47811703177229070, 6.148715791637015649, -10.19635138606057367 ) ) ;
#22537 = CARTESIAN_POINT ( 'NONE',  ( 13.44051670066911086, 5.407089921784862696, -5.671874999385540406 ) ) ;
#22538 = CARTESIAN_POINT ( 'NONE',  ( 10.56230152254410903, 0.000000000000000000, -0.4500000000000614619 ) ) ;
#22539 = CARTESIAN_POINT ( 'NONE',  ( 20.99999999999998579, 247.2437500012290457, -5.999999999999997335 ) ) ;
#22540 = CARTESIAN_POINT ( 'NONE',  ( -9.534712964251941258, 67.62268628210145494, 1.715153634034234154 ) ) ;
#22541 = CARTESIAN_POINT ( 'NONE',  ( 3.253724281355069334E-15, 199.5500000012290513, -27.00000000000000355 ) ) ;
#22542 = CARTESIAN_POINT ( 'NONE',  ( -11.61527771782819940, 113.3351862821014606, 4.622313124798574258 ) ) ;
#22543 = CARTESIAN_POINT ( 'NONE',  ( 15.00000000000000000, 0.000000000000000000, -0.8437499987709595750 ) ) ;
#22544 = ORIENTED_EDGE ( 'NONE', *, *, #17498, .F. ) ;
#22545 = CARTESIAN_POINT ( 'NONE',  ( 37.09755260828975310, 7.646167579472015790E-16, 162.3589405374562205 ) ) ;
#22546 = CARTESIAN_POINT ( 'NONE',  ( 26.75643035624999655, -3.323476615752267715, -4.903124999385481964 ) ) ;
#22547 = CARTESIAN_POINT ( 'NONE',  ( -13.62178482187498396, 197.2343750006145626, 23.59362340125808188 ) ) ;
#22548 = CARTESIAN_POINT ( 'NONE',  ( 34.45992230116843302, 5.407089921784862696, 168.0291520325897636 ) ) ;
#22549 = CARTESIAN_POINT ( 'NONE',  ( 31.17434351900397971, 6.928203230275514990, 166.2932785684852490 ) ) ;
#22550 = FACE_OUTER_BOUND ( 'NONE', #24959, .T. ) ;
#22551 = CARTESIAN_POINT ( 'NONE',  ( 18.00000000000000000, 249.9250000000000114, -5.196152422706630247 ) ) ;
#22552 = CARTESIAN_POINT ( 'NONE',  ( -27.24356964375000345, 199.8031250006145285, 0.000000000000000000 ) ) ;
#22553 = EDGE_CURVE ( 'NONE', #32257, #15602, #24111, .T. ) ;
#22554 = CARTESIAN_POINT ( 'NONE',  ( -2.064181346179062349, 8.502313717898553946, -9.465287035748106703 ) ) ;
#22555 = CARTESIAN_POINT ( 'NONE',  ( -2.660918448318275509, 139.4976862821014549, 12.46528703574805874 ) ) ;
#22557 = VERTEX_POINT ( 'NONE', #35677 ) ;
#22556 = ORIENTED_EDGE ( 'NONE', *, *, #29268, .F. ) ;
#22558 = CARTESIAN_POINT ( 'NONE',  ( 18.12178482187499640, 243.8218750006145399, -4.985214923628404904 ) ) ;
#22559 = CARTESIAN_POINT ( 'NONE',  ( -11.61527771782809282, 16.26481371789853370, -4.622313124798832717 ) ) ;
#22560 = CARTESIAN_POINT ( 'NONE',  ( 23.87821517812500005, -4.985214923628404016, -4.490624999385461891 ) ) ;
#22561 = CARTESIAN_POINT ( 'NONE',  ( 3.257655550456945548, 114.3023137178985422, 15.46528703574811736 ) ) ;
#22562 = DIRECTION ( 'NONE',  ( 2.057406622567553763E-16, -0.000000000000000000, -1.000000000000000000 ) ) ;
#22563 = CARTESIAN_POINT ( 'NONE',  ( 26.75643035624999655, 7.049594010296217766E-16, -2.278124999385483740 ) ) ;
#22564 = CARTESIAN_POINT ( 'NONE',  ( 10.31873187879411091, -3.604726614523244610, -7.359374999385524418 ) ) ;
#22565 = PRODUCT_DEFINITION_SHAPE ( 'NONE', 'NONE',  #29920 ) ;
#22566 = CARTESIAN_POINT ( 'NONE',  ( 27.24356964374999635, 195.1156250006145001, -15.72908226750539029 ) ) ;
#22567 = CARTESIAN_POINT ( 'NONE',  ( 12.46528703574805874, 118.7976862821014663, 2.660918448318279950 ) ) ;
#22568 = CARTESIAN_POINT ( 'NONE',  ( 19.68408634441910721, -5.407089921784855591, -2.240624999385543159 ) ) ;
#22569 =( BOUNDED_CURVE ( )  B_SPLINE_CURVE ( 2, ( #17691, #35106, #29230, #37380, #34921, #11803, #46 ),
 .UNSPECIFIED., .F., .F. ) 
 B_SPLINE_CURVE_WITH_KNOTS ( ( 3, 2, 2, 3 ),
 ( 0.2173913043478257756, 0.2246376811594198997, 0.2318840579710139960, 0.2391304347826081200 ),
 .UNSPECIFIED. ) 
 CURVE ( )  GEOMETRIC_REPRESENTATION_ITEM ( )  RATIONAL_B_SPLINE_CURVE ( ( 1.000000000000005773, 0.8660254037844331565, 1.000000000000000000, 0.8660254037844387076, 1.000000000000000000, 0.8660254037844494768, 0.9999999999999892308 ) ) 
 REPRESENTATION_ITEM ( '' )  );
#22570 = EDGE_CURVE ( 'NONE', #20178, #32003, #30712, .T. ) ;
#22571 = CARTESIAN_POINT ( 'NONE',  ( -47.02752896937850835, 214.3500491399821897, 7.303452534266821949 ) ) ;
#22572 = CARTESIAN_POINT ( 'NONE',  ( 20.99999999999999645, 244.6843750006145513, -6.646953231504538984 ) ) ;
#22573 = CARTESIAN_POINT ( 'NONE',  ( 16.56230152254411436, -6.928203230275506996, -7.424999998770979381 ) ) ;
#22574 = CARTESIAN_POINT ( 'NONE',  ( -38.71502896937850124, 213.8393509191290889, -2.350049139982142155 ) ) ;
#22575 = CARTESIAN_POINT ( 'NONE',  ( 10.49813415415989581, 128.5726862821014720, 7.228626920339068285 ) ) ;
#22576 = CARTESIAN_POINT ( 'NONE',  ( 19.56230152254410370, 5.196152422706631135, -4.537499998771011178 ) ) ;
#22577 = EDGE_CURVE ( 'NONE', #18882, #21667, #30447, .T. ) ;
#22578 = CARTESIAN_POINT ( 'NONE',  ( -48.61830436395490551, 209.8844732041982581, 6.500000000000000888 ) ) ;
#22579 = CARTESIAN_POINT ( 'NONE',  ( 21.00000000000000355, 0.000000000000000000, 50.00000000000001421 ) ) ;
#22580 = CARTESIAN_POINT ( 'NONE',  ( 1.255007937094097924E-14, 199.4375000000000284, -27.00000000000000000 ) ) ;
#22581 = CARTESIAN_POINT ( 'NONE',  ( 8.927990412390657937, 98.67268628210146630, -13.04141134922759804 ) ) ;
#22582 = CARTESIAN_POINT ( 'NONE',  ( 4.622313124798573369, 19.03518628210144925, 11.61527771782819940 ) ) ;
#22583 = CARTESIAN_POINT ( 'NONE',  ( -77.00000000000002842, 210.0000000000000000, 2.500000000000001332 ) ) ;
#22584 = CARTESIAN_POINT ( 'NONE',  ( -2.064181346179269738, 130.2976862821014379, 9.465287035748067623 ) ) ;
#22585 = AXIS2_PLACEMENT_3D ( 'NONE', #10405, #33525, #7567 ) ;
#22586 = CARTESIAN_POINT ( 'NONE',  ( 16.56230152254411436, -7.209453229046475009, -0.4781249993855187230 ) ) ;
#22587 =( BOUNDED_CURVE ( )  B_SPLINE_CURVE ( 2, ( #14051, #25601, #34319, #188, #14416, #3032, #11754 ),
 .UNSPECIFIED., .F., .F. ) 
 B_SPLINE_CURVE_WITH_KNOTS ( ( 3, 2, 2, 3 ),
 ( 0.6086956521739120829, 0.6159420289855060959, 0.6231884057971003310, 0.6304347826086944551 ),
 .UNSPECIFIED. ) 
 CURVE ( )  GEOMETRIC_REPRESENTATION_ITEM ( )  RATIONAL_B_SPLINE_CURVE ( ( 1.000000000000018430, 0.8660254037844202779, 1.000000000000000000, 0.8660254037844387076, 1.000000000000000000, 0.8660254037844612451, 0.9999999999999774625 ) ) 
 REPRESENTATION_ITEM ( '' )  );
#22588 = DIRECTION ( 'NONE',  ( 1.000000000000000000, 0.000000000000000000, 0.000000000000000000 ) ) ;
#22589 = ORIENTED_EDGE ( 'NONE', *, *, #11217, .F. ) ;
#22590 = DIRECTION ( 'NONE',  ( 0.000000000000000000, 0.000000000000000000, 1.000000000000000000 ) ) ;
#22591 = CARTESIAN_POINT ( 'NONE',  ( 3.796722387233379514, 70.78518628210143504, -8.710071997420127943 ) ) ;
#22592 = CARTESIAN_POINT ( 'NONE',  ( 19.56230152254410370, 5.196152422706631135, -2.287499998770980980 ) ) ;
#22593 = CARTESIAN_POINT ( 'NONE',  ( 5.778771075727756162E-15, 195.8656250006145285, 31.45816453501075927 ) ) ;
#22594 = CARTESIAN_POINT ( 'NONE',  ( 20.99999999999997513, 246.7937500012290286, -5.999999999999999112 ) ) ;
#22595 = CARTESIAN_POINT ( 'NONE',  ( -13.62178482187498396, 195.4343750006145228, 23.59362340125808188 ) ) ;
#22596 = CARTESIAN_POINT ( 'NONE',  ( 18.00000000000000000, 249.9250000000000114, -5.196152422706630247 ) ) ;
#22597 = CARTESIAN_POINT ( 'NONE',  ( 5.438367727407757144E-14, 198.5374999999999943, -27.00000000000000000 ) ) ;
#22598 = CARTESIAN_POINT ( 'NONE',  ( -2.064181346179062349, 63.70231371789854791, -9.465287035748106703 ) ) ;
#22599 = CARTESIAN_POINT ( 'NONE',  ( 15.00000000000000000, 3.464101615137752166, -9.937500000000000000 ) ) ;
#22600 = ORIENTED_EDGE ( 'NONE', *, *, #28607, .T. ) ;
#22601 = MECHANICAL_DESIGN_GEOMETRIC_PRESENTATION_REPRESENTATION (  '', ( #6872 ), #32865 ) ;
#22602 = CARTESIAN_POINT ( 'NONE',  ( 21.00000000000000000, 242.5187500012290513, 6.928203230275506996 ) ) ;
#22603 = CARTESIAN_POINT ( 'NONE',  ( -11.61527771782809282, 62.26481371789854791, -4.622313124798832717 ) ) ;
#22604 = CARTESIAN_POINT ( 'NONE',  ( 16.56230152254411081, 7.209453229046482114, -5.709374999385496530 ) ) ;
#22605 = CARTESIAN_POINT ( 'NONE',  ( 21.00000000000000000, 6.646953231504538984, -6.215624999385504168 ) ) ;
#22606 = CARTESIAN_POINT ( 'NONE',  ( -11.48171059495408208, 24.31481371789855217, 4.944772684328421875 ) ) ;
#22607 = EDGE_LOOP ( 'NONE', ( #13869, #2606 ) ) ;
#22608 = CARTESIAN_POINT ( 'NONE',  ( 19.68408634441911076, 5.407089921784862696, -1.246874999385527705 ) ) ;
#22609 = DIRECTION ( 'NONE',  ( 1.000000000000000000, 6.123233995736766036E-17, -0.000000000000000000 ) ) ;
#22610 = ADVANCED_FACE ( 'NONE', ( #16307 ), #33733, .F. ) ;
#22611 = CARTESIAN_POINT ( 'NONE',  ( 22.56230152254595112, 3.464101615136682355, -9.524999998771026100 ) ) ;
#22612 = CARTESIAN_POINT ( 'NONE',  ( -45.84002896937850124, 204.4285982733020433, 3.350049139982171020 ) ) ;
#22613 = CARTESIAN_POINT ( 'NONE',  ( 25.41288579386105440, 0.000000000000000000, 169.2817949039725818 ) ) ;
#22614 = ADVANCED_FACE ( 'NONE', ( #32837 ), #6882, .T. ) ;
#22616 = B_SPLINE_CURVE_WITH_KNOTS ( 'NONE', 3,
 ( #27370, #33810, #13158, #30220, #7662, #22070, #25085, #36640, #24713, #18861, #35894, #4245, #30409, #24533, #4804, #4432, #16013, #1590, #21880, #33621, #19239, #30781, #16384, #27928 ),
 .UNSPECIFIED., .F., .F.,
 ( 4, 2, 2, 2, 2, 2, 2, 2, 2, 2, 2, 4 ),
 ( 0.000000000000000000, 0.001571281823982130250, 0.002356922735973196025, 0.003142563647964261367, 0.004713845471946314855, 0.005499486383937341599, 0.006285127295928367476, 0.007856409119910477343, 0.009427690943892588077, 0.01021333185588364431, 0.01099897276787470055, 0.01257025459185682689 ),
 .UNSPECIFIED. ) ;
#22615 = PLANE ( 'NONE',  #8501 ) ;
#22617 = CARTESIAN_POINT ( 'NONE',  ( -35.15997103062156270, 213.8393509191290889, 2.350049139982164359 ) ) ;
#22618 = CARTESIAN_POINT ( 'NONE',  ( -41.09747103062156981, 213.3500491399821328, -5.571401726697985168 ) ) ;
#22619 = VERTEX_POINT ( 'NONE', #33917 ) ;
#22620 = CARTESIAN_POINT ( 'NONE',  ( -27.00000000000000355, 197.8625000012290513, 0.000000000000000000 ) ) ;
#22621 = CARTESIAN_POINT ( 'NONE',  ( -4.694659320240884604E-14, 197.5250000012290172, 27.00000000000000000 ) ) ;
#22622 = CARTESIAN_POINT ( 'NONE',  ( 2.908627838312458636, 36.67731371789854933, -15.53471296425188442 ) ) ;
#22623 = CARTESIAN_POINT ( 'NONE',  ( -32.57961230271184405, 212.3930949314663792, 8.469044688360751749 ) ) ;
#22624 = CARTESIAN_POINT ( 'NONE',  ( 10.49813415415989581, 8.972686282101431487, 7.228626920339068285 ) ) ;
#22625 = CARTESIAN_POINT ( 'NONE',  ( 12.53471296425194836, 53.82268628210144357, -2.311890736173178418 ) ) ;
#22626 = VECTOR ( 'NONE', #18871, 1000.000000000000000 ) ;
#22627 = CARTESIAN_POINT ( 'NONE',  ( 15.53471296425195369, 17.02268628210144996, -2.908627838312120684 ) ) ;
#22629 = EDGE_CURVE ( 'NONE', #21, #4681, #12411, .T. ) ;
#22628 = CARTESIAN_POINT ( 'NONE',  ( 16.56230152254411436, -6.928203230275514990, -1.687500000000023981 ) ) ;
#22630 = VERTEX_POINT ( 'NONE', #27672 ) ;
#22631 = CARTESIAN_POINT ( 'NONE',  ( -12.53471296425194836, 141.2226862821014493, 2.311890736173176641 ) ) ;
#22632 = DIRECTION ( 'NONE',  ( -0.000000000000000000, 1.000000000000000000, -0.000000000000000000 ) ) ;
#22633 = CARTESIAN_POINT ( 'NONE',  ( -1.926257025242585782E-15, 197.9468750006145399, -31.45816453501075927 ) ) ;
#22634 = CARTESIAN_POINT ( 'NONE',  ( 10.56230152254410726, 0.000000000000000000, -6.637499998771001941 ) ) ;
#22635 = SURFACE_SIDE_STYLE ('',( #28120 ) ) ;
#22636 = FACE_BOUND ( 'NONE', #8885, .T. ) ;
#22637 = CARTESIAN_POINT ( 'NONE',  ( 8.715434833791931624, 9.260186282101429356, 8.962234695871760692 ) ) ;
#22638 = CARTESIAN_POINT ( 'NONE',  ( 18.12178482187500350, 248.1343750006145399, 4.985214923628407568 ) ) ;
#22639 = CARTESIAN_POINT ( 'NONE',  ( 5.233372021372610483, 120.0523137178985280, -8.152565276336593669 ) ) ;
#22640 = CARTESIAN_POINT ( 'NONE',  ( 20.99999999999999645, 242.0968750006145456, -6.646953231504538984 ) ) ;
#22641 = EDGE_LOOP ( 'NONE', ( #24968, #951, #36925, #32638 ) ) ;
#22642 = DIRECTION ( 'NONE',  ( 0.1219804832088915436, 0.9925324990730154395, 0.000000000000000000 ) ) ;
#22643 = DIRECTION ( 'NONE',  ( -0.000000000000000000, 1.000000000000000000, -0.000000000000000000 ) ) ;
#22644 = CARTESIAN_POINT ( 'NONE',  ( 18.00000000000000355, 248.3312500012290513, 5.196152422706632912 ) ) ;
#22645 = EDGE_CURVE ( 'NONE', #10703, #205, #27975, .T. ) ;
#22646 = CARTESIAN_POINT ( 'NONE',  ( 8.715434833792128799, 120.3398137178985650, -8.962234695871567070 ) ) ;
#22647 = CARTESIAN_POINT ( 'NONE',  ( 14.39393254099747743, 5.957544813848095089, -10.12707777273552523 ) ) ;
#22648 = CARTESIAN_POINT ( 'NONE',  ( 30.78949644248743311, -7.209453229046475009, 161.8944563553360467 ) ) ;
#22649 = CARTESIAN_POINT ( 'NONE',  ( 20.99999999999995026, 240.9437500012290911, -5.999999999999998224 ) ) ;
#22650 = CARTESIAN_POINT ( 'NONE',  ( -26.99999999999998934, 195.0875000000000341, 15.58845726811991561 ) ) ;
#22651 = ORIENTED_EDGE ( 'NONE', *, *, #790, .T. ) ;
#22652 = VERTEX_POINT ( 'NONE', #29999 ) ;
#22653 = VERTEX_POINT ( 'NONE', #4546 ) ;
#22654 = CARTESIAN_POINT ( 'NONE',  ( 26.99999999999999645, 3.464101615137755275, -4.631249998770964993 ) ) ;
#22656 = VECTOR ( 'NONE', #8094, 1000.000000000000000 ) ;
#22655 = CARTESIAN_POINT ( 'NONE',  ( 26.75643035624999655, 3.323476615752271268, -2.578124999385477345 ) ) ;
#22657 = CARTESIAN_POINT ( 'NONE',  ( 20.99999999999999645, 6.928203230275506996, -6.412499999999995204 ) ) ;
#22659 = CARTESIAN_POINT ( 'NONE',  ( 37.25609859885201303, -3.464101615137556767, 166.9657777497094173 ) ) ;
#22658 = PRODUCT_DEFINITION_FORMATION_WITH_SPECIFIED_SOURCE ( 'ANY', '', #16821, .NOT_KNOWN. ) ;
#22660 = CARTESIAN_POINT ( 'NONE',  ( 21.00000000000000000, 249.1843750006144944, -6.646953231504538984 ) ) ;
#22661 = CARTESIAN_POINT ( 'NONE',  ( -12.50000000000000355, 58.71018628210145351, -0.1745138560725492671 ) ) ;
#22662 = AXIS2_PLACEMENT_3D ( 'NONE', #13942, #5210, #36858 ) ;
#22663 = VECTOR ( 'NONE', #5205, 1000.000000000000000 ) ;
#22664 = CARTESIAN_POINT ( 'NONE',  ( -58.50669563604516554, 209.8844732041982013, -6.500000000000000888 ) ) ;
#22665 = CARTESIAN_POINT ( 'NONE',  ( 14.43174379454687362, 216.5682562054521725, 0.6968546016497486617 ) ) ;
#22666 = CARTESIAN_POINT ( 'NONE',  ( -36.34002896937849414, 206.1606490808709111, 2.350049139982143931 ) ) ;
#22667 = CARTESIAN_POINT ( 'NONE',  ( 36.91945954259593776, 3.464101615137755275, 163.1179757295544164 ) ) ;
#22668 = CARTESIAN_POINT ( 'NONE',  ( 10.69584247140429589, 113.1523137178985650, 6.932735513424201024 ) ) ;
#22669 = CARTESIAN_POINT ( 'NONE',  ( -31.99330436395490196, 210.1155267958017134, -6.500000000000000888 ) ) ;
#22670 = CARTESIAN_POINT ( 'NONE',  ( -46.44122103062156981, 207.8379586601371329, -8.530955311639223382 ) ) ;
#22671 = CARTESIAN_POINT ( 'NONE',  ( 23.87821517812500005, -4.985214923628404016, -5.503124999385489602 ) ) ;
#22672 = CARTESIAN_POINT ( 'NONE',  ( 27.24356964375000700, 195.0406250006145399, 15.72908226750537075 ) ) ;
#22673 = CARTESIAN_POINT ( 'NONE',  ( 3.257655550456945548, 95.90231371789855075, 15.46528703574811736 ) ) ;
#22674 = CARTESIAN_POINT ( 'NONE',  ( -33.37127896937850124, 216.5309553116391612, 1.626142955000506873 ) ) ;
#22675 = ORIENTED_EDGE ( 'NONE', *, *, #24434, .T. ) ;
#22676 =( BOUNDED_CURVE ( )  B_SPLINE_CURVE ( 2, ( #6777, #12466, #9436, #2994, #8872, #17787, #6020 ),
 .UNSPECIFIED., .F., .F. ) 
 B_SPLINE_CURVE_WITH_KNOTS ( ( 3, 2, 2, 3 ),
 ( 0.8695652173913032135, 0.8768115942028972265, 0.8840579710144913506, 0.8913043478260852526 ),
 .UNSPECIFIED. ) 
 CURVE ( )  GEOMETRIC_REPRESENTATION_ITEM ( )  RATIONAL_B_SPLINE_CURVE ( ( 1.000000000000020428, 0.8660254037844181685, 1.000000000000000000, 0.8660254037844387076, 1.000000000000000000, 0.8660254037844694608, 0.9999999999999692468 ) ) 
 REPRESENTATION_ITEM ( '' )  );
#22677 = CARTESIAN_POINT ( 'NONE',  ( 23.99999999999999645, 249.0062500012290627, -5.196152422706631135 ) ) ;
#22678 = CARTESIAN_POINT ( 'NONE',  ( -2.311890736173176641, 115.9226862821014521, -12.53471296425194836 ) ) ;
#22679 = CARTESIAN_POINT ( 'NONE',  ( -14.25334919248782306, 68.48518628210145209, -6.092822981423979378 ) ) ;
#22680 = CARTESIAN_POINT ( 'NONE',  ( 16.56230152254411792, -6.928203230275514990, -0.7875000000000323963 ) ) ;
#22681 = CARTESIAN_POINT ( 'NONE',  ( 27.77600699476686330, 5.407089921784862696, 163.2685782149489171 ) ) ;
#22682 = PRESENTATION_LAYER_ASSIGNMENT (  '', '', ( #23270 ) ) ;
#22683 = CARTESIAN_POINT ( 'NONE',  ( -10.83675517735155047, 78.26018628210144357, -11.08355503943142750 ) ) ;
#22684 = EDGE_CURVE ( 'NONE', #21723, #23273, #28043, .T. ) ;
#22685 = CARTESIAN_POINT ( 'NONE',  ( 10.31873187879411269, 3.604726614523236616, -6.028124999385552130 ) ) ;
#22686 = CARTESIAN_POINT ( 'NONE',  ( -5.529263428287477744, 20.47268628210143859, 7.954856959092191815 ) ) ;
#22687 = DIRECTION ( 'NONE',  ( -0.000000000000000000, 1.000000000000000000, -0.000000000000000000 ) ) ;
#22688 = CARTESIAN_POINT ( 'NONE',  ( -67.42038769728823411, 208.1428034533959703, 6.469044688360770401 ) ) ;
#22689 = CARTESIAN_POINT ( 'NONE',  ( 18.00000000000000000, 243.2312500012290570, -5.196152422706630247 ) ) ;
#22690 = CARTESIAN_POINT ( 'NONE',  ( -12.46528703574805697, 58.99768628210144783, -2.660918448318280838 ) ) ;
#22691 = CARTESIAN_POINT ( 'NONE',  ( 27.00000000000001066, 197.9375000000000284, 15.58845726811988897 ) ) ;
#22692 = CARTESIAN_POINT ( 'NONE',  ( 13.49999999999999645, 197.7125000012290172, -23.38268590217984766 ) ) ;
#22694 = CARTESIAN_POINT ( 'NONE',  ( 22.80587116629411781, -3.604726614523238837, -2.709374999385515181 ) ) ;
#22693 = CARTESIAN_POINT ( 'NONE',  ( 3.796722387233379514, 24.78518628210144215, -8.710071997420127943 ) ) ;
#22695 = CARTESIAN_POINT ( 'NONE',  ( 26.75643035624999655, 249.6718750006145342, -3.323476615752271268 ) ) ;
#22696 = ORIENTED_EDGE ( 'NONE', *, *, #6911, .T. ) ;
#22697 = CARTESIAN_POINT ( 'NONE',  ( 26.99999999999999645, 7.347880794884117764E-16, -5.175000000000013145 ) ) ;
#22698 = CARTESIAN_POINT ( 'NONE',  ( 10.49999999999999467, 210.0000000000000000, 0.000000000000000000 ) ) ;
#22699 = ADVANCED_FACE ( 'NONE', ( #33545 ), #7959, .F. ) ;
#22700 = CARTESIAN_POINT ( 'NONE',  ( 33.83240095338533848, 5.407089921784862696, 160.8565502063291603 ) ) ;
#22701 = CARTESIAN_POINT ( 'NONE',  ( 16.56230152254411081, -7.209453229046475009, -2.728124999385529215 ) ) ;
#22702 = CARTESIAN_POINT ( 'NONE',  ( 34.46482481169798717, 5.407089921784857367, 168.0851879843573897 ) ) ;
#22703 = CARTESIAN_POINT ( 'NONE',  ( 18.00000000000000000, 244.0749999999999886, -5.196152422706630247 ) ) ;
#22704 = CARTESIAN_POINT ( 'NONE',  ( -13.49999999999998401, 198.7250000000000227, 23.38268590217985476 ) ) ;
#22705 = EDGE_CURVE ( 'NONE', #35917, #20737, #31840, .T. ) ;
#22706 =( BOUNDED_CURVE ( )  B_SPLINE_CURVE ( 2, ( #28325, #16964, #9126, #576, #17664, #13754, #20692, #9315, #29200 ),
 .UNSPECIFIED., .F., .F. ) 
 B_SPLINE_CURVE_WITH_KNOTS ( ( 3, 2, 2, 2, 3 ),
 ( 0.1847826086956521618, 0.1884057971014492794, 0.1956521739130434867, 0.2028985507246376940, 0.2065217391304347838 ),
 .UNSPECIFIED. ) 
 CURVE ( )  GEOMETRIC_REPRESENTATION_ITEM ( )  RATIONAL_B_SPLINE_CURVE ( ( 0.9330127018922194093, 0.9330127018922190762, 1.000000000000000000, 0.8660254037844387076, 1.000000000000000000, 0.8660254037844387076, 1.000000000000000000, 0.9330127018922194093, 0.9330127018922194093 ) ) 
 REPRESENTATION_ITEM ( '' )  );
#22707 = CARTESIAN_POINT ( 'NONE',  ( 4.622313124798573369, 65.03518628210144925, 11.61527771782819940 ) ) ;
#22708 = VERTEX_POINT ( 'NONE', #33320 ) ;
#22709 = ORIENTED_EDGE ( 'NONE', *, *, #11948, .F. ) ;
#22710 = CARTESIAN_POINT ( 'NONE',  ( 5.727106289114498080E-15, 194.8250000012290570, 31.17691453623979214 ) ) ;
#22711 = CARTESIAN_POINT ( 'NONE',  ( 36.72009078106068358, 7.347880794884117764E-16, 160.8391803576695622 ) ) ;
#22712 = CARTESIAN_POINT ( 'NONE',  ( 10.83675517735179206, 37.53981371789855359, -11.08355503943118769 ) ) ;
#22713 = CARTESIAN_POINT ( 'NONE',  ( 21.00000000000000000, -6.646953231504538984, -8.690624999385464733 ) ) ;
#22714 = CARTESIAN_POINT ( 'NONE',  ( 15.24356964375000167, 241.7968750006145342, 3.323476615752272600 ) ) ;
#22715 = CARTESIAN_POINT ( 'NONE',  ( -46.44122103062156981, 208.9097554298617752, -4.530955311639240257 ) ) ;
#22716 = CARTESIAN_POINT ( 'NONE',  ( 20.99999999999999645, 6.928203230275506996, -7.312499999999986677 ) ) ;
#22717 = CARTESIAN_POINT ( 'NONE',  ( 30.74537384772143866, -7.209453229046482114, 161.3901327894271276 ) ) ;
#22718 = CARTESIAN_POINT ( 'NONE',  ( 3.474262827703532341, 36.96481371789853654, -8.843639120294245259 ) ) ;
#22719 = LINE ( 'NONE', #25915, #9925 ) ;
#22720 = CARTESIAN_POINT ( 'NONE',  ( 3.796722387233182339, 86.41481371789855359, 8.710071997420207879 ) ) ;
#22721 = CARTESIAN_POINT ( 'NONE',  ( 13.62178482187499640, 197.4593750006145285, -23.59362340125807123 ) ) ;
#22722 = CARTESIAN_POINT ( 'NONE',  ( 8.927990412390371944, 141.3273137178985621, 13.04141134922778811 ) ) ;
#22723 = CARTESIAN_POINT ( 'NONE',  ( -0.1745138560725500443, 65.61018628210145209, 12.50000000000000355 ) ) ;
#22724 = DIRECTION ( 'NONE',  ( 0.000000000000000000, 0.000000000000000000, 1.000000000000000000 ) ) ;
#22725 = CARTESIAN_POINT ( 'NONE',  ( 24.36378002397578868, 0.000000000000000000, 160.0851093307920223 ) ) ;
#22726 = CARTESIAN_POINT ( 'NONE',  ( 23.99999999999999645, 5.196152422706631135, -0.5437499987709648597 ) ) ;
#22727 = CARTESIAN_POINT ( 'NONE',  ( 22.80587116629411781, -3.604726614523238837, -9.459374999385547156 ) ) ;
#22728 = FILL_AREA_STYLE ('',( #28392 ) ) ;
#22729 = CARTESIAN_POINT ( 'NONE',  ( 6.594114490232313663, 82.86018628210146630, 6.840914352312096547 ) ) ;
#22730 = PLANE ( 'NONE',  #3138 ) ;
#22731 = CARTESIAN_POINT ( 'NONE',  ( 8.715434833791931624, 119.6601862821014493, 8.962234695871760692 ) ) ;
#22732 = CARTESIAN_POINT ( 'NONE',  ( 15.65448942698881574, 195.0065153083762652, -22.13879085154164628 ) ) ;
#22733 = CARTESIAN_POINT ( 'NONE',  ( 20.99999999999999645, 185.0294372515228645, -5.999999999999999112 ) ) ;
#22734 = ORIENTED_EDGE ( 'NONE', *, *, #7408, .F. ) ;
#22735 = CARTESIAN_POINT ( 'NONE',  ( 30.80910648460564971, 7.209453229046475009, 162.1186001624066932 ) ) ;
#22736 = CARTESIAN_POINT ( 'NONE',  ( 15.24356964374999990, 3.323476615752268604, -6.928124999385478766 ) ) ;
#22737 = CARTESIAN_POINT ( 'NONE',  ( -1.926257025242585782E-15, 196.1468750006145569, -31.45816453501076637 ) ) ;
#22738 = CARTESIAN_POINT ( 'NONE',  ( 37.44236251553516581, -3.604726614523238837, 166.3001358117817006 ) ) ;
#22739 = CARTESIAN_POINT ( 'NONE',  ( 28.28054129496681313, -5.196152422706638241, 167.6381075309029711 ) ) ;
#22740 = CARTESIAN_POINT ( 'NONE',  ( -7.234628195640289583, 198.1075961894323143, -27.00000000000001421 ) ) ;
#22741 = CARTESIAN_POINT ( 'NONE',  ( 15.24356964374999990, 241.3093750006145228, 0.000000000000000000 ) ) ;
#22742 = CARTESIAN_POINT ( 'NONE',  ( -13.62178482187498396, 199.4281250006145569, 23.59362340125808188 ) ) ;
#22743 = AXIS2_PLACEMENT_3D ( 'NONE', #4505, #16082, #1661 ) ;
#22744 = CARTESIAN_POINT ( 'NONE',  ( 10.49813415416005213, 129.8273137178985905, -7.228626920338837358 ) ) ;
#22745 = CARTESIAN_POINT ( 'NONE',  ( 27.24356964374999279, 195.6218750006145228, -15.72908226750539207 ) ) ;
#22747 = ORIENTED_EDGE ( 'NONE', *, *, #35157, .F. ) ;
#22746 = VERTEX_POINT ( 'NONE', #15895 ) ;
#22748 = CARTESIAN_POINT ( 'NONE',  ( 18.12178482187500350, 241.2718750006145001, 4.985214923628407568 ) ) ;
#22749 = CARTESIAN_POINT ( 'NONE',  ( 2.660918448318003282, 13.10231371789855004, 12.46528703574811558 ) ) ;
#22750 = CARTESIAN_POINT ( 'NONE',  ( 14.25334919248795451, 102.5148137178985621, -6.092822981423661410 ) ) ;
#22751 = CARTESIAN_POINT ( 'NONE',  ( -11.61527771782819940, 104.1351862821014578, 4.622313124798574258 ) ) ;
#22752 = CARTESIAN_POINT ( 'NONE',  ( 26.75643035624999655, 3.323476615752271712, -2.240624999385472549 ) ) ;
#22753 = CARTESIAN_POINT ( 'NONE',  ( -27.00000000000000355, 198.3125000012290400, 0.000000000000000000 ) ) ;
#22754 = CARTESIAN_POINT ( 'NONE',  ( 2.311890736173175753, 120.5226862821014606, 12.53471296425194836 ) ) ;
#22755 = CARTESIAN_POINT ( 'NONE',  ( 22.80587116629410360, -3.604726614523235284, -4.003124999385554439 ) ) ;
#22756 = CARTESIAN_POINT ( 'NONE',  ( -45.24627896937850835, 201.4690446883607251, -2.162041339862721845 ) ) ;
#22757 = CARTESIAN_POINT ( 'NONE',  ( 26.75643035624999655, 243.2218750006145171, -7.049594010296217766E-16 ) ) ;
#22758 = CARTESIAN_POINT ( 'NONE',  ( 2.999999999999997335, 244.5000000000000000, 5.000000000000000000 ) ) ;
#22759 = CARTESIAN_POINT ( 'NONE',  ( -62.66294563604517975, 214.6737587650350747, -4.842901733360249317 ) ) ;
#22760 = CARTESIAN_POINT ( 'NONE',  ( -2.311890736173176641, 125.1226862821014549, -12.53471296425194836 ) ) ;
#22761 = CARTESIAN_POINT ( 'NONE',  ( 13.56230152254411259, -5.196152422706632912, -2.512499998771011711 ) ) ;
#22762 = CIRCLE ( 'NONE', #3379, 1.000000000000002220 ) ;
#22763 = CARTESIAN_POINT ( 'NONE',  ( -49.01413769728823411, 213.1499508600178672, 5.686928522499718142 ) ) ;
#22764 = FACE_OUTER_BOUND ( 'NONE', #32756, .T. ) ;
#22765 = CARTESIAN_POINT ( 'NONE',  ( 25.45210587809749825, 0.000000000000000000, 169.7300825181138748 ) ) ;
#22766 = CARTESIAN_POINT ( 'NONE',  ( -2.908627838312119351, 97.52268628210144641, -15.53471296425195369 ) ) ;
#22767 = CARTESIAN_POINT ( 'NONE',  ( -2.660918448318275509, 10.69768628210143646, 12.46528703574805874 ) ) ;
#22768 = CARTESIAN_POINT ( 'NONE',  ( -70.80918835584510873, 215.2843023367891249, -7.500000000000000000 ) ) ;
#22769 = CARTESIAN_POINT ( 'NONE',  ( -8.710071997420127943, 123.6851862821014549, -3.796722387233380402 ) ) ;
#22770 = CARTESIAN_POINT ( 'NONE',  ( 10.31873187879411091, -3.604726614523240613, -1.903124999385531924 ) ) ;
#22771 = CARTESIAN_POINT ( 'NONE',  ( 22.56230152254563492, 3.464101615136866652, -9.074999998770993059 ) ) ;
#22772 = ORIENTED_EDGE ( 'NONE', *, *, #10071, .F. ) ;
#22773 = CYLINDRICAL_SURFACE ( 'NONE', #20352, 27.00000000000000355 ) ;
#22774 = CARTESIAN_POINT ( 'NONE',  ( 5.529263428287477744, 61.87268628210144783, -7.954856959092191815 ) ) ;
#22775 = CARTESIAN_POINT ( 'NONE',  ( 18.12178482187499640, 4.985214923628404904, -0.2156249993854608693 ) ) ;
#22776 = CARTESIAN_POINT ( 'NONE',  ( 20.99999999999995026, 241.3375000000000341, -5.999999999999998224 ) ) ;
#22777 = CARTESIAN_POINT ( 'NONE',  ( 10.56230152254410903, 7.347880794884117764E-16, -10.00000000000000000 ) ) ;
#22778 = CARTESIAN_POINT ( 'NONE',  ( -27.24356964375000345, 196.7093750006145569, 0.000000000000000000 ) ) ;
#22779 = CARTESIAN_POINT ( 'NONE',  ( 6.753460448932012028, 195.0000000000000284, 26.40771703998824549 ) ) ;
#22780 = CARTESIAN_POINT ( 'NONE',  ( -7.234628195640328663, 197.0549038117967484, 26.99999999999999289 ) ) ;
#22781 = CARTESIAN_POINT ( 'NONE',  ( 0.1745138560723095977, 40.98981371789854933, 9.500000000000005329 ) ) ;
#22782 = CARTESIAN_POINT ( 'NONE',  ( 21.00000000000000000, 6.928203230275506996, -8.662499999999972999 ) ) ;
#22783 = EDGE_LOOP ( 'NONE', ( #17197, #5035, #13980, #11033 ) ) ;
#22784 = CARTESIAN_POINT ( 'NONE',  ( 26.99999999999999645, 240.8312500012290513, -7.347880794884117764E-16 ) ) ;
#22785 = CARTESIAN_POINT ( 'NONE',  ( -8.715434833792127023, 69.73981371789855643, 8.962234695871568846 ) ) ;
#22786 = CARTESIAN_POINT ( 'NONE',  ( 19.68408634441911786, -5.407089921784861808, -8.596874999385523353 ) ) ;
#22787 = CARTESIAN_POINT ( 'NONE',  ( 18.12178482187500350, -4.985214923628407568, -10.07812499938548534 ) ) ;
#22788 = CARTESIAN_POINT ( 'NONE',  ( 11.61527771782809637, 20.86481371789854222, 4.622313124798827388 ) ) ;
#22789 = CIRCLE ( 'NONE', #33061, 7.500000000000000000 ) ;
#22790 = ORIENTED_EDGE ( 'NONE', *, *, #29328, .T. ) ;
#22791 = CARTESIAN_POINT ( 'NONE',  ( 13.44051670066911086, 5.407089921784862696, -0.7218749993855300140 ) ) ;
#22792 = CARTESIAN_POINT ( 'NONE',  ( 4.944772684328679446, 6.385186282101440014, -11.48171059495397373 ) ) ;
#22793 = CARTESIAN_POINT ( 'NONE',  ( 31.11796464796764994, 7.209453229046482114, 165.6488651237693261 ) ) ;
#22794 = CARTESIAN_POINT ( 'NONE',  ( -39.50669563604517265, 209.8844732041982013, -6.500000000000000888 ) ) ;
#22795 = CARTESIAN_POINT ( 'NONE',  ( 13.56230152254410726, 5.196152422706630247, -0.4124999987710209481 ) ) ;
#22796 = AXIS2_PLACEMENT_3D ( 'NONE', #6005, #17587, #29119 ) ;
#22797 = CARTESIAN_POINT ( 'NONE',  ( 16.56230152254411436, 6.928203230275514990, -2.812500000000029310 ) ) ;
#22798 = CARTESIAN_POINT ( 'NONE',  ( -68.00669563604516554, 209.8844732041982297, -4.499999999999996447 ) ) ;
#22800 = ADVANCED_FACE ( 'NONE', ( #22326 ), #27999, .T. ) ;
#22799 = CARTESIAN_POINT ( 'NONE',  ( -50.00372103062157692, 216.5309553116391612, -1.626142955000564383 ) ) ;
#22801 = CARTESIAN_POINT ( 'NONE',  ( -20.86978606573367045, 194.8588513912095266, -17.51182790300216752 ) ) ;
#22802 = VERTEX_POINT ( 'NONE', #13798 ) ;
#22803 = CARTESIAN_POINT ( 'NONE',  ( -27.00000000000000355, 196.8125000000000000, -15.58845726811989429 ) ) ;
#22804 = DIRECTION ( 'NONE',  ( 1.000000000000000000, 0.000000000000000000, 0.000000000000000000 ) ) ;
#22805 = CARTESIAN_POINT ( 'NONE',  ( -15.53471296425188442, 15.97731371789853405, -2.908627838312459080 ) ) ;
#22806 = CARTESIAN_POINT ( 'NONE',  ( -33.56919563604517265, 218.5000000000000000, -0.1155267958018185298 ) ) ;
#22807 = CARTESIAN_POINT ( 'NONE',  ( 12.50000000000000355, 17.31018628210144428, 0.1745138560725507937 ) ) ;
#22808 = CARTESIAN_POINT ( 'NONE',  ( -12.50000000000000355, 40.31018628210144783, -0.1745138560725492671 ) ) ;
#22810 = EDGE_CURVE ( 'NONE', #6605, #22453, #12255, .T. ) ;
#22809 = CARTESIAN_POINT ( 'NONE',  ( 10.56230152254411436, -3.464101615137761048, -4.012500000000060574 ) ) ;
#22811 = CARTESIAN_POINT ( 'NONE',  ( 0.000000000000000000, 0.000000000000000000, -5.000000000000000000 ) ) ;
#22812 = VERTEX_POINT ( 'NONE', #2216 ) ;
#22813 = CARTESIAN_POINT ( 'NONE',  ( -5.770363421893818234, 14.43518628210144072, -14.38691631536207005 ) ) ;
#22814 = CARTESIAN_POINT ( 'NONE',  ( 13.62178482187501416, 195.0031250006145456, 23.59362340125806767 ) ) ;
#22815 = CARTESIAN_POINT ( 'NONE',  ( 27.24356964375000345, 197.3843750006145399, -3.336375036156643733E-15 ) ) ;
#22816 = CARTESIAN_POINT ( 'NONE',  ( 16.56230152254411081, 6.928203230275514990, -6.412500000000027178 ) ) ;
#22817 = CARTESIAN_POINT ( 'NONE',  ( -27.00000000000000355, 198.6500000000000341, 0.000000000000000000 ) ) ;
#22818 = CARTESIAN_POINT ( 'NONE',  ( 20.99999999999999645, 6.928203230275506996, -5.456249998770962506 ) ) ;
#22819 = CARTESIAN_POINT ( 'NONE',  ( 23.99999999999999645, 246.3062500012290457, -5.196152422706631135 ) ) ;
#22820 = CARTESIAN_POINT ( 'NONE',  ( 26.75643035624999655, 244.2718750006145001, -3.323476615752271712 ) ) ;
#22821 = CARTESIAN_POINT ( 'NONE',  ( 3.474262827703532341, 101.3648137178985706, -8.843639120294245259 ) ) ;
#22822 = CARTESIAN_POINT ( 'NONE',  ( 26.75643035624999655, 241.5343750006145456, -7.049594010296217766E-16 ) ) ;
#22823 = ORIENTED_EDGE ( 'NONE', *, *, #33667, .T. ) ;
#22824 = CARTESIAN_POINT ( 'NONE',  ( 0.000000000000000000, 148.0000000000000000, 7.500000000000000000 ) ) ;
#22825 = CARTESIAN_POINT ( 'NONE',  ( 1.120210788295102201E-13, 195.8375000000000057, -27.00000000000000711 ) ) ;
#22826 = VECTOR ( 'NONE', #22609, 1000.000000000000000 ) ;
#22827 = EDGE_CURVE ( 'NONE', #5728, #6033, #7547, .T. ) ;
#22828 = CARTESIAN_POINT ( 'NONE',  ( 21.00000000000000000, 247.6937500012290343, -6.928203230275506996 ) ) ;
#22829 = VERTEX_POINT ( 'NONE', #7176 ) ;
#22830 = CARTESIAN_POINT ( 'NONE',  ( -11.48171059495408208, 116.3148137178985593, 4.944772684328421875 ) ) ;
#22831 = CARTESIAN_POINT ( 'NONE',  ( 13.44051670066911086, 5.407089921784862696, -0.7218749993855300140 ) ) ;
#22832 = CARTESIAN_POINT ( 'NONE',  ( 36.93740393099094632, -3.604726614523235284, 160.5284327797126025 ) ) ;
#22833 = CARTESIAN_POINT ( 'NONE',  ( 26.75643035624999655, 7.049594010296217766E-16, -0.4781249993854874702 ) ) ;
#22834 = CARTESIAN_POINT ( 'NONE',  ( -27.00000000000000355, 195.0263594417697846, -9.827195513778322677 ) ) ;
#22835 = ORIENTED_EDGE ( 'NONE', *, *, #17058, .F. ) ;
#22836 = VERTEX_POINT ( 'NONE', #16269 ) ;
#22837 = ORIENTED_EDGE ( 'NONE', *, *, #1304, .F. ) ;
#22838 = CARTESIAN_POINT ( 'NONE',  ( 23.99999999999999645, 5.196152422706631135, -6.843749998770965348 ) ) ;
#22839 = CARTESIAN_POINT ( 'NONE',  ( 15.24356964375000167, -3.323476615752272600, -3.703124999385450700 ) ) ;
#22840 = ADVANCED_BREP_SHAPE_REPRESENTATION ( '', ( #7452, #17215 ), #33555 ) ;
#22841 = CARTESIAN_POINT ( 'NONE',  ( 30.59584727662355164, 6.928203230275506996, 159.6810362611256267 ) ) ;
#22842 = DIRECTION ( 'NONE',  ( -0.000000000000000000, 1.000000000000000000, -0.000000000000000000 ) ) ;
#22843 = CARTESIAN_POINT ( 'NONE',  ( 18.12178482187499640, 248.7718750006145001, -4.985214923628404904 ) ) ;
#22844 = CARTESIAN_POINT ( 'NONE',  ( -10.49813415415989581, 59.57268628210145778, -7.228626920339068285 ) ) ;
#22845 = CARTESIAN_POINT ( 'NONE',  ( -65.03794563604516554, 205.3262412349648116, 4.842901733360249317 ) ) ;
#22846 = CARTESIAN_POINT ( 'NONE',  ( 5.840947329779441866, 215.6846447513326268, 1.929602858956334099 ) ) ;
#22847 = CARTESIAN_POINT ( 'NONE',  ( -44.05877896937850124, 211.0902445701383101, -4.530955311639234040 ) ) ;
#22848 =( BOUNDED_CURVE ( )  B_SPLINE_CURVE ( 2, ( #12511, #15544, #29748, #3970, #24630, #24075, #18207, #24264, #9666 ),
 .UNSPECIFIED., .F., .F. ) 
 B_SPLINE_CURVE_WITH_KNOTS ( ( 3, 2, 2, 2, 3 ),
 ( 0.1041666666666666713, 0.1111111111111111049, 0.1250000000000000000, 0.1388888888888888951, 0.1458333333333333426 ),
 .UNSPECIFIED. ) 
 CURVE ( )  GEOMETRIC_REPRESENTATION_ITEM ( )  RATIONAL_B_SPLINE_CURVE ( ( 0.9330127018922194093, 0.9330127018922194093, 1.000000000000000000, 0.8660254037844387076, 1.000000000000000000, 0.8660254037844387076, 1.000000000000000000, 0.9330127018922194093, 0.9330127018922194093 ) ) 
 REPRESENTATION_ITEM ( '' )  );
#22849 = CARTESIAN_POINT ( 'NONE',  ( 33.92107042726159705, -5.196152422706629359, 163.2673710542620427 ) ) ;
#22850 = CARTESIAN_POINT ( 'NONE',  ( -10.49813415416004858, 97.62731371789855928, 7.228626920338839135 ) ) ;
#22851 = CARTESIAN_POINT ( 'NONE',  ( -33.18080436395490551, 203.5000000000000000, -0.1155267958017335561 ) ) ;
#22852 = CARTESIAN_POINT ( 'NONE',  ( -44.26413769728823411, 214.1499508600179240, 7.418979330068584233 ) ) ;
#22853 = CARTESIAN_POINT ( 'NONE',  ( 23.87821517812499650, 4.985214923628404904, -3.553124999385481875 ) ) ;
#22854 = CARTESIAN_POINT ( 'NONE',  ( 22.56230152254410370, 7.347880794884117764E-16, -4.162499998770996967 ) ) ;
#22855 = CARTESIAN_POINT ( 'NONE',  ( -11.08355503943118592, 72.03981371789855359, -10.83675517735179383 ) ) ;
#22856 = CARTESIAN_POINT ( 'NONE',  ( -38.12127896937848703, 216.5309553116391612, 1.626142955000506873 ) ) ;
#22857 = ADVANCED_FACE ( 'NONE', ( #19494 ), #30669, .T. ) ;
#22858 = ORIENTED_EDGE ( 'NONE', *, *, #12839, .T. ) ;
#22859 = CARTESIAN_POINT ( 'NONE',  ( -80.75120197997713944, 224.5663476446710831, -7.500000000000000000 ) ) ;
#22860 = CARTESIAN_POINT ( 'NONE',  ( 2.311890736173175753, 102.1226862821014691, 12.53471296425194836 ) ) ;
#22861 = CARTESIAN_POINT ( 'NONE',  ( 2.908627838312118019, 65.32268628210144357, 15.53471296425195369 ) ) ;
#22862 = CARTESIAN_POINT ( 'NONE',  ( 25.01527935017339033, 0.000000000000000000, 50.00000000000000000 ) ) ;
#22863 = CARTESIAN_POINT ( 'NONE',  ( 37.01747826964035681, 3.604726614523243278, 161.4436866585844541 ) ) ;
#22864 = CARTESIAN_POINT ( 'NONE',  ( 14.38691631536207538, 71.93518628210142651, -5.770363421893813793 ) ) ;
#22865 = CARTESIAN_POINT ( 'NONE',  ( 10.31873187879411091, 3.604726614523236616, -6.478124999385515004 ) ) ;
#22866 = CARTESIAN_POINT ( 'NONE',  ( -74.35000000000002274, 210.0000000000000000, -5.000000000000001776 ) ) ;
#22867 = CARTESIAN_POINT ( 'NONE',  ( -56.73288769728823411, 203.5309553116391612, -1.857196546604028775 ) ) ;
#22868 = CARTESIAN_POINT ( 'NONE',  ( 5.999999999999999112, -20.00000000000000000, -19.99999999999999289 ) ) ;
#22869 = CARTESIAN_POINT ( 'NONE',  ( 2.311890736173175753, 37.72268628210144215, 12.53471296425194836 ) ) ;
#22870 = CARTESIAN_POINT ( 'NONE',  ( -13.50000000000000533, 197.2250000000000227, -23.38268590217984411 ) ) ;
#22871 = CARTESIAN_POINT ( 'NONE',  ( -26.99999999999999645, 197.9000000012290457, 15.58845726811991561 ) ) ;
#22872 = CARTESIAN_POINT ( 'NONE',  ( 3.474262827703335166, 28.23518628210144854, 8.843639120294326972 ) ) ;
#22873 = CARTESIAN_POINT ( 'NONE',  ( 18.12178482187499640, 248.4343750006145228, -4.985214923628404904 ) ) ;
#22874 = ORIENTED_EDGE ( 'NONE', *, *, #32055, .T. ) ;
#22875 = CARTESIAN_POINT ( 'NONE',  ( 26.99999999999999645, -3.464101615137751278, -3.862499999999976730 ) ) ;
#22876 = CARTESIAN_POINT ( 'NONE',  ( 37.18092677073180141, 7.347880794884125653E-16, 166.1065598226053055 ) ) ;
#22877 = CARTESIAN_POINT ( 'NONE',  ( 27.65834674205753529, 5.407089921784862696, 161.9237153725250664 ) ) ;
#22878 = CARTESIAN_POINT ( 'NONE',  ( 19.68408634441910365, 5.407089921784857367, -2.990624999385543603 ) ) ;
#22879 = CARTESIAN_POINT ( 'NONE',  ( 34.54326498017087488, 5.407089921784857367, 168.9817632126399758 ) ) ;
#22880 = CARTESIAN_POINT ( 'NONE',  ( 26.99999999999999645, 244.3375000000000341, 3.464101615137751278 ) ) ;
#22881 = DIRECTION ( 'NONE',  ( 0.1219804832088915436, 0.9925324990730154395, 0.000000000000000000 ) ) ;
#22882 = CARTESIAN_POINT ( 'NONE',  ( 8.962234695871762469, 71.36018628210145209, -8.715434833791931624 ) ) ;
#22883 = EDGE_LOOP ( 'NONE', ( #27769, #389, #12480, #13801, #3654, #22147, #11451, #23755, #34799, #8143, #31476, #25294, #20360, #21401, #1522, #4083, #21627, #19123, #21090, #29958, #15560, #29795, #4390, #9027, #8326, #34754, #10786, #30674, #35916, #10597, #10691, #27488, #30169, #3803, #24090, #14105, #34197, #16647, #14195, #10912, #34566, #9526, #5189, #24331, #18445, #7591 ) ) ;
#22884 = VERTEX_POINT ( 'NONE', #21770 ) ;
#22885 = DIRECTION ( 'NONE',  ( 0.5887012860850814322, -0.8083506638593001004, -3.328006943901143992E-31 ) ) ;
#22886 = CARTESIAN_POINT ( 'NONE',  ( -27.00000000000000355, 196.4750000012290343, -15.58845726811989429 ) ) ;
#22887 = CARTESIAN_POINT ( 'NONE',  ( -7.234628195640263826, 196.4200961906613543, -27.00000000000003553 ) ) ;
#22888 = CIRCLE ( 'NONE', #28929, 1.500000000000001332 ) ;
#22889 = CARTESIAN_POINT ( 'NONE',  ( 15.46528703574811736, 47.60231371789853938, -3.257655550456947768 ) ) ;
#22890 = CARTESIAN_POINT ( 'NONE',  ( 18.12178482187500350, -4.985214923628407568, -9.178124999385472549 ) ) ;
#22891 = ADVANCED_FACE ( 'NONE', ( #13046 ), #30291, .F. ) ;
#22892 = CARTESIAN_POINT ( 'NONE',  ( 21.00000000000000000, 243.2218750006145456, 6.646953231504538984 ) ) ;
#22893 = AXIS2_PLACEMENT_3D ( 'NONE', #2485, #10, #20498 ) ;
#22894 = CARTESIAN_POINT ( 'NONE',  ( -50.20163769728823411, 213.9548777149308592, -2.149950860017830756 ) ) ;
#22895 = CARTESIAN_POINT ( 'NONE',  ( 18.00000000000000355, 242.9312500012290457, 5.196152422706632912 ) ) ;
#22896 = CARTESIAN_POINT ( 'NONE',  ( 33.95006120609467359, 5.407089921784862696, 162.2014130487530110 ) ) ;
#22897 = CARTESIAN_POINT ( 'NONE',  ( -9.534712964251895073, 15.97731371789853405, -1.715153634034446428 ) ) ;
#22898 = CARTESIAN_POINT ( 'NONE',  ( 16.56230152254411081, 7.209453229046475009, -9.703124999385543958 ) ) ;
#22899 =( BOUNDED_CURVE ( )  B_SPLINE_CURVE ( 2, ( #24594, #1840, #33683, #19306, #13229, #10745, #22318, #10187, #15888 ),
 .UNSPECIFIED., .F., .F. ) 
 B_SPLINE_CURVE_WITH_KNOTS ( ( 3, 2, 2, 2, 3 ),
 ( 0.7717391304347825942, 0.7753623188405797118, 0.7826086956521739468, 0.7898550724637680709, 0.7934782608695651884 ),
 .UNSPECIFIED. ) 
 CURVE ( )  GEOMETRIC_REPRESENTATION_ITEM ( )  RATIONAL_B_SPLINE_CURVE ( ( 0.9330127018922194093, 0.9330127018922194093, 1.000000000000000000, 0.8660254037844387076, 1.000000000000000000, 0.8660254037844387076, 1.000000000000000000, 0.9330127018922194093, 0.9330127018922194093 ) ) 
 REPRESENTATION_ITEM ( '' )  );
#22900 = LINE ( 'NONE', #5442, #37275 ) ;
#22901 = CARTESIAN_POINT ( 'NONE',  ( -27.24356964374999635, 195.3968750006145569, 15.72908226750539384 ) ) ;
#22902 = CARTESIAN_POINT ( 'NONE',  ( 6.932735513424201024, 18.85231371789855714, -10.69584247140429412 ) ) ;
#22903 = EDGE_CURVE ( 'NONE', #6033, #717, #37219, .T. ) ;
#22904 = EDGE_LOOP ( 'NONE', ( #2725, #16014, #1778, #12239 ) ) ;
#22905 = CARTESIAN_POINT ( 'NONE',  ( 2.660918448318279950, 61.29768628210143788, -12.46528703574805697 ) ) ;
#22906 = CARTESIAN_POINT ( 'NONE',  ( 18.00000000000000000, 240.4749999999999943, -5.196152422706630247 ) ) ;
#22907 = CARTESIAN_POINT ( 'NONE',  ( 26.99999999999999645, 245.2750000000000057, -7.347880794884117764E-16 ) ) ;
#22908 = VECTOR ( 'NONE', #24718, 1000.000000000000227 ) ;
#22909 = CARTESIAN_POINT ( 'NONE',  ( 24.39973176785919406, 3.604726614523236616, 160.4960396437548411 ) ) ;
#22910 = ADVANCED_FACE ( 'NONE', ( #22143, #7920 ), #36522, .F. ) ;
#22911 = CARTESIAN_POINT ( 'NONE',  ( 15.00000000000000000, 3.464101615137752166, -3.581249998770953624 ) ) ;
#22912 = CARTESIAN_POINT ( 'NONE',  ( 22.80587116629412137, 7.646167579472024665E-16, -8.521874999385502747 ) ) ;
#22913 = CARTESIAN_POINT ( 'NONE',  ( 22.56230152254421384, 3.464101615137700207, -0.1875000000000502653 ) ) ;
#22914 = CARTESIAN_POINT ( 'NONE',  ( -9.500000000000005329, 77.11018628210145209, -0.1745138560725176813 ) ) ;
#22915 = CARTESIAN_POINT ( 'NONE',  ( 21.00000000000000355, 0.000000000000000000, 50.00000000000001421 ) ) ;
#22916 =( BOUNDED_CURVE ( )  B_SPLINE_CURVE ( 2, ( #8296, #17012, #2594, #25719, #28739, #2778, #34616 ),
 .UNSPECIFIED., .F., .F. ) 
 B_SPLINE_CURVE_WITH_KNOTS ( ( 3, 2, 2, 3 ),
 ( 0.4347826086956526059, 0.4420289855072469520, 0.4492753623188412426, 0.4565217391304355332 ),
 .UNSPECIFIED. ) 
 CURVE ( )  GEOMETRIC_REPRESENTATION_ITEM ( )  RATIONAL_B_SPLINE_CURVE ( ( 0.9999999999999917843, 0.8660254037844469233, 1.000000000000000000, 0.8660254037844387076, 1.000000000000000000, 0.8660254037844243857, 1.000000000000014433 ) ) 
 REPRESENTATION_ITEM ( '' )  );
#22917 = CARTESIAN_POINT ( 'NONE',  ( -12.46528703574805697, 104.9976862821014691, -2.660918448318280838 ) ) ;
#22918 = CARTESIAN_POINT ( 'NONE',  ( -27.00000000000000355, 197.2624999999999886, -15.58845726811989429 ) ) ;
#22919 = DIRECTION ( 'NONE',  ( 1.000000000000000000, 0.000000000000000000, 0.000000000000000000 ) ) ;
#22920 = EDGE_LOOP ( 'NONE', ( #243, #30344, #25717, #27581 ) ) ;
#22921 = CARTESIAN_POINT ( 'NONE',  ( 30.88754665307854452, 7.209453229046475009, 163.0151753906892793 ) ) ;
#22922 = CARTESIAN_POINT ( 'NONE',  ( 21.00000000000000000, 6.646953231504538984, -7.453124999385469351 ) ) ;
#22923 = CARTESIAN_POINT ( 'NONE',  ( 13.49999999999999645, 196.2500000000000000, -23.38268590217984766 ) ) ;
#22924 = CARTESIAN_POINT ( 'NONE',  ( 31.35328515338631306, 7.209453229046482114, 168.3385908086170843 ) ) ;
#22925 = CARTESIAN_POINT ( 'NONE',  ( 34.10736582727759725, -5.196152422706635576, 165.3967372202087915 ) ) ;
#22926 = CARTESIAN_POINT ( 'NONE',  ( 13.56230152254410726, 5.196152422706636465, -4.125000000000045297 ) ) ;
#22927 = CARTESIAN_POINT ( 'NONE',  ( 18.12178482187500350, 241.3843750006145115, 4.985214923628407568 ) ) ;
#22928 = CARTESIAN_POINT ( 'NONE',  ( -27.24356964375000345, 198.4531250006145342, 0.000000000000000000 ) ) ;
#22929 = CARTESIAN_POINT ( 'NONE',  ( -12.53471296425189152, 126.3773137178985593, -2.311890736173453753 ) ) ;
#22930 = CARTESIAN_POINT ( 'NONE',  ( 4.622313124798573369, 120.2351862821014663, 11.61527771782819940 ) ) ;
#22932 = ORIENTED_EDGE ( 'NONE', *, *, #776, .T. ) ;
#22931 = EDGE_LOOP ( 'NONE', ( #4259, #9494 ) ) ;
#22933 = CARTESIAN_POINT ( 'NONE',  ( -1.926257025242585782E-15, 197.8906250006145342, -31.45816453501075927 ) ) ;
#22934 = CARTESIAN_POINT ( 'NONE',  ( 18.12178482187500350, 241.7218750006145171, 4.985214923628407568 ) ) ;
#22935 = CARTESIAN_POINT ( 'NONE',  ( 13.56230152254411614, -5.196152422706638241, -2.175000000000065548 ) ) ;
#22936 = CARTESIAN_POINT ( 'NONE',  ( 5.770363421894130873, 92.16481371789855359, -14.38691631536193860 ) ) ;
#22937 = CARTESIAN_POINT ( 'NONE',  ( -0.1745138560725500443, 102.4101862821014493, 12.50000000000000355 ) ) ;
#22938 = CARTESIAN_POINT ( 'NONE',  ( 15.24356964374999990, 0.000000000000000000, -1.603124999385474592 ) ) ;
#22939 = CIRCLE ( 'NONE', #19916, 27.00000000000000000 ) ;
#22940 = CARTESIAN_POINT ( 'NONE',  ( -27.00000000000000355, 197.4125000012290343, 0.000000000000000000 ) ) ;
#22941 = CARTESIAN_POINT ( 'NONE',  ( 2.311890736173175753, 111.3226862821014720, 12.53471296425194836 ) ) ;
#22942 = CARTESIAN_POINT ( 'NONE',  ( 22.80587116629411071, -3.604726614523235284, -2.653124999385503280 ) ) ;
#22943 = ADVANCED_FACE ( 'NONE', ( #4316 ), #33878, .T. ) ;
#22944 = CARTESIAN_POINT ( 'NONE',  ( 23.87821517812500005, 244.4968750006145228, 4.985214923628404016 ) ) ;
#22945 = CARTESIAN_POINT ( 'NONE',  ( 26.99999999999999645, 246.7187500012290684, -3.464101615137755275 ) ) ;
#22946 = CARTESIAN_POINT ( 'NONE',  ( 6.932735513423970097, 119.9476862821014578, 10.69584247140445044 ) ) ;
#22947 = CARTESIAN_POINT ( 'NONE',  ( 10.56230152254410903, 0.000000000000000000, -3.937499998770993770 ) ) ;
#22948 = EDGE_CURVE ( 'NONE', #21187, #18882, #24134, .T. ) ;
#22949 = CARTESIAN_POINT ( 'NONE',  ( -49.40997103062156981, 215.5714017266979852, 3.350049139982118618 ) ) ;
#22950 = CARTESIAN_POINT ( 'NONE',  ( 36.79853094953357129, 7.347880794884117764E-16, 161.7357555859521199 ) ) ;
#22951 = CARTESIAN_POINT ( 'NONE',  ( 27.99292734389955939, 5.196152422706636465, 164.3506650272002219 ) ) ;
#22952 = CARTESIAN_POINT ( 'NONE',  ( 15.53471296425195369, 109.0226862821014606, -2.908627838312120684 ) ) ;
#22953 = CARTESIAN_POINT ( 'NONE',  ( 12.46528703574805874, 17.59768628210144215, 2.660918448318279950 ) ) ;
#22954 = CARTESIAN_POINT ( 'NONE',  ( 36.90638618107669799, 7.347880794884125653E-16, 162.9685465236163111 ) ) ;
#22955 = CARTESIAN_POINT ( 'NONE',  ( 27.00000000000001421, 196.7000000012290286, 15.58845726811988897 ) ) ;
#22956 = CARTESIAN_POINT ( 'NONE',  ( 6.840914352312096547, 135.7601862821014720, -6.594114490232313663 ) ) ;
#22957 = CARTESIAN_POINT ( 'NONE',  ( 26.99999999999999645, 245.7437500012290457, 3.464101615137751278 ) ) ;
#22958 = VERTEX_POINT ( 'NONE', #1472 ) ;
#22959 = CARTESIAN_POINT ( 'NONE',  ( 20.99999999999999645, 0.000000000000000000, -8.000000000000000000 ) ) ;
#22960 = CARTESIAN_POINT ( 'NONE',  ( -2.064181346179269738, 56.69768628210144357, 9.465287035748067623 ) ) ;
#22961 = DIRECTION ( 'NONE',  ( 0.000000000000000000, 0.000000000000000000, 1.000000000000000000 ) ) ;
#22962 = CARTESIAN_POINT ( 'NONE',  ( 15.00000000000000000, 0.000000000000000000, -4.950000000000009948 ) ) ;
#22963 = CYLINDRICAL_SURFACE ( 'NONE', #26964, 5.999999999999994671 ) ;
#22964 = CARTESIAN_POINT ( 'NONE',  ( 5.778771075727756162E-15, 195.9218750006145342, 31.45816453501075927 ) ) ;
#22965 = LINE ( 'NONE', #11576, #29534 ) ;
#22966 = CARTESIAN_POINT ( 'NONE',  ( 20.99999999999999645, 185.0294372515228645, 5.999999999999999112 ) ) ;
#22967 = CARTESIAN_POINT ( 'NONE',  ( 6.840914352311949109, 30.63981371789855146, 6.594114490232462877 ) ) ;
#22968 = CARTESIAN_POINT ( 'NONE',  ( -27.24356964374999279, 198.5468750006145342, 15.72908226750539384 ) ) ;
#22969 = ORIENTED_EDGE ( 'NONE', *, *, #2939, .F. ) ;
#22970 = ORIENTED_EDGE ( 'NONE', *, *, #12890, .F. ) ;
#22971 = CARTESIAN_POINT ( 'NONE',  ( 21.00000000000000000, 248.7343750006145342, -6.646953231504538984 ) ) ;
#22972 = CARTESIAN_POINT ( 'NONE',  ( -12.53471296425189152, 52.77731371789855075, -2.311890736173453309 ) ) ;
#22973 = CARTESIAN_POINT ( 'NONE',  ( 22.80587116629412847, -3.604726614523238837, -9.009374999385519445 ) ) ;
#22974 = CARTESIAN_POINT ( 'NONE',  ( 23.87821517812499650, 4.985214923628404904, -9.403124999385475746 ) ) ;
#22975 = CARTESIAN_POINT ( 'NONE',  ( -12.53471296425189152, 15.97731371789853760, -2.311890736173453753 ) ) ;
#22976 = EDGE_LOOP ( 'NONE', ( #8833, #34974 ) ) ;
#22977 = CARTESIAN_POINT ( 'NONE',  ( 13.44051670066911264, -5.407089921784865361, -1.921874999385508875 ) ) ;
#22978 = CARTESIAN_POINT ( 'NONE',  ( 27.24356964374999635, 199.6156250006145285, -15.72908226750539029 ) ) ;
#22979 = CARTESIAN_POINT ( 'NONE',  ( 24.98313052087628350, 3.604726614523240613, 167.1643179041065252 ) ) ;
#22980 = CARTESIAN_POINT ( 'NONE',  ( -37.13169563604516554, 210.1155267958017703, 6.500000000000000888 ) ) ;
#22981 = CARTESIAN_POINT ( 'NONE',  ( 24.70365593725145104, 3.464101615137415102, 161.1752605482510035 ) ) ;
#22982 = CARTESIAN_POINT ( 'NONE',  ( -25.62253007092369117, 194.9999999999999716, 8.926458104496534318 ) ) ;
#22983 = CARTESIAN_POINT ( 'NONE',  ( -55.73586230271182984, 207.8500491399821613, 3.954877714930852495 ) ) ;
#22984 = CARTESIAN_POINT ( 'NONE',  ( -40.30580436395489841, 216.5000000000000000, 0.1155267958017343610 ) ) ;
#22985 = CARTESIAN_POINT ( 'NONE',  ( 28.35571312319377313, 5.196152422706630247, 168.4973254592314618 ) ) ;
#22986 = ORIENTED_EDGE ( 'NONE', *, *, #25649, .T. ) ;
#22987 = CARTESIAN_POINT ( 'NONE',  ( -28.72218192485006227, 203.0733802275103983, 4.011256465603768362 ) ) ;
#22988 = CARTESIAN_POINT ( 'NONE',  ( 20.99999999999999645, -6.928203230275506996, -7.087500000000004796 ) ) ;
#22989 = CARTESIAN_POINT ( 'NONE',  ( -0.1745138560722442889, 27.18981371789855572, -15.50000000000000533 ) ) ;
#22990 = CARTESIAN_POINT ( 'NONE',  ( -36.34002896937849414, 202.6965474657332038, 4.350049139982197666 ) ) ;
#22991 = CARTESIAN_POINT ( 'NONE',  ( 2.311890736173175753, 10.12268628210144428, 12.53471296425194836 ) ) ;
#22992 = CARTESIAN_POINT ( 'NONE',  ( -11.61527771782819940, 39.73518628210144499, 4.622313124798574258 ) ) ;
#22993 = CARTESIAN_POINT ( 'NONE',  ( 10.56230152254410903, 3.464101615137757051, -4.537500000000050271 ) ) ;
#22994 = EDGE_LOOP ( 'NONE', ( #19069, #4747 ) ) ;
#22995 = CARTESIAN_POINT ( 'NONE',  ( -47.00000000000000711, 244.5000000000000000, -5.000000000000000000 ) ) ;
#22996 = CIRCLE ( 'NONE', #33902, 7.500000000000000000 ) ;
#22997 = CARTESIAN_POINT ( 'NONE',  ( -27.24356964374999635, 195.8468750006145171, 15.72908226750539384 ) ) ;
#22998 = CARTESIAN_POINT ( 'NONE',  ( 37.26590362001809353, -3.464101615137614054, 167.0778496544690768 ) ) ;
#22999 = FACE_BOUND ( 'NONE', #26452, .T. ) ;
#23000 = CARTESIAN_POINT ( 'NONE',  ( 7.234628195640309123, 197.6174038105676516, -27.00000000000000711 ) ) ;
#23001 = FACE_OUTER_BOUND ( 'NONE', #30782, .T. ) ;
#23002 = CARTESIAN_POINT ( 'NONE',  ( 18.12178482187499640, 245.7343750006145342, -4.985214923628404904 ) ) ;
#23003 = CARTESIAN_POINT ( 'NONE',  ( 3.796722387233182339, 95.61481371789857064, 8.710071997420207879 ) ) ;
#23004 = CARTESIAN_POINT ( 'NONE',  ( 15.24356964375000167, 240.8968750006145001, 3.323476615752272600 ) ) ;
#23005 = VERTEX_POINT ( 'NONE', #28185 ) ;
#23006 = CARTESIAN_POINT ( 'NONE',  ( -52.97247103062156981, 206.6499508600178672, 5.571401726697986057 ) ) ;
#23007 = DIRECTION ( 'NONE',  ( -0.000000000000000000, -0.000000000000000000, -1.000000000000000000 ) ) ;
#23008 = CARTESIAN_POINT ( 'NONE',  ( 24.00000000000000000, 247.5062500012290627, 5.196152422706629359 ) ) ;
#23009 = VERTEX_POINT ( 'NONE', #13416 ) ;
#23010 = CARTESIAN_POINT ( 'NONE',  ( -7.228626920338836470, 109.1273137178985593, -10.49813415416005213 ) ) ;
#23011 = CARTESIAN_POINT ( 'NONE',  ( 19.68408634441911431, -5.407089921784861808, -0.4968749993855270386 ) ) ;
#23012 = CARTESIAN_POINT ( 'NONE',  ( 30.69144623189632526, 7.209453229046475009, 160.7737373199828426 ) ) ;
#23013 = CARTESIAN_POINT ( 'NONE',  ( 18.12178482187500350, -4.985214923628407568, -1.528124999385482852 ) ) ;
#23014 = CARTESIAN_POINT ( 'NONE',  ( 8.962234695871567070, 58.23981371789854933, 8.715434833792127023 ) ) ;
#23015 = CARTESIAN_POINT ( 'NONE',  ( -1.926257025242585782E-15, 199.7468750006145513, -31.45816453501075927 ) ) ;
#23016 = EDGE_CURVE ( 'NONE', #15181, #5473, #19313, .T. ) ;
#23017 = VERTEX_POINT ( 'NONE', #4876 ) ;
#23018 = VERTEX_POINT ( 'NONE', #30485 ) ;
#23019 = AXIS2_PLACEMENT_3D ( 'NONE', #37014, #27931, #16940 ) ;
#23020 = ORIENTED_EDGE ( 'NONE', *, *, #25391, .T. ) ;
#23021 = CARTESIAN_POINT ( 'NONE',  ( 21.00000000000000000, 6.928203230275506996, -6.356249998770953979 ) ) ;
#23022 = CARTESIAN_POINT ( 'NONE',  ( 23.87821517812499650, 4.985214923628404904, -3.890624999385472460 ) ) ;
#23023 = DIRECTION ( 'NONE',  ( -0.000000000000000000, -1.000000000000000000, -0.000000000000000000 ) ) ;
#23024 = CARTESIAN_POINT ( 'NONE',  ( 18.12178482187499640, 245.6218750006145228, -4.985214923628404904 ) ) ;
#23025 = CARTESIAN_POINT ( 'NONE',  ( -6.932735513423968321, 50.94768628210144357, -10.69584247140445221 ) ) ;
#23026 = CARTESIAN_POINT ( 'NONE',  ( -54.54836230271182984, 204.3130714775002446, -3.149950860017828091 ) ) ;
#23027 = CARTESIAN_POINT ( 'NONE',  ( 21.00000000000003553, 209.9999999999999716, -5.999999999999996447 ) ) ;
#23028 = CARTESIAN_POINT ( 'NONE',  ( -36.73586230271183695, 207.8500491399821613, 3.954877714930852495 ) ) ;
#23029 = FILL_AREA_STYLE ('',( #37411 ) ) ;
#23030 = VECTOR ( 'NONE', #8017, 1000.000000000000114 ) ;
#23031 = CARTESIAN_POINT ( 'NONE',  ( 24.78209610572492494, 3.464101615137752166, 162.0718357765335611 ) ) ;
#23032 = CARTESIAN_POINT ( 'NONE',  ( 2.660918448318002838, 105.1023137178985536, 12.46528703574811558 ) ) ;
#23033 = CARTESIAN_POINT ( 'NONE',  ( -63.85788769728821990, 214.4690446883608104, 1.321298161741840893 ) ) ;
#23034 = CARTESIAN_POINT ( 'NONE',  ( -42.08705436395490551, 203.8621396198270475, -6.307003348497942419 ) ) ;
#23035 = EDGE_CURVE ( 'NONE', #31630, #35189, #36622, .T. ) ;
#23036 = CARTESIAN_POINT ( 'NONE',  ( 18.12178482187500350, -4.985214923628407568, -4.228124999385491023 ) ) ;
#23037 = CARTESIAN_POINT ( 'NONE',  ( 5.778771075727756162E-15, 194.9656250006145228, 31.45816453501075927 ) ) ;
#23038 = CARTESIAN_POINT ( 'NONE',  ( -15.50000000000000533, 70.88981371789854791, 0.1745138560722471477 ) ) ;
#23039 = CARTESIAN_POINT ( 'NONE',  ( -36.73586230271183695, 206.8500491399821328, 5.686928522499748340 ) ) ;
#23040 = EDGE_LOOP ( 'NONE', ( #28115, #5877, #32279, #34250 ) ) ;
#23041 = DIRECTION ( 'NONE',  ( -0.1219804832088935975, -0.9925324990730152175, 0.000000000000000000 ) ) ;
#23042 = CARTESIAN_POINT ( 'NONE',  ( 2.660918448318279950, 107.2976862821014521, -12.46528703574805697 ) ) ;
#23043 = CARTESIAN_POINT ( 'NONE',  ( 14.38691631536207538, 44.33518628210144641, -5.770363421893813793 ) ) ;
#23044 = EDGE_CURVE ( 'NONE', #253, #1148, #24335, .T. ) ;
#23045 = CARTESIAN_POINT ( 'NONE',  ( 0.000000000000000000, 148.0000000000000000, 0.000000000000000000 ) ) ;
#23046 = CARTESIAN_POINT ( 'NONE',  ( 30.80420397407610622, 7.209453229046482114, 162.0625642106390671 ) ) ;
#23047 = MECHANICAL_DESIGN_GEOMETRIC_PRESENTATION_REPRESENTATION (  '', ( #30921 ), #9107 ) ;
#23048 = CARTESIAN_POINT ( 'NONE',  ( 15.46528703574804986, 63.59768628210142793, 3.257655550457285720 ) ) ;
#23049 = CARTESIAN_POINT ( 'NONE',  ( 13.44051670066911264, 5.407089921784856479, -8.765624999385545735 ) ) ;
#23050 = CARTESIAN_POINT ( 'NONE',  ( 16.56230152254411081, 6.928203230275514990, -8.662500000000004974 ) ) ;
#23051 = CARTESIAN_POINT ( 'NONE',  ( -47.43080436395489841, 203.5000000000000000, -0.1155267958017335561 ) ) ;
#23052 = CARTESIAN_POINT ( 'NONE',  ( -4.944772684328673229, 47.78518628210144925, 11.48171059495397728 ) ) ;
#23053 = CARTESIAN_POINT ( 'NONE',  ( -13.50000000000000533, 199.0250000000000057, -23.38268590217984411 ) ) ;
#23054 = CARTESIAN_POINT ( 'NONE',  ( -7.234628195640289583, 197.7700961906613770, -27.00000000000001421 ) ) ;
#23055 = CARTESIAN_POINT ( 'NONE',  ( -8.843639120294326972, 12.13518628210144712, 3.474262827703335166 ) ) ;
#23056 = CARTESIAN_POINT ( 'NONE',  ( 15.24356964374999990, 248.4718750006144603, -3.323476615752268604 ) ) ;
#23057 = ORIENTED_EDGE ( 'NONE', *, *, #34267, .T. ) ;
#23058 = CARTESIAN_POINT ( 'NONE',  ( 21.00000000000000000, 6.928203230275506996, -4.162500000000017408 ) ) ;
#23059 = CARTESIAN_POINT ( 'NONE',  ( 26.99999999999999645, 243.4749999999999943, -7.347880794884117764E-16 ) ) ;
#23060 = CARTESIAN_POINT ( 'NONE',  ( 36.81484116775207127, -3.604726614523238837, 159.1275339855211257 ) ) ;
#23061 = CARTESIAN_POINT ( 'NONE',  ( 13.44051670066911264, 5.407089921784856479, -3.365624999385530280 ) ) ;
#23062 = CARTESIAN_POINT ( 'NONE',  ( 28.32999068460662428, 5.407089921784856479, 169.6006407646945604 ) ) ;
#23063 = CARTESIAN_POINT ( 'NONE',  ( 15.00000000000000000, 241.8625000000000114, -3.464101615137752166 ) ) ;
#23064 = CARTESIAN_POINT ( 'NONE',  ( -27.00000000000000355, 196.4750000012289775, -15.58845726811989429 ) ) ;
#23065 = CARTESIAN_POINT ( 'NONE',  ( -6.932735513423968321, 60.14768628210144641, -10.69584247140445221 ) ) ;
#23066 = VERTEX_POINT ( 'NONE', #37266 ) ;
#23067 = ORIENTED_EDGE ( 'NONE', *, *, #24913, .F. ) ;
#23068 = CARTESIAN_POINT ( 'NONE',  ( -13.49999999999998401, 196.5875000012290457, 23.38268590217985476 ) ) ;
#23069 = DIRECTION ( 'NONE',  ( 1.000000000000000000, 0.000000000000000000, 0.000000000000000000 ) ) ;
#23070 = EDGE_CURVE ( 'NONE', #37311, #26550, #5609, .T. ) ;
#23071 = CARTESIAN_POINT ( 'NONE',  ( 5.770363421894130873, 46.16481371789854649, -14.38691631536193860 ) ) ;
#23072 = CARTESIAN_POINT ( 'NONE',  ( 20.99999999999999645, -6.928203230275506996, -5.231249998770948650 ) ) ;
#23073 = CARTESIAN_POINT ( 'NONE',  ( 26.75643035624999655, 241.5718750006145115, -3.323476615752271712 ) ) ;
#23074 = AXIS2_PLACEMENT_3D ( 'NONE', #4604, #16739, #8207 ) ;
#23075 = CARTESIAN_POINT ( 'NONE',  ( -43.07663769728824121, 206.0451222850691408, 2.149950860017832532 ) ) ;
#23076 = CARTESIAN_POINT ( 'NONE',  ( 10.56230152254410726, 0.000000000000000000, -9.900000000000048317 ) ) ;
#23077 = CARTESIAN_POINT ( 'NONE',  ( 27.71064018770612947, -5.407089921784865361, 162.5214321913800859 ) ) ;
#23078 = CARTESIAN_POINT ( 'NONE',  ( -3.796722387233185003, 26.61481371789854933, -8.710071997420207879 ) ) ;
#23079 = EDGE_CURVE ( 'NONE', #14417, #23913, #25528, .T. ) ;
#23080 = CARTESIAN_POINT ( 'NONE',  ( -67.42038769728823411, 208.1428034533959703, 6.469044688360770401 ) ) ;
#23081 = CARTESIAN_POINT ( 'NONE',  ( 0.000000000000000000, 0.000000000000000000, 0.000000000000000000 ) ) ;
#23082 = FACE_OUTER_BOUND ( 'NONE', #32609, .T. ) ;
#23083 = CARTESIAN_POINT ( 'NONE',  ( 27.24356964374999635, 195.1718750006145342, -15.72908226750539029 ) ) ;
#23084 = CARTESIAN_POINT ( 'NONE',  ( 6.092822981423662299, 123.2148137178985792, 14.25334919248795096 ) ) ;
#23085 = EDGE_CURVE ( 'NONE', #34986, #12783, #33607, .T. ) ;
#23086 = ORIENTED_EDGE ( 'NONE', *, *, #20322, .F. ) ;
#23087 = CARTESIAN_POINT ( 'NONE',  ( 10.49813415415989581, 54.97268628210144925, 7.228626920339068285 ) ) ;
#23088 = CARTESIAN_POINT ( 'NONE',  ( 20.99999999999999289, 240.4374999999999716, -5.999999999999997335 ) ) ;
#23089 = LINE ( 'NONE', #34633, #37435 ) ;
#23090 = CARTESIAN_POINT ( 'NONE',  ( 37.60251119283397259, 7.646167579472024665E-16, 168.1306435695252901 ) ) ;
#23091 = CARTESIAN_POINT ( 'NONE',  ( 15.00000000000000178, -3.464101615137757051, -3.056249998770964371 ) ) ;
#23092 = CARTESIAN_POINT ( 'NONE',  ( 22.80587116629411781, 3.604726614523243278, -8.034374999385502036 ) ) ;
#23093 = CARTESIAN_POINT ( 'NONE',  ( 20.99999999999999645, 0.000000000000000000, -8.000000000000000000 ) ) ;
#23094 = CARTESIAN_POINT ( 'NONE',  ( -0.1745138560725182642, 74.81018628210145494, 9.500000000000005329 ) ) ;
#23095 = DIRECTION ( 'NONE',  ( -0.000000000000000000, -1.000000000000000000, -0.000000000000000000 ) ) ;
#23096 = DIRECTION ( 'NONE',  ( 0.000000000000000000, -0.000000000000000000, -1.000000000000000000 ) ) ;
#23097 = EDGE_CURVE ( 'NONE', #8415, #20125, #2403, .T. ) ;
#23098 = CARTESIAN_POINT ( 'NONE',  ( 10.69584247140445221, 99.24768628210146915, -6.932735513423970097 ) ) ;
#23099 = CARTESIAN_POINT ( 'NONE',  ( 24.00000000000000000, 249.7000000000000171, 5.196152422706629359 ) ) ;
#23100 = CARTESIAN_POINT ( 'NONE',  ( -27.00000000000000355, 195.1250000012290400, -15.58845726811989429 ) ) ;
#23101 = ORIENTED_EDGE ( 'NONE', *, *, #19026, .F. ) ;
#23102 = CARTESIAN_POINT ( 'NONE',  ( 24.52066036092156054, 0.000000000000000000, 161.8782597873571660 ) ) ;
#23103 = CARTESIAN_POINT ( 'NONE',  ( 18.12178482187500350, -4.985214923628407568, -7.265624999385461358 ) ) ;
#23104 = CARTESIAN_POINT ( 'NONE',  ( 27.24356964375000345, 195.5843750006145285, -3.336375036156643733E-15 ) ) ;
#23105 = CARTESIAN_POINT ( 'NONE',  ( 28.12898775289485442, 5.407089921784862696, 167.3031667422204691 ) ) ;
#23106 = CARTESIAN_POINT ( 'NONE',  ( 25.28215217963245465, 3.464101615137757051, 167.7875028556105974 ) ) ;
#23107 = CARTESIAN_POINT ( 'NONE',  ( 8.562301522544109034, 9.797174393178823685E-16, 2.535898384862258492 ) ) ;
#23108 = CARTESIAN_POINT ( 'NONE',  ( 19.00081571707362116, 239.8729221881839351, -5.492723647597327563 ) ) ;
#23109 = CARTESIAN_POINT ( 'NONE',  ( 27.24356964375000345, 198.2281250006145399, -3.336375036156643733E-15 ) ) ;
#23110 = CARTESIAN_POINT ( 'NONE',  ( 4.622313124798831829, 128.9648137178985507, -11.61527771782809282 ) ) ;
#23111 = APPLICATION_CONTEXT ( 'automotive_design' ) ;
#23112 = CARTESIAN_POINT ( 'NONE',  ( 12.50000000000000355, 127.7101862821014606, 0.1745138560725507937 ) ) ;
#23114 = ORIENTED_EDGE ( 'NONE', *, *, #37125, .T. ) ;
#23113 = ORIENTED_EDGE ( 'NONE', *, *, #17058, .T. ) ;
#23115 = CARTESIAN_POINT ( 'NONE',  ( -27.24356964375000345, 197.1031250006145399, 0.000000000000000000 ) ) ;
#23116 = CARTESIAN_POINT ( 'NONE',  ( 26.75643035624999655, 242.2843750006145171, 3.323476615752267715 ) ) ;
#23117 = CARTESIAN_POINT ( 'NONE',  ( 13.56230152254411436, -5.196152422706638241, -3.075000000000049916 ) ) ;
#23118 = EDGE_CURVE ( 'NONE', #3827, #19208, #8291, .T. ) ;
#23119 = CARTESIAN_POINT ( 'NONE',  ( -15.46528703574811736, 98.20231371789854791, 3.257655550456946436 ) ) ;
#23120 =( BOUNDED_CURVE ( )  B_SPLINE_CURVE ( 2, ( #9523, #6866, #12165, #4014, #35277, #26758, #27329, #32444, #1358 ),
 .UNSPECIFIED., .F., .F. ) 
 B_SPLINE_CURVE_WITH_KNOTS ( ( 3, 2, 2, 2, 3 ),
 ( 0.2934782608695652439, 0.2971014492753623060, 0.3043478260869565410, 0.3115942028985507206, 0.3152173913043477826 ),
 .UNSPECIFIED. ) 
 CURVE ( )  GEOMETRIC_REPRESENTATION_ITEM ( )  RATIONAL_B_SPLINE_CURVE ( ( 0.9330127018922194093, 0.9330127018922198534, 1.000000000000000000, 0.8660254037844387076, 1.000000000000000000, 0.8660254037844387076, 1.000000000000000000, 0.9330127018922198534, 0.9330127018922191873 ) ) 
 REPRESENTATION_ITEM ( '' )  );
#23121 = CARTESIAN_POINT ( 'NONE',  ( 26.75643035624999655, -3.323476615752267715, -3.215624999385490401 ) ) ;
#23122 = CARTESIAN_POINT ( 'NONE',  ( -13.49999999999998401, 195.6875000012290400, 23.38268590217985476 ) ) ;
#23123 = CARTESIAN_POINT ( 'NONE',  ( -6.840914352311947333, 72.03981371789855359, -6.594114490232462877 ) ) ;
#23124 = CARTESIAN_POINT ( 'NONE',  ( 16.56230152254411436, 7.209453229046475009, -2.503124999385547778 ) ) ;
#23125 = CARTESIAN_POINT ( 'NONE',  ( 26.75643035624999655, 242.2843750006145456, 3.323476615752267271 ) ) ;
#23126 = CARTESIAN_POINT ( 'NONE',  ( -8.715434833792127023, 51.33981371789855785, 8.962234695871568846 ) ) ;
#23127 = ADVANCED_FACE ( 'NONE', ( #8469 ), #14159, .T. ) ;
#23128 = CIRCLE ( 'NONE', #15857, 2.499999999999996891 ) ;
#23129 = CYLINDRICAL_SURFACE ( 'NONE', #26093, 5.999999999999998224 ) ;
#23130 = CARTESIAN_POINT ( 'NONE',  ( -11.48171059495397373, 96.08518628210146062, -4.944772684328680334 ) ) ;
#23131 = CARTESIAN_POINT ( 'NONE',  ( 10.56230152254410726, 3.464101615137752166, -3.074999998770978404 ) ) ;
#23132 =( BOUNDED_CURVE ( )  B_SPLINE_CURVE ( 2, ( #30238, #27018, #1043, #1417, #24180, #12995, #24551 ),
 .UNSPECIFIED., .F., .F. ) 
 B_SPLINE_CURVE_WITH_KNOTS ( ( 3, 2, 2, 3 ),
 ( 0.04347826086956516761, 0.05072463768115921534, 0.05797101449275325613, 0.06521739130434729692 ),
 .UNSPECIFIED. ) 
 CURVE ( )  GEOMETRIC_REPRESENTATION_ITEM ( )  RATIONAL_B_SPLINE_CURVE ( ( 1.000000000000000888, 0.8660254037844378194, 1.000000000000000000, 0.8660254037844387076, 1.000000000000000000, 0.8660254037844484776, 0.9999999999999902300 ) ) 
 REPRESENTATION_ITEM ( '' )  );
#23133 = CARTESIAN_POINT ( 'NONE',  ( -69.79538769728823411, 211.3212981617418222, -4.469044688360751749 ) ) ;
#23134 = CARTESIAN_POINT ( 'NONE',  ( -74.35000000000003695, 210.0000000000000000, 5.000000000000000888 ) ) ;
#23135 = CARTESIAN_POINT ( 'NONE',  ( -13.49999999999998401, 198.8375000012290457, 23.38268590217985476 ) ) ;
#23136 = CARTESIAN_POINT ( 'NONE',  ( 11.08355503943142750, 108.1601862821014635, -10.83675517735155225 ) ) ;
#23137 = CARTESIAN_POINT ( 'NONE',  ( -12.46528703574805874, 12.99768628210143362, -2.660918448318280838 ) ) ;
#23138 = CARTESIAN_POINT ( 'NONE',  ( 10.56230152254273058, 3.464101615136960355, -8.137500000000033040 ) ) ;
#23139 = CARTESIAN_POINT ( 'NONE',  ( 27.00000000000000355, 196.7375000012290229, -3.306546357697854128E-15 ) ) ;
#23140 = CARTESIAN_POINT ( 'NONE',  ( 8.710071997420127943, 137.4851862821014379, 3.796722387233375073 ) ) ;
#23141 = CARTESIAN_POINT ( 'NONE',  ( 26.99999999999999645, 7.347880794884117764E-16, -4.668749998770954868 ) ) ;
#23142 = CARTESIAN_POINT ( 'NONE',  ( 21.00000000000000000, 243.1093750006145058, 6.646953231504538984 ) ) ;
#23143 = ORIENTED_EDGE ( 'NONE', *, *, #6466, .F. ) ;
#23144 = CARTESIAN_POINT ( 'NONE',  ( 25.14491336835161306, 3.604726614523236616, 169.0135043124392951 ) ) ;
#23145 = CARTESIAN_POINT ( 'NONE',  ( 9.500000000000005329, 63.31018628210144783, 0.1745138560725188748 ) ) ;
#23146 = CARTESIAN_POINT ( 'NONE',  ( 26.99999999999999645, 244.0187500012290513, -3.464101615137755275 ) ) ;
#23148 = EDGE_CURVE ( 'NONE', #25162, #36971, #28203, .T. ) ;
#23147 = CARTESIAN_POINT ( 'NONE',  ( 26.99999999999999645, 241.2249999999999943, -7.347880794884117764E-16 ) ) ;
#23149 = CARTESIAN_POINT ( 'NONE',  ( 15.00000000000000000, 0.000000000000000000, -2.700000000000008171 ) ) ;
#23150 = CARTESIAN_POINT ( 'NONE',  ( 27.24356964375000700, 195.5468750006145342, 15.72908226750537075 ) ) ;
#23151 = CARTESIAN_POINT ( 'NONE',  ( 20.99999999999997513, 246.2874999999999943, -5.999999999999999112 ) ) ;
#23152 = CARTESIAN_POINT ( 'NONE',  ( 21.00000000000000355, 0.000000000000000000, 50.00000000000001421 ) ) ;
#23153 = CARTESIAN_POINT ( 'NONE',  ( -5.529263428287297444, 35.52731371789855075, -7.954856959092311719 ) ) ;
#23154 = PLANE ( 'NONE',  #21836 ) ;
#23155 = ORIENTED_EDGE ( 'NONE', *, *, #22405, .F. ) ;
#23156 = VERTEX_POINT ( 'NONE', #28733 ) ;
#23157 = CARTESIAN_POINT ( 'NONE',  ( 23.87821517812500005, 249.4468750006145115, 4.985214923628404016 ) ) ;
#23158 = CARTESIAN_POINT ( 'NONE',  ( -12.46528703574811558, 52.20231371789854791, 2.660918448318004170 ) ) ;
#23159 = CARTESIAN_POINT ( 'NONE',  ( 19.68408634441912142, -5.407089921784861808, -7.696874999385511451 ) ) ;
#23160 = CARTESIAN_POINT ( 'NONE',  ( 15.24356964374999990, 0.000000000000000000, -9.253124999385493155 ) ) ;
#23161 = CARTESIAN_POINT ( 'NONE',  ( 2.660918448318002838, 13.10231371789855004, 12.46528703574811558 ) ) ;
#23162 = ADVANCED_FACE ( 'NONE', ( #2772 ), #8653, .T. ) ;
#23163 = EDGE_LOOP ( 'NONE', ( #28234, #21352 ) ) ;
#23164 = CARTESIAN_POINT ( 'NONE',  ( 10.31873187879410736, 0.000000000000000000, -2.896874999385512517 ) ) ;
#23165 = CARTESIAN_POINT ( 'NONE',  ( 27.24356964375000700, 198.1906250006145740, 15.72908226750537075 ) ) ;
#23166 = CARTESIAN_POINT ( 'NONE',  ( 24.90795869275643426, 0.000000000000000000, 166.3050999770023850 ) ) ;
#23167 = CARTESIAN_POINT ( 'NONE',  ( -67.41294563604516554, 216.1378603801729241, -6.307003348498026796 ) ) ;
#23168 = CARTESIAN_POINT ( 'NONE',  ( 26.75643035624999655, 248.1343750006145399, 3.323476615752267271 ) ) ;
#23169 = CARTESIAN_POINT ( 'NONE',  ( -12.09976244894570563, 194.9999999999999432, 24.41260623486415682 ) ) ;
#23170 = CARTESIAN_POINT ( 'NONE',  ( -61.27752896937849414, 212.3500491399821613, 3.839350919129088435 ) ) ;
#23171 = CARTESIAN_POINT ( 'NONE',  ( -45.25372103062155560, 216.5309553116391612, -1.626142955000564383 ) ) ;
#23172 = CARTESIAN_POINT ( 'NONE',  ( 25.10896162446820412, 0.000000000000000000, 168.6025739994764479 ) ) ;
#23173 = VERTEX_POINT ( 'NONE', #5425 ) ;
#23174 = DIRECTION ( 'NONE',  ( 0.000000000000000000, 1.000000000000000000, 0.000000000000000000 ) ) ;
#23175 = CARTESIAN_POINT ( 'NONE',  ( -15.53471296425188442, 25.17731371789854933, -2.908627838312459080 ) ) ;
#23176 = CARTESIAN_POINT ( 'NONE',  ( -64.45163769728823411, 217.4189793300686233, -4.149950860017907139 ) ) ;
#23177 = PRODUCT ( 'handle link', 'handle link', '', ( #27408 ) ) ;
#23178 = CARTESIAN_POINT ( 'NONE',  ( 0.1745138560725515708, 15.01018628210143468, -12.50000000000000355 ) ) ;
#23179 = CARTESIAN_POINT ( 'NONE',  ( 2.311890736173175753, 46.92268628210145209, 12.53471296425194836 ) ) ;
#23180 = CARTESIAN_POINT ( 'NONE',  ( 16.56230152254411436, -6.928203230275514990, -3.487500000000039346 ) ) ;
#23181 = ORIENTED_EDGE ( 'NONE', *, *, #21864, .F. ) ;
#23182 = CARTESIAN_POINT ( 'NONE',  ( -38.12872103062155560, 203.4690446883607535, 1.626142955000567936 ) ) ;
#23183 = CARTESIAN_POINT ( 'NONE',  ( -13.49999999999998401, 198.8375000012290457, 23.38268590217985476 ) ) ;
#23184 = CARTESIAN_POINT ( 'NONE',  ( -27.24356964375000345, 195.8093750006145513, 0.000000000000000000 ) ) ;
#23185 = CARTESIAN_POINT ( 'NONE',  ( 25.29849388150488210, -3.464101615137825441, 167.9742893627271485 ) ) ;
#23186 = CIRCLE ( 'NONE', #21397, 5.999999999999998224 ) ;
#23187 = CARTESIAN_POINT ( 'NONE',  ( 13.50000000000001421, 196.2125000012290172, 23.38268590217984055 ) ) ;
#23188 = DIRECTION ( 'NONE',  ( -0.000000000000000000, 1.000000000000000000, -0.000000000000000000 ) ) ;
#23189 = DIRECTION ( 'NONE',  ( -1.000000000000000000, 0.000000000000000000, 1.558072081575740353E-16 ) ) ;
#23190 = CARTESIAN_POINT ( 'NONE',  ( 21.00000000000000000, 245.9218750006145058, 6.646953231504538984 ) ) ;
#23191 = CARTESIAN_POINT ( 'NONE',  ( -8.843639120294245259, 99.06481371789857349, -3.474262827703533230 ) ) ;
#23192 = CARTESIAN_POINT ( 'NONE',  ( 30.80175271875777199, -6.928203230275514990, 162.0345462341430505 ) ) ;
#23193 = ORIENTED_EDGE ( 'NONE', *, *, #23790, .T. ) ;
#23194 = CARTESIAN_POINT ( 'NONE',  ( -58.90997103062156270, 215.5714017266979852, 3.350049139982118618 ) ) ;
#23195 = DIRECTION ( 'NONE',  ( 1.000000000000000000, 0.000000000000000000, 0.000000000000000000 ) ) ;
#23196 = CARTESIAN_POINT ( 'NONE',  ( 15.00000000000000000, 245.9687500012290684, -3.464101615137752166 ) ) ;
#23197 = VERTEX_POINT ( 'NONE', #28547 ) ;
#23198 = CARTESIAN_POINT ( 'NONE',  ( -4.622313124798826500, 96.76481371789854791, 11.61527771782809637 ) ) ;
#23199 = CARTESIAN_POINT ( 'NONE',  ( 19.68408634441911076, 5.407089921784862696, -1.696874999385505900 ) ) ;
#23200 = CARTESIAN_POINT ( 'NONE',  ( 7.234628195640322446, 197.9950961906613429, 26.99999999999999645 ) ) ;
#23201 = CARTESIAN_POINT ( 'NONE',  ( 15.24356964374999990, 3.323476615752268604, -2.540624999385480809 ) ) ;
#23202 = CARTESIAN_POINT ( 'NONE',  ( 10.69584247140429589, 67.15231371789855075, 6.932735513424201024 ) ) ;
#23203 = CARTESIAN_POINT ( 'NONE',  ( 5.727106289114498080E-15, 195.1625000000000227, 31.17691453623979214 ) ) ;
#23204 = ORIENTED_EDGE ( 'NONE', *, *, #24532, .F. ) ;
#23205 = ORIENTED_EDGE ( 'NONE', *, *, #11687, .T. ) ;
#23206 = ORIENTED_EDGE ( 'NONE', *, *, #14077, .F. ) ;
#23207 = CARTESIAN_POINT ( 'NONE',  ( 20.99999999999999645, -6.646953231504538984, -4.528124999385448213 ) ) ;
#23208 = CARTESIAN_POINT ( 'NONE',  ( 30.62526233969377998, 6.928203230275514990, 160.0172519705072318 ) ) ;
#23209 = CARTESIAN_POINT ( 'NONE',  ( 21.00000000000000000, 246.7093750006145285, 6.646953231504538984 ) ) ;
#23210 = CARTESIAN_POINT ( 'NONE',  ( -4.944772684328673229, 38.58518628210144641, 11.48171059495397728 ) ) ;
#23211 = CARTESIAN_POINT ( 'NONE',  ( -49.00669563604516554, 209.8844732041982013, -6.500000000000000888 ) ) ;
#23212 = EDGE_CURVE ( 'NONE', #23833, #21861, #29174, .T. ) ;
#23213 = CARTESIAN_POINT ( 'NONE',  ( 19.44430458907289605, 214.1485210958233836, -5.808099892140725196 ) ) ;
#23214 = CARTESIAN_POINT ( 'NONE',  ( -41.68377896937850124, 208.9097554298617183, 4.530955311639234040 ) ) ;
#23215 = SURFACE_STYLE_USAGE ( .BOTH. , #25680 ) ;
#23216 = CARTESIAN_POINT ( 'NONE',  ( 27.78048522105927987, -5.196152422706632912, 161.9224404518259064 ) ) ;
#23217 = CARTESIAN_POINT ( 'NONE',  ( 11.61527771782809637, 112.8648137178985564, 4.622313124798827388 ) ) ;
#23218 = CARTESIAN_POINT ( 'NONE',  ( -65.24330436395489130, 210.1155267958017703, -4.499999999999996447 ) ) ;
#23219 = CARTESIAN_POINT ( 'NONE',  ( -39.31622103062156981, 212.1620413398628671, 8.530955311639223382 ) ) ;
#23220 = CARTESIAN_POINT ( 'NONE',  ( 26.75643035624999655, 7.049594010296217766E-16, -3.628124999385473615 ) ) ;
#23221 = CARTESIAN_POINT ( 'NONE',  ( -20.86978604919638869, 194.8026013911397740, -17.51182792271053046 ) ) ;
#23222 = CARTESIAN_POINT ( 'NONE',  ( -5.770363421894122880, 78.36481371789855643, 14.38691631536194393 ) ) ;
#23223 = CARTESIAN_POINT ( 'NONE',  ( -59.29836230271182984, 202.5810206699313767, -4.149950860017804111 ) ) ;
#23224 = ORIENTED_EDGE ( 'NONE', *, *, #8424, .T. ) ;
#23225 = FACE_OUTER_BOUND ( 'NONE', #912, .T. ) ;
#23226 = CARTESIAN_POINT ( 'NONE',  ( -11.48171059495397373, 105.2851862821014493, -4.944772684328680334 ) ) ;
#23227 = CARTESIAN_POINT ( 'NONE',  ( -8.927990412390661490, 38.87268628210144072, 13.04141134922759804 ) ) ;
#23228 = CARTESIAN_POINT ( 'NONE',  ( 19.98630977700905831, 239.7005235349005829, -5.748934002787875919 ) ) ;
#23229 = CARTESIAN_POINT ( 'NONE',  ( 36.97825818540390941, 3.604726614523243278, 160.9953990444431611 ) ) ;
#23230 = CARTESIAN_POINT ( 'NONE',  ( -8.632099005475501130, 69.34768628210143504, -13.23911966647218996 ) ) ;
#23231 = CARTESIAN_POINT ( 'NONE',  ( -27.24356964375000345, 199.7656250006145342, -15.72908226750537786 ) ) ;
#23232 = CARTESIAN_POINT ( 'NONE',  ( 10.31873187879411091, 3.604726614523236616, -10.07812499938551198 ) ) ;
#23233 = LINE ( 'NONE', #9009, #8584 ) ;
#23234 = CARTESIAN_POINT ( 'NONE',  ( -53.96205436395489130, 214.6737587650352168, 4.842901733360204908 ) ) ;
#23235 = CARTESIAN_POINT ( 'NONE',  ( 10.53852972689264433, -1.498109391770361842, -10.00000000000000355 ) ) ;
#23236 = CARTESIAN_POINT ( 'NONE',  ( 6.932735513423970097, 37.14768628210143930, 10.69584247140445044 ) ) ;
#23237 = CARTESIAN_POINT ( 'NONE',  ( 5.778771075727756162E-15, 199.5218750006145854, 31.45816453501075927 ) ) ;
#23238 = CARTESIAN_POINT ( 'NONE',  ( 20.99999999999999645, 6.928203230275506996, -7.706249998770941190 ) ) ;
#23239 = CARTESIAN_POINT ( 'NONE',  ( -5.529263428287477744, 11.27268628210142865, 7.954856959092191815 ) ) ;
#23240 = CARTESIAN_POINT ( 'NONE',  ( 20.99999999999999645, 248.8468750006145456, -6.646953231504538984 ) ) ;
#23241 = AXIS2_PLACEMENT_3D ( 'NONE', #26821, #15835, #21345 ) ;
#23242 = ORIENTED_EDGE ( 'NONE', *, *, #9647, .F. ) ;
#23243 = CARTESIAN_POINT ( 'NONE',  ( 21.00000000000000000, 6.928203230275506996, -5.512500000000003730 ) ) ;
#23244 = MECHANICAL_DESIGN_GEOMETRIC_PRESENTATION_REPRESENTATION (  '', ( #34112 ), #22032 ) ;
#23245 = DIRECTION ( 'NONE',  ( 0.08715574274765150453, 0.000000000000000000, 0.9961946980917461003 ) ) ;
#23246 = CARTESIAN_POINT ( 'NONE',  ( 15.00000000000000000, 0.000000000000000000, -6.693749998770953447 ) ) ;
#23247 = CARTESIAN_POINT ( 'NONE',  ( 10.31873187879411091, 3.604726614523236616, -5.578124999385555505 ) ) ;
#23248 = CARTESIAN_POINT ( 'NONE',  ( 25.03378979634835488, -3.604726614523240613, 167.7433560723723076 ) ) ;
#23249 = CARTESIAN_POINT ( 'NONE',  ( 15.00000000000000000, 242.3125000000000000, -3.464101615137752166 ) ) ;
#23250 = CARTESIAN_POINT ( 'NONE',  ( 23.99999999999999645, 5.196152422706631135, -0.9937499987709430549 ) ) ;
#23251 = AXIS2_PLACEMENT_3D ( 'NONE', #11115, #8279, #19852 ) ;
#23252 = CARTESIAN_POINT ( 'NONE',  ( -11.48171059495397373, 68.48518628210145209, -4.944772684328680334 ) ) ;
#23253 = ORIENTED_EDGE ( 'NONE', *, *, #25713, .F. ) ;
#23254 = ORIENTED_EDGE ( 'NONE', *, *, #10065, .F. ) ;
#23255 = CARTESIAN_POINT ( 'NONE',  ( 24.99999999999999289, 0.000000000000000000, 49.65004534589634488 ) ) ;
#23256 = CARTESIAN_POINT ( 'NONE',  ( -27.00000000000000355, 195.1625000012290343, 0.000000000000000000 ) ) ;
#23257 = CARTESIAN_POINT ( 'NONE',  ( -47.00000000000000711, 244.5000000000000000, 0.4999999999999995559 ) ) ;
#23258 = CARTESIAN_POINT ( 'NONE',  ( 26.75643035624999655, 3.323476615752271712, -7.078124999385466687 ) ) ;
#23259 = CARTESIAN_POINT ( 'NONE',  ( 3.257655550456945548, 40.70231371789854791, 15.46528703574811736 ) ) ;
#23260 = CARTESIAN_POINT ( 'NONE',  ( 20.00041244883536606, 5.668978318349186196, -10.25260146540740003 ) ) ;
#23261 = CARTESIAN_POINT ( 'NONE',  ( 26.75643035624999655, 240.2218750006145171, -3.323476615752271712 ) ) ;
#23262 = CARTESIAN_POINT ( 'NONE',  ( -46.04538769728823411, 211.3212981617418222, -4.469044688360751749 ) ) ;
#23263 = CARTESIAN_POINT ( 'NONE',  ( 20.99999999999995026, 242.7437500012290741, -5.999999999999998224 ) ) ;
#23264 = CARTESIAN_POINT ( 'NONE',  ( 37.39010055343325689, 3.464101615137755275, 168.4974270992498475 ) ) ;
#23265 = CARTESIAN_POINT ( 'NONE',  ( 9.500000000000005329, 29.48981371789855288, -0.1745138560723090149 ) ) ;
#23266 = CARTESIAN_POINT ( 'NONE',  ( -59.89955436395490551, 214.8429017333601792, -4.673758765035196383 ) ) ;
#23267 = CARTESIAN_POINT ( 'NONE',  ( -41.19590334923083930, -31.88285731531777145, 5.000000000000000000 ) ) ;
#23268 = DIRECTION ( 'NONE',  ( -0.5887012860850800999, 0.8083506638593009885, -0.000000000000000000 ) ) ;
#23269 = CARTESIAN_POINT ( 'NONE',  ( -1.926257025242585782E-15, 197.0468750006145626, -31.45816453501075927 ) ) ;
#23270=STYLED_ITEM('',(#37542),#8321);
#23271 = CARTESIAN_POINT ( 'NONE',  ( -14.38691631536193860, 126.6648137178985820, -5.770363421894132649 ) ) ;
#23272 = AXIS2_PLACEMENT_3D ( 'NONE', #32346, #3541, #686 ) ;
#23273 = VERTEX_POINT ( 'NONE', #31955 ) ;
#23274 = CARTESIAN_POINT ( 'NONE',  ( 12.46528703574805874, 45.19768628210143646, 2.660918448318279950 ) ) ;
#23275 = CARTESIAN_POINT ( 'NONE',  ( 16.56230152254411081, -6.928203230275506996, -8.324999998771003717 ) ) ;
#23276 = ADVANCED_FACE ( 'NONE', ( #5986 ), #17566, .F. ) ;
#23277 = CARTESIAN_POINT ( 'NONE',  ( 20.99999999999997513, 247.1875000000000284, -5.999999999999999112 ) ) ;
#23278 = CARTESIAN_POINT ( 'NONE',  ( 28.25972136701633630, -5.407089921784865361, 168.7974587893581315 ) ) ;
#23279 = CARTESIAN_POINT ( 'NONE',  ( 21.00000000000000000, 6.928203230275506996, -2.756249998770956111 ) ) ;
#23280 = CARTESIAN_POINT ( 'NONE',  ( 13.44051670066910908, 5.407089921784862696, -8.821874999385526550 ) ) ;
#23281 = CARTESIAN_POINT ( 'NONE',  ( -13.49999999999998401, 197.0375000012290627, 23.38268590217985476 ) ) ;
#23282 = CARTESIAN_POINT ( 'NONE',  ( -8.152565276336710909, 57.84768628210144925, 5.233372021372435512 ) ) ;
#23283 = DIRECTION ( 'NONE',  ( 0.000000000000000000, 0.000000000000000000, 1.000000000000000000 ) ) ;
#23284 = CARTESIAN_POINT ( 'NONE',  ( 21.00000000000000000, 245.6125000000000114, 5.999999999999998224 ) ) ;
#23285 = CARTESIAN_POINT ( 'NONE',  ( -11.61527771782819940, 85.73518628210143788, 4.622313124798574258 ) ) ;
#23286 = CYLINDRICAL_SURFACE ( 'NONE', #5753, 5.999999999999998224 ) ;
#23287 = LINE ( 'NONE', #9251, #31098 ) ;
#23288 = ORIENTED_EDGE ( 'NONE', *, *, #14244, .F. ) ;
#23289 = CARTESIAN_POINT ( 'NONE',  ( 30.90715669519676467, -7.209453229046475009, 163.2393191977599258 ) ) ;
#23290 = CARTESIAN_POINT ( 'NONE',  ( 21.00000000000000000, 6.646953231504538984, -7.903124999385464200 ) ) ;
#23291 = CARTESIAN_POINT ( 'NONE',  ( 27.24356964375000700, 195.9968750006145513, 15.72908226750537075 ) ) ;
#23292 = CARTESIAN_POINT ( 'NONE',  ( 37.37045902776835504, 3.604726614523243278, 165.4782751858560061 ) ) ;
#23293 = CARTESIAN_POINT ( 'NONE',  ( 25.28542051998549667, 0.000000000000000000, 167.8248601567890432 ) ) ;
#23294 = CARTESIAN_POINT ( 'NONE',  ( 13.56230152254410548, 5.196152422706636465, -9.075000000000027711 ) ) ;
#23295 = CARTESIAN_POINT ( 'NONE',  ( 15.00000000000000000, 247.2624999999999886, -3.464101615137752166 ) ) ;
#23296 = CARTESIAN_POINT ( 'NONE',  ( 27.24356964375000345, 197.7781250006145228, -3.336375036156643733E-15 ) ) ;
#23297 = CARTESIAN_POINT ( 'NONE',  ( -2.660918448318004614, 128.1023137178985678, -12.46528703574811558 ) ) ;
#23298 = CARTESIAN_POINT ( 'NONE',  ( 6.932735513423970097, 119.9476862821014578, 10.69584247140445044 ) ) ;
#23300 = EDGE_LOOP ( 'NONE', ( #3441, #20415, #14666, #26353 ) ) ;
#23299 = ORIENTED_EDGE ( 'NONE', *, *, #31874, .F. ) ;
#23301 = CARTESIAN_POINT ( 'NONE',  ( -13.62178482187500528, 197.0281250006145228, -23.59362340125807123 ) ) ;
#23302 = CARTESIAN_POINT ( 'NONE',  ( 26.75643035624999655, 243.2593750006145115, -3.323476615752271712 ) ) ;
#23303 = EDGE_CURVE ( 'NONE', #33968, #24114, #11032, .T. ) ;
#23304 = CARTESIAN_POINT ( 'NONE',  ( 15.53471296425188797, 103.3773137178985451, 2.908627838312457747 ) ) ;
#23305 = CARTESIAN_POINT ( 'NONE',  ( 26.75643035624999655, 3.323476615752271712, -4.040624999385487470 ) ) ;
#23306 = CARTESIAN_POINT ( 'NONE',  ( 26.75643035624999655, 246.9343750006145228, -7.049594010296217766E-16 ) ) ;
#23307 = CARTESIAN_POINT ( 'NONE',  ( -1.909035429704832693E-15, 196.8500000012290343, -31.17691453623979214 ) ) ;
#23308 = CARTESIAN_POINT ( 'NONE',  ( -0.1745138560723084320, 82.38981371789856212, -9.500000000000005329 ) ) ;
#23309 = CARTESIAN_POINT ( 'NONE',  ( 19.68408634441910721, 5.407089921784857367, -5.690624999385579308 ) ) ;
#23310 = CARTESIAN_POINT ( 'NONE',  ( 20.99999999999999645, 242.2093750006144717, 6.646953231504538984 ) ) ;
#23311 = CARTESIAN_POINT ( 'NONE',  ( 2.311890736173452865, 45.87731371789854506, -12.53471296425189152 ) ) ;
#23312 = CARTESIAN_POINT ( 'NONE',  ( -77.00000000000002842, 210.0000000000000000, 5.000000000000000000 ) ) ;
#23313 = CARTESIAN_POINT ( 'NONE',  ( -11.61527771782819940, 94.93518628210145494, 4.622313124798574258 ) ) ;
#23314 = CARTESIAN_POINT ( 'NONE',  ( 22.56230152254410370, 3.464101615137755275, -3.224999998770998744 ) ) ;
#23315 = CARTESIAN_POINT ( 'NONE',  ( -69.39955436395489130, 213.3788001182225003, -3.209657149897400252 ) ) ;
#23316 = CYLINDRICAL_SURFACE ( 'NONE', #1636, 6.000000000000001776 ) ;
#23317 = CARTESIAN_POINT ( 'NONE',  ( 8.632099005475504683, 101.5476862821014663, 13.23911966647218996 ) ) ;
#23318 = CARTESIAN_POINT ( 'NONE',  ( -4.944772684328673229, 20.18518628210144783, 11.48171059495397728 ) ) ;
#23319 = CARTESIAN_POINT ( 'NONE',  ( 24.96839150574053434, 3.464101615137542112, 164.2012019424803100 ) ) ;
#23320 = CARTESIAN_POINT ( 'NONE',  ( 19.39230484541326760, 241.5986538117967370, 5.999999999999999112 ) ) ;
#23321 = CARTESIAN_POINT ( 'NONE',  ( 7.954856959092191815, 128.5726862821014436, 5.529263428287477744 ) ) ;
#23322 = CARTESIAN_POINT ( 'NONE',  ( 5.778771075727756162E-15, 196.3718750006145513, 31.45816453501075927 ) ) ;
#23323 = CARTESIAN_POINT ( 'NONE',  ( 23.87821517812499650, 241.9468750006145115, -4.985214923628404904 ) ) ;
#23324 = ORIENTED_EDGE ( 'NONE', *, *, #13888, .F. ) ;
#23325 = CARTESIAN_POINT ( 'NONE',  ( 25.14818170870464797, 0.000000000000000000, 169.0508616136177409 ) ) ;
#23326 = CARTESIAN_POINT ( 'NONE',  ( 7.954856959092191815, 54.97268628210144215, 5.529263428287477744 ) ) ;
#23327 = FACE_OUTER_BOUND ( 'NONE', #5754, .T. ) ;
#23328 = DIRECTION ( 'NONE',  ( 0.000000000000000000, 0.000000000000000000, 1.000000000000000000 ) ) ;
#23330 = CARTESIAN_POINT ( 'NONE',  ( 15.00000000000000000, 0.000000000000000000, -3.599999999999992095 ) ) ;
#23329 =( BOUNDED_CURVE ( )  B_SPLINE_CURVE ( 2, ( #8391, #16183, #16555, #2133, #27733, #30956, #22245, #10477, #10666 ),
 .UNSPECIFIED., .F., .F. ) 
 B_SPLINE_CURVE_WITH_KNOTS ( ( 3, 2, 2, 2, 3 ),
 ( 0.6458333333333333703, 0.6527777777777777901, 0.6666666666666666297, 0.6805555555555555802, 0.6875000000000000000 ),
 .UNSPECIFIED. ) 
 CURVE ( )  GEOMETRIC_REPRESENTATION_ITEM ( )  RATIONAL_B_SPLINE_CURVE ( ( 0.9330127018922192983, 0.9330127018922198534, 1.000000000000000000, 0.8660254037844387076, 1.000000000000000000, 0.8660254037844387076, 1.000000000000000000, 0.9330127018922194093, 0.9330127018922194093 ) ) 
 REPRESENTATION_ITEM ( '' )  );
#23331 = CARTESIAN_POINT ( 'NONE',  ( 13.62178482187501416, 195.5093750006145399, 23.59362340125806767 ) ) ;
#23332 = DIRECTION ( 'NONE',  ( 0.000000000000000000, -1.000000000000000000, 0.000000000000000000 ) ) ;
#23333 = CARTESIAN_POINT ( 'NONE',  ( 10.56230152254332033, -3.464101615137297419, -5.699999998771033916 ) ) ;
#23334 = CARTESIAN_POINT ( 'NONE',  ( -0.1745138560723084320, 45.58981371789855785, -9.500000000000005329 ) ) ;
#23335 = CARTESIAN_POINT ( 'NONE',  ( -13.62178482187500528, 199.7843750006145456, -23.59362340125807123 ) ) ;
#23336 = ORIENTED_EDGE ( 'NONE', *, *, #3678, .T. ) ;
#23337 = ORIENTED_EDGE ( 'NONE', *, *, #34029, .T. ) ;
#23338 = CARTESIAN_POINT ( 'NONE',  ( 15.24356964374999990, 249.2968750006145058, 0.000000000000000000 ) ) ;
#23339 = CARTESIAN_POINT ( 'NONE',  ( 0.1745138560722779009, 50.18981371789854506, 12.50000000000000355 ) ) ;
#23340 = CARTESIAN_POINT ( 'NONE',  ( 22.80587116629412137, 7.646167579472024665E-16, -8.971874999385509142 ) ) ;
#23341 = CARTESIAN_POINT ( 'NONE',  ( 26.75643035624999655, -3.323476615752267715, -9.965624999385457983 ) ) ;
#23342 = CARTESIAN_POINT ( 'NONE',  ( -2.311890736173448424, 13.67731371789854400, 12.53471296425189330 ) ) ;
#23343 = ORIENTED_EDGE ( 'NONE', *, *, #31169, .F. ) ;
#23344 = CARTESIAN_POINT ( 'NONE',  ( 16.56230152254411436, 7.209453229046482114, -4.809374999385505944 ) ) ;
#23345 = CARTESIAN_POINT ( 'NONE',  ( 19.39230484541324628, 245.9138461906613315, -5.999999999999989342 ) ) ;
#23346 = CARTESIAN_POINT ( 'NONE',  ( 31.21601485855876135, -7.209453229046482114, 166.7695841591225587 ) ) ;
#23347 = VECTOR ( 'NONE', #30998, 1000.000000000000000 ) ;
#23348 =( BOUNDED_CURVE ( )  B_SPLINE_CURVE ( 2, ( #13406, #14149, #24955, #36513, #22134, #7720, #27990 ),
 .UNSPECIFIED., .F., .F. ) 
 B_SPLINE_CURVE_WITH_KNOTS ( ( 3, 2, 2, 3 ),
 ( 0.6521739130434790477, 0.6594202898550725056, 0.6666666666666657415, 0.6739130434782591994 ),
 .UNSPECIFIED. ) 
 CURVE ( )  GEOMETRIC_REPRESENTATION_ITEM ( )  RATIONAL_B_SPLINE_CURVE ( ( 0.9999999999999856781, 0.8660254037844530295, 1.000000000000000000, 0.8660254037844387076, 1.000000000000000000, 0.8660254037844694608, 0.9999999999999692468 ) ) 
 REPRESENTATION_ITEM ( '' )  );
#23349 = CARTESIAN_POINT ( 'NONE',  ( -31.78794563604516554, 205.3262412349647832, 4.842901733360250205 ) ) ;
#23350 = CARTESIAN_POINT ( 'NONE',  ( 18.12178482187499640, 248.7718750006145001, -4.985214923628404904 ) ) ;
#23351 = FACE_OUTER_BOUND ( 'NONE', #36983, .T. ) ;
#23352 = CARTESIAN_POINT ( 'NONE',  ( -55.53794563604517975, 206.7903428501025758, 3.378800118222471838 ) ) ;
#23353 = CARTESIAN_POINT ( 'NONE',  ( -37.33705436395490551, 205.3262412349647263, -4.842901733360204020 ) ) ;
#23354 = CARTESIAN_POINT ( 'NONE',  ( 37.64990212795299840, 3.604726614523238837, 168.6723244366126551 ) ) ;
#23355 = VERTEX_POINT ( 'NONE', #1044 ) ;
#23356 = CARTESIAN_POINT ( 'NONE',  ( -28.88880888891164744, 202.4104480656949079, 2.583632243664814254 ) ) ;
#23357 = CARTESIAN_POINT ( 'NONE',  ( -14.25334919248795096, 15.11481371789854933, 6.092822981423662299 ) ) ;
#23358 = CARTESIAN_POINT ( 'NONE',  ( -60.88913769728824121, 205.8500491399820760, -7.418979330068584233 ) ) ;
#23359 = CARTESIAN_POINT ( 'NONE',  ( 3.796722387233379514, 135.1851862821014549, -8.710071997420127943 ) ) ;
#23360 = EDGE_CURVE ( 'NONE', #36105, #5013, #6366, .T. ) ;
#23361 = CARTESIAN_POINT ( 'NONE',  ( -4.622313124798576922, 51.23518628210143788, -11.61527771782819762 ) ) ;
#23362 = EDGE_CURVE ( 'NONE', #21882, #8395, #7588, .T. ) ;
#23363 = CARTESIAN_POINT ( 'NONE',  ( 16.56230152254411081, -6.928203230275514990, -5.287500000000021849 ) ) ;
#23364 = ORIENTED_EDGE ( 'NONE', *, *, #15916, .T. ) ;
#23365 = CARTESIAN_POINT ( 'NONE',  ( -45.25372103062156270, 216.5309553116392181, -1.626142955000564383 ) ) ;
#23366 = DIRECTION ( 'NONE',  ( 1.000000000000000000, 0.000000000000000000, 0.000000000000000000 ) ) ;
#23367 = CARTESIAN_POINT ( 'NONE',  ( 5.529263428287477744, 25.07268628210145067, -7.954856959092191815 ) ) ;
#23368 = CARTESIAN_POINT ( 'NONE',  ( -27.24356964375000345, 196.7093750006145569, 0.000000000000000000 ) ) ;
#23369 = DIRECTION ( 'NONE',  ( 0.9961946980917462113, 0.000000000000000000, -0.08715574274765118534 ) ) ;
#23370 = DIRECTION ( 'NONE',  ( -0.000000000000000000, 1.000000000000000000, -0.000000000000000000 ) ) ;
#23371 = CARTESIAN_POINT ( 'NONE',  ( 7.234628195640295800, 197.4325961894323882, 27.00000000000001066 ) ) ;
#23372 = CARTESIAN_POINT ( 'NONE',  ( 37.30839204460733782, 7.347880794884117764E-16, 167.5634945697888440 ) ) ;
#23373 = EDGE_CURVE ( 'NONE', #1338, #21070, #29858, .T. ) ;
#23374 = CARTESIAN_POINT ( 'NONE',  ( 15.24356964374999990, 244.4593750006145569, 0.000000000000000000 ) ) ;
#23375 = CARTESIAN_POINT ( 'NONE',  ( -8.710071997420207879, 88.71481371789855075, 3.796722387233182339 ) ) ;
#23376 = LINE ( 'NONE', #15033, #12501 ) ;
#23377 = ORIENTED_EDGE ( 'NONE', *, *, #7286, .F. ) ;
#23378 = CARTESIAN_POINT ( 'NONE',  ( -57.52455436395488420, 205.1570982666397356, 4.673758765035198159 ) ) ;
#23379 = CARTESIAN_POINT ( 'NONE',  ( 26.99999999999999645, 246.7187500012290400, -3.464101615137755275 ) ) ;
#23380 = CARTESIAN_POINT ( 'NONE',  ( -8.715434833792127023, 97.33981371789855075, 8.962234695871568846 ) ) ;
#23381 = CARTESIAN_POINT ( 'NONE',  ( 10.31873187879410558, 0.000000000000000000, -1.546874999385550176 ) ) ;
#23382 = CARTESIAN_POINT ( 'NONE',  ( 27.48022219281702405, -5.407089921784859143, 159.8877424583000391 ) ) ;
#23383 = CARTESIAN_POINT ( 'NONE',  ( 26.75643035624999655, -3.323476615752267715, -2.765624999385494220 ) ) ;
#23384 = CARTESIAN_POINT ( 'NONE',  ( -10.69584247140429412, 71.75231371789855928, -6.932735513424201024 ) ) ;
#23385 = CARTESIAN_POINT ( 'NONE',  ( -27.24356964374999990, 197.1218750006145228, -15.72908226750537786 ) ) ;
#23386 = EDGE_LOOP ( 'NONE', ( #16126, #35261, #20165, #32798 ) ) ;
#23387 = VERTEX_POINT ( 'NONE', #23430 ) ;
#23388 = ORIENTED_EDGE ( 'NONE', *, *, #27471, .F. ) ;
#23389 = CARTESIAN_POINT ( 'NONE',  ( 15.24356964375000167, -3.323476615752272600, -4.153124999385478411 ) ) ;
#23390 = CARTESIAN_POINT ( 'NONE',  ( -13.50000000000000533, 195.4250000000000114, -23.38268590217984411 ) ) ;
#23391 =( BOUNDED_CURVE ( )  B_SPLINE_CURVE ( 2, ( #20104, #35049, #22951, #11931, #14598, #8722, #8905 ),
 .UNSPECIFIED., .F., .F. ) 
 B_SPLINE_CURVE_WITH_KNOTS ( ( 3, 2, 2, 3 ),
 ( 0.5217391304347818171, 0.5289855072463759411, 0.5362318840579700652, 0.5434782608695640782 ),
 .UNSPECIFIED. ) 
 CURVE ( )  GEOMETRIC_REPRESENTATION_ITEM ( )  RATIONAL_B_SPLINE_CURVE ( ( 1.000000000000014433, 0.8660254037844243857, 1.000000000000000000, 0.8660254037844387076, 1.000000000000000000, 0.8660254037844592467, 0.9999999999999794609 ) ) 
 REPRESENTATION_ITEM ( '' )  );
#23392 = CARTESIAN_POINT ( 'NONE',  ( 21.00000000000000000, 247.6093750006145342, 6.646953231504538984 ) ) ;
#23393 = AXIS2_PLACEMENT_3D ( 'NONE', #34, #34718, #16743 ) ;
#23394 = CARTESIAN_POINT ( 'NONE',  ( 10.49813415415989581, 45.77268628210144641, 7.228626920339068285 ) ) ;
#23395 = CARTESIAN_POINT ( 'NONE',  ( -49.40252896937850124, 206.6499508600178387, -5.571401726697954970 ) ) ;
#23396 = CARTESIAN_POINT ( 'NONE',  ( 15.84454946586586566, 211.9332939502924660, -5.693556627489360089 ) ) ;
#23397 = CARTESIAN_POINT ( 'NONE',  ( -67.21502896937850835, 215.5714017266979567, -3.350049139982168800 ) ) ;
#23398 = CARTESIAN_POINT ( 'NONE',  ( 30.75272761356932705, 6.928203230275506996, 161.4741867176907988 ) ) ;
#23399 = CARTESIAN_POINT ( 'NONE',  ( 4.622313124798831829, 101.3648137178985564, -11.61527771782809282 ) ) ;
#23400 = CARTESIAN_POINT ( 'NONE',  ( -54.75372103062156270, 214.5309553116392749, -1.090244570138262148 ) ) ;
#23401 = CARTESIAN_POINT ( 'NONE',  ( -33.57663769728823411, 202.5810206699313767, 4.149950860017909804 ) ) ;
#23402 = CARTESIAN_POINT ( 'NONE',  ( 15.24356964374999990, 3.323476615752268604, -3.440624999385503813 ) ) ;
#23403 = CARTESIAN_POINT ( 'NONE',  ( 26.99999999999999645, 7.347880794884117764E-16, -0.6750000000000089262 ) ) ;
#23404 = CARTESIAN_POINT ( 'NONE',  ( 15.53471296425188797, 75.77731371789855075, 2.908627838312457747 ) ) ;
#23405 = CARTESIAN_POINT ( 'NONE',  ( -61.47544563604516554, 216.3070033484980854, 6.137860380172893926 ) ) ;
#23406 = ORIENTED_EDGE ( 'NONE', *, *, #15154, .F. ) ;
#23407 = DIRECTION ( 'NONE',  ( 1.000000000000000000, 0.000000000000000000, 0.000000000000000000 ) ) ;
#23408 = CARTESIAN_POINT ( 'NONE',  ( 10.49813415415989581, 100.9726862821014635, 7.228626920339068285 ) ) ;
#23409 = CARTESIAN_POINT ( 'NONE',  ( -14.25334919248782306, 50.08518628210143930, -6.092822981423979378 ) ) ;
#23410 = CARTESIAN_POINT ( 'NONE',  ( 18.00000000000000000, 5.196152422706630247, -5.868749998770961263 ) ) ;
#23411 = CARTESIAN_POINT ( 'NONE',  ( 24.47653776615555898, 0.000000000000000000, 161.3739362214482469 ) ) ;
#23412 = CARTESIAN_POINT ( 'NONE',  ( 13.04141134922759804, 73.37268628210144072, 8.927990412390657937 ) ) ;
#23413 = AXIS2_PLACEMENT_3D ( 'NONE', #13427, #7372, #36348 ) ;
#23414 = LINE ( 'NONE', #8137, #6040 ) ;
#23415 = CARTESIAN_POINT ( 'NONE',  ( 16.56230152254411081, 7.209453229046475009, -9.703124999385542182 ) ) ;
#23416 = CARTESIAN_POINT ( 'NONE',  ( -46.24330436395489841, 210.1155267958017134, -6.500000000000000888 ) ) ;
#23417 = CARTESIAN_POINT ( 'NONE',  ( 20.99999999999999645, 185.0294372515228645, -5.999999999999999112 ) ) ;
#23418 = CARTESIAN_POINT ( 'NONE',  ( -11.48171059495397373, 40.88518628210144357, -4.944772684328680334 ) ) ;
#23419 = CARTESIAN_POINT ( 'NONE',  ( 13.50000000000001421, 196.1000000000000227, 23.38268590217984055 ) ) ;
#23420 = CARTESIAN_POINT ( 'NONE',  ( 19.95811783012821650, 240.0005236131589754, -5.908847734042844912 ) ) ;
#23421 = CARTESIAN_POINT ( 'NONE',  ( 3.474262827703335166, 9.835186282101449962, 8.843639120294326972 ) ) ;
#23422 = CARTESIAN_POINT ( 'NONE',  ( 23.87821517812499650, 245.6593750006145171, -4.985214923628404904 ) ) ;
#23423 = ORIENTED_EDGE ( 'NONE', *, *, #12715, .F. ) ;
#23424 = CARTESIAN_POINT ( 'NONE',  ( 18.00000000000000000, 5.196152422706630247, -7.725000000000009415 ) ) ;
#23425 = CARTESIAN_POINT ( 'NONE',  ( 26.99999999999999645, 243.4375000000000284, 3.464101615137751278 ) ) ;
#23426 = FACE_OUTER_BOUND ( 'NONE', #16593, .T. ) ;
#23427 = CARTESIAN_POINT ( 'NONE',  ( 16.56230152254411081, 7.209453229046475009, -3.403124999385538807 ) ) ;
#23428 = CARTESIAN_POINT ( 'NONE',  ( 37.36882485759181804, -3.604726614523235284, 165.4595965352667690 ) ) ;
#23429 = CARTESIAN_POINT ( 'NONE',  ( 18.00000000000000355, 240.1750000000000114, 5.196152422706632912 ) ) ;
#23430 = CARTESIAN_POINT ( 'NONE',  ( 22.56230152254410015, 7.347880794884117764E-16, -8.212499998771022547 ) ) ;
#23431 = CARTESIAN_POINT ( 'NONE',  ( 2.660918448318279950, 70.49768628210145494, -12.46528703574805874 ) ) ;
#23432 = ORIENTED_EDGE ( 'NONE', *, *, #3926, .T. ) ;
#23433 = ORIENTED_EDGE ( 'NONE', *, *, #36224, .F. ) ;
#23434 = CARTESIAN_POINT ( 'NONE',  ( 36.94233792496062563, -3.464101615137448409, 163.3794768365791015 ) ) ;
#23435 = CARTESIAN_POINT ( 'NONE',  ( -79.65000000000001990, 210.0000000000000000, 5.000000000000000000 ) ) ;
#23436 = CARTESIAN_POINT ( 'NONE',  ( 10.31873187879411091, 0.000000000000000000, -0.1406249993855246405 ) ) ;
#23437 = CARTESIAN_POINT ( 'NONE',  ( 26.75643035624999655, 7.049594010296217766E-16, -7.565624999385455851 ) ) ;
#23438 = CARTESIAN_POINT ( 'NONE',  ( -11.08355503943118592, 44.43981371789855928, -10.83675517735179383 ) ) ;
#23439 = CARTESIAN_POINT ( 'NONE',  ( -38.47274018782780303, 246.3803829651731121, 5.000000000000000000 ) ) ;
#23440 = CARTESIAN_POINT ( 'NONE',  ( 26.75643035624999655, 241.0843750006145285, -7.049594010296217766E-16 ) ) ;
#23441 = CARTESIAN_POINT ( 'NONE',  ( -65.82961230271185116, 211.3212981617417938, 4.469044688360757966 ) ) ;
#23442 = VECTOR ( 'NONE', #28284, 1000.000000000000000 ) ;
#23443 = CARTESIAN_POINT ( 'NONE',  ( 16.56230152254410726, 0.000000000000000000, -10.00000000000000000 ) ) ;
#23444 = CARTESIAN_POINT ( 'NONE',  ( 27.51453976652391376, -5.407089921784865361, 160.2799941206736776 ) ) ;
#23445 = CARTESIAN_POINT ( 'NONE',  ( -9.534712964251895073, 25.17731371789854933, -1.715153634034446428 ) ) ;
#23446 = CARTESIAN_POINT ( 'NONE',  ( -64.84747103062156270, 213.3500491399821328, -5.571401726697985168 ) ) ;
#23447 = CARTESIAN_POINT ( 'NONE',  ( -45.64211230271183695, 201.5309553116392181, 2.393094931466368980 ) ) ;
#23448 = DIRECTION ( 'NONE',  ( 1.000000000000000000, 0.000000000000000000, 0.000000000000000000 ) ) ;
#23449 = CARTESIAN_POINT ( 'NONE',  ( 18.39679865110830548, 195.0000000000000284, -19.80091321147607886 ) ) ;
#23450 = CARTESIAN_POINT ( 'NONE',  ( 13.62178482187499640, 196.1093750006145342, -23.59362340125807123 ) ) ;
#23451 = CARTESIAN_POINT ( 'NONE',  ( 2.908627838312458636, 128.6773137178985280, -15.53471296425188442 ) ) ;
#23452 = CARTESIAN_POINT ( 'NONE',  ( -53.16294563604517265, 214.6737587650350747, -4.842901733360249317 ) ) ;
#23453 = ORIENTED_EDGE ( 'NONE', *, *, #4065, .F. ) ;
#23454 = CARTESIAN_POINT ( 'NONE',  ( 8.962234695871762469, 52.96018628210144641, -8.715434833791931624 ) ) ;
#23455 = CARTESIAN_POINT ( 'NONE',  ( -49.64999999999999858, 244.5000000000000000, 5.000000000000000000 ) ) ;
#23456 = CARTESIAN_POINT ( 'NONE',  ( 15.00000000000000000, 0.000000000000000000, -1.293749998770965526 ) ) ;
#23457 = CARTESIAN_POINT ( 'NONE',  ( 37.64173127707041289, 7.646167579472024665E-16, 168.5789311836665831 ) ) ;
#23458 = CARTESIAN_POINT ( 'NONE',  ( 15.00000000000000178, -3.464101615137757051, -1.706249998770944964 ) ) ;
#23459 = CARTESIAN_POINT ( 'NONE',  ( 19.68408634441912142, -5.407089921784861808, -7.696874999385511451 ) ) ;
#23460 = CARTESIAN_POINT ( 'NONE',  ( -66.03497103062157692, 204.4285982733020148, -3.350049139982115509 ) ) ;
#23461 = CARTESIAN_POINT ( 'NONE',  ( 10.31873187879411269, -3.604726614523240613, -1.003124999385540450 ) ) ;
#23462 = CARTESIAN_POINT ( 'NONE',  ( -6.840914352312096547, 57.56018628210145494, 6.594114490232313663 ) ) ;
#23463 = DIRECTION ( 'NONE',  ( 0.9961946980917462113, 0.000000000000000000, -0.08715574274765118534 ) ) ;
#23464 = CYLINDRICAL_SURFACE ( 'NONE', #8659, 27.00000000000000000 ) ;
#23465 = CARTESIAN_POINT ( 'NONE',  ( -11.48171059495397373, 96.08518628210146062, -4.944772684328680334 ) ) ;
#23466 = CARTESIAN_POINT ( 'NONE',  ( 27.00000000000000355, 199.4375000012290400, -3.306546357697854128E-15 ) ) ;
#23467 = CARTESIAN_POINT ( 'NONE',  ( 20.99999999999999645, 0.000000000000000000, -8.000000000000000000 ) ) ;
#23468 = ORIENTED_EDGE ( 'NONE', *, *, #37375, .F. ) ;
#23469 = CARTESIAN_POINT ( 'NONE',  ( 24.40300010821222898, 0.000000000000000000, 160.5333969449332869 ) ) ;
#23470 = CARTESIAN_POINT ( 'NONE',  ( 23.87821517812500005, -4.985214923628404016, -8.540624999385460825 ) ) ;
#23471 = CARTESIAN_POINT ( 'NONE',  ( 7.234628195640269155, 196.0825961894323939, 27.00000000000003197 ) ) ;
#23472 = CARTESIAN_POINT ( 'NONE',  ( 31.01991443737654208, -7.209453229046482114, 164.5281460884161504 ) ) ;
#23473 = CARTESIAN_POINT ( 'NONE',  ( 36.94887460566616966, 3.464101615137759271, 163.4541914389360215 ) ) ;
#23474 = CARTESIAN_POINT ( 'NONE',  ( 26.99999999999999645, 196.6625000000000512, -15.58845726811990495 ) ) ;
#23475 = CARTESIAN_POINT ( 'NONE',  ( 18.00000000000000355, 247.8249999999999886, 5.196152422706632912 ) ) ;
#23476 = CARTESIAN_POINT ( 'NONE',  ( 27.24356964375000345, 198.6781250006145569, -3.336375036156643733E-15 ) ) ;
#23477 = CARTESIAN_POINT ( 'NONE',  ( -0.1745138560722763466, 109.9898137178985706, -12.50000000000000355 ) ) ;
#23478 = CARTESIAN_POINT ( 'NONE',  ( -6.932735513423968321, 115.3476862821014635, -10.69584247140445221 ) ) ;
#23479 = AXIS2_PLACEMENT_3D ( 'NONE', #31706, #5734, #14462 ) ;
#23481 = ORIENTED_EDGE ( 'NONE', *, *, #22553, .T. ) ;
#23480 = ORIENTED_EDGE ( 'NONE', *, *, #581, .T. ) ;
#23482 = CARTESIAN_POINT ( 'NONE',  ( 13.62178482187499640, 196.9531250006145342, -23.59362340125807123 ) ) ;
#23483 = CARTESIAN_POINT ( 'NONE',  ( 15.24356964374999990, 242.9968750006145228, 0.000000000000000000 ) ) ;
#23484 = CARTESIAN_POINT ( 'NONE',  ( 11.08355503943118769, 85.83981371789856496, 10.83675517735179028 ) ) ;
#23485 = EDGE_CURVE ( 'NONE', #4869, #7912, #35710, .T. ) ;
#23486 = CARTESIAN_POINT ( 'NONE',  ( 26.75643035624999655, 7.049594010296217766E-16, -3.628124999385473615 ) ) ;
#23487 = CARTESIAN_POINT ( 'NONE',  ( 15.24356964374999990, 246.6718750006145342, -3.323476615752268604 ) ) ;
#23488 = CARTESIAN_POINT ( 'NONE',  ( 27.00000000000000355, 196.7375000012290229, -3.306546357697854128E-15 ) ) ;
#23489 = CARTESIAN_POINT ( 'NONE',  ( -5.529263428287297444, 72.32731371789854791, -7.954856959092311719 ) ) ;
#23490 = CARTESIAN_POINT ( 'NONE',  ( 16.56230152254411436, 7.209453229046475009, -4.753124999385526017 ) ) ;
#23491 = ADVANCED_FACE ( 'NONE', ( #9587 ), #18813, .F. ) ;
#23492 = AXIS2_PLACEMENT_3D ( 'NONE', #7112, #10313, #18683 ) ;
#23493 = CARTESIAN_POINT ( 'NONE',  ( 23.87821517812500005, 241.7968750006145342, 4.985214923628404016 ) ) ;
#23494 = CARTESIAN_POINT ( 'NONE',  ( -8.962234695871565293, 44.43981371789855217, -8.715434833792128799 ) ) ;
#23495 = CARTESIAN_POINT ( 'NONE',  ( 22.56230152254410370, 7.347880794884117764E-16, -1.462499998771016330 ) ) ;
#23496 = CARTESIAN_POINT ( 'NONE',  ( -4.944772684328673229, 102.9851862821014663, 11.48171059495397728 ) ) ;
#23497 = CARTESIAN_POINT ( 'NONE',  ( 19.56230152254411081, -5.196152422706629359, -5.587499998771034093 ) ) ;
#23498 = ADVANCED_FACE ( 'NONE', ( #6635 ), #18396, .F. ) ;
#23499 = CARTESIAN_POINT ( 'NONE',  ( -65.63913769728821990, 207.8500491399821613, -3.954877714930864485 ) ) ;
#23500 = CARTESIAN_POINT ( 'NONE',  ( 15.00000000000031797, 3.464101615137936019, -7.181249998770955045 ) ) ;
#23501 = CARTESIAN_POINT ( 'NONE',  ( 36.67106567565804198, 7.347880794884125653E-16, 160.2788208387686097 ) ) ;
#23502 = VECTOR ( 'NONE', #9444, 1000.000000000000000 ) ;
#23503 = CARTESIAN_POINT ( 'NONE',  ( -3.257655550457281723, 75.09768628210143504, 15.46528703574804986 ) ) ;
#23504 = EDGE_CURVE ( 'NONE', #7705, #483, #36931, .T. ) ;
#23505 = CARTESIAN_POINT ( 'NONE',  ( -6.932735513423968321, 4.947686282101432020, -10.69584247140445221 ) ) ;
#23506 = CARTESIAN_POINT ( 'NONE',  ( 26.99999999999999645, 7.347880794884117764E-16, -0.2250000000000029754 ) ) ;
#23507 = CARTESIAN_POINT ( 'NONE',  ( 5.233372021372432847, 119.9476862821014294, 8.152565276336710909 ) ) ;
#23508 = CARTESIAN_POINT ( 'NONE',  ( 7.234628195640322446, 198.8950961906613770, 26.99999999999999645 ) ) ;
#23509 = ADVANCED_FACE ( 'NONE', ( #375 ), #28033, .F. ) ;
#23510 = CARTESIAN_POINT ( 'NONE',  ( -3.257655550457281723, 19.89768628210143930, 15.46528703574804986 ) ) ;
#23511 = CARTESIAN_POINT ( 'NONE',  ( 4.999999999999997335, 216.0000000000000000, 7.347880794884120722E-16 ) ) ;
#23512 = CARTESIAN_POINT ( 'NONE',  ( 23.87821517812500005, 242.2468750006145228, 4.985214923628404016 ) ) ;
#23513 = EDGE_LOOP ( 'NONE', ( #1911, #3322, #1421, #35854 ) ) ;
#23514 = CARTESIAN_POINT ( 'NONE',  ( 37.64990212795299129, 3.604726614523238837, 168.6723244366126551 ) ) ;
#23515 = CARTESIAN_POINT ( 'NONE',  ( 6.594114490232313663, 36.86018628210144499, 6.840914352312096547 ) ) ;
#23516 = CARTESIAN_POINT ( 'NONE',  ( 18.12178482187500350, -4.985214923628407568, -1.415624999385467486 ) ) ;
#23517 = CARTESIAN_POINT ( 'NONE',  ( 24.00000000000000000, 241.6000000000000227, 5.196152422706629359 ) ) ;
#23518 = CARTESIAN_POINT ( 'NONE',  ( 22.46128102716605923, 1.096376214649937619, -10.00000000000000000 ) ) ;
#23519 = LINE ( 'NONE', #32792, #11223 ) ;
#23520 = CARTESIAN_POINT ( 'NONE',  ( -1.057942093924267191, 194.9999999999999432, 27.27867916801710635 ) ) ;
#23521 = CARTESIAN_POINT ( 'NONE',  ( 26.99999999999999645, 198.9125000000000512, -15.58845726811990495 ) ) ;
#23522 = CARTESIAN_POINT ( 'NONE',  ( -0.1745138560723084320, 36.38981371789855501, -9.500000000000005329 ) ) ;
#23523 = CARTESIAN_POINT ( 'NONE',  ( 27.24356964375000700, 199.1468750006145285, 15.72908226750537075 ) ) ;
#23524 = AXIS2_PLACEMENT_3D ( 'NONE', #15872, #15493, #4295 ) ;
#23525 = ORIENTED_EDGE ( 'NONE', *, *, #26065, .F. ) ;
#23526 = CARTESIAN_POINT ( 'NONE',  ( 15.00000000000000000, 240.1562500012290684, 0.000000000000000000 ) ) ;
#23527 = CARTESIAN_POINT ( 'NONE',  ( -7.228626920338836470, 44.72731371789855359, -10.49813415416005213 ) ) ;
#23528 = CARTESIAN_POINT ( 'NONE',  ( 15.24356964374999990, 0.000000000000000000, -8.353124999385480365 ) ) ;
#23529 = CARTESIAN_POINT ( 'NONE',  ( 11.48171059495408208, 10.51481371789855856, -4.944772684328420986 ) ) ;
#23530 = DIRECTION ( 'NONE',  ( 0.000000000000000000, 0.000000000000000000, 1.000000000000000000 ) ) ;
#23531 = ORIENTED_EDGE ( 'NONE', *, *, #32387, .F. ) ;
#23532 = CARTESIAN_POINT ( 'NONE',  ( 22.80587116629411781, -3.604726614523238837, -4.509374999385530103 ) ) ;
#23533 = ORIENTED_EDGE ( 'NONE', *, *, #16238, .F. ) ;
#23534 = CARTESIAN_POINT ( 'NONE',  ( -1.926257025242585782E-15, 198.3406250006145228, -31.45816453501075927 ) ) ;
#23535 = EDGE_CURVE ( 'NONE', #12454, #29192, #13927, .T. ) ;
#23536 = CARTESIAN_POINT ( 'NONE',  ( 31.15718473220409379, 7.209453229046482114, 166.0971527379105908 ) ) ;
#23537 = EDGE_CURVE ( 'NONE', #37311, #26963, #26523, .T. ) ;
#23538 = CARTESIAN_POINT ( 'NONE',  ( -32.38169563604517265, 210.1155267958017703, 6.500000000000000888 ) ) ;
#23539 = FILL_AREA_STYLE ('',( #18429 ) ) ;
#23540 = CARTESIAN_POINT ( 'NONE',  ( 0.000000000000000000, 148.0000000000000000, 0.000000000000000000 ) ) ;
#23541 = EDGE_CURVE ( 'NONE', #34897, #18997, #36339, .T. ) ;
#23542 = CARTESIAN_POINT ( 'NONE',  ( -61.87127896937851546, 214.5309553116392749, 1.090244570138288127 ) ) ;
#23543 = CARTESIAN_POINT ( 'NONE',  ( 25.06317337608639306, -3.464101615137925805, 165.2845636778794187 ) ) ;
#23544 = CARTESIAN_POINT ( 'NONE',  ( 28.32999068460662428, 5.407089921784856479, 169.6006407646945604 ) ) ;
#23545 = ORIENTED_EDGE ( 'NONE', *, *, #12616, .T. ) ;
#23546 = CARTESIAN_POINT ( 'NONE',  ( 25.32464060422194052, 0.000000000000000000, 168.2731477709303363 ) ) ;
#23547 = CARTESIAN_POINT ( 'NONE',  ( 3.257655550456945548, 13.10231371789855181, 15.46528703574811736 ) ) ;
#23548 = CARTESIAN_POINT ( 'NONE',  ( -56.13913769728823411, 205.8500491399820760, -7.418979330068584233 ) ) ;
#23549 = EDGE_CURVE ( 'NONE', #30233, #25013, #30134, .T. ) ;
#23550 = CARTESIAN_POINT ( 'NONE',  ( -8.710071997420127943, 132.8851862821014436, -3.796722387233380402 ) ) ;
#23551 =( BOUNDED_CURVE ( )  B_SPLINE_CURVE ( 2, ( #26514, #15534, #32579, #544, #15343, #26897, #21416 ),
 .UNSPECIFIED., .F., .F. ) 
 B_SPLINE_CURVE_WITH_KNOTS ( ( 3, 2, 2, 3 ),
 ( 0.2391304347826081200, 0.2463768115942023829, 0.2536231884057966179, 0.2608695652173908530 ),
 .UNSPECIFIED. ) 
 CURVE ( )  GEOMETRIC_REPRESENTATION_ITEM ( )  RATIONAL_B_SPLINE_CURVE ( ( 1.000000000000010658, 0.8660254037844279384, 1.000000000000000000, 0.8660254037844387076, 1.000000000000000000, 0.8660254037844469233, 0.9999999999999917843 ) ) 
 REPRESENTATION_ITEM ( '' )  );
#23552 = CARTESIAN_POINT ( 'NONE',  ( 7.228626920339068285, 25.07268628210144712, -10.49813415415989581 ) ) ;
#23553 = CARTESIAN_POINT ( 'NONE',  ( 10.56230152254411259, -3.464101615137761048, -5.362500000000047784 ) ) ;
#23554 = ORIENTED_EDGE ( 'NONE', *, *, #20519, .F. ) ;
#23555 = CARTESIAN_POINT ( 'NONE',  ( -38.72247103062156981, 206.6499508600178672, 5.571401726697986057 ) ) ;
#23556 = CARTESIAN_POINT ( 'NONE',  ( 13.56230152254410370, 5.196152422706630247, -5.362499998771003362 ) ) ;
#23557 = CARTESIAN_POINT ( 'NONE',  ( -5.233372021372430183, 23.34768628210144570, -8.152565276336710909 ) ) ;
#23558 = CARTESIAN_POINT ( 'NONE',  ( 13.62178482187501416, 195.5093750006145399, 23.59362340125806767 ) ) ;
#23559 = CARTESIAN_POINT ( 'NONE',  ( 5.438367727407757144E-14, 198.2000000012290002, -27.00000000000000000 ) ) ;
#23560 = CARTESIAN_POINT ( 'NONE',  ( -13.49999999999998401, 198.7250000000000227, 23.38268590217985476 ) ) ;
#23561 = DIRECTION ( 'NONE',  ( 0.000000000000000000, 0.000000000000000000, 1.000000000000000000 ) ) ;
#23562 = CARTESIAN_POINT ( 'NONE',  ( 31.41946904558886544, 6.928203230275506996, 169.0950761580926383 ) ) ;
#23563 = CARTESIAN_POINT ( 'NONE',  ( 23.87821517812499650, 245.6593750006145171, -4.985214923628404904 ) ) ;
#23564 = CARTESIAN_POINT ( 'NONE',  ( 9.465287035748106703, 93.60231371789855359, -2.064181346179063237 ) ) ;
#23565 = CARTESIAN_POINT ( 'NONE',  ( 18.12178482187499640, 240.3343750006145285, -4.985214923628404904 ) ) ;
#23566 = ORIENTED_EDGE ( 'NONE', *, *, #14456, .T. ) ;
#23567 = CARTESIAN_POINT ( 'NONE',  ( -52.18080436395490551, 203.5000000000000000, -0.1155267958017335561 ) ) ;
#23568 = CARTESIAN_POINT ( 'NONE',  ( 26.99999999999999645, 246.2312500012290570, -7.347880794884117764E-16 ) ) ;
#23569 = CARTESIAN_POINT ( 'NONE',  ( -12.46528703574811558, 107.4023137178985650, 2.660918448318004170 ) ) ;
#23570 = CARTESIAN_POINT ( 'NONE',  ( 22.80587116629411426, 7.646167579472024665E-16, -2.221874999385531346 ) ) ;
#23571 = CARTESIAN_POINT ( 'NONE',  ( 36.90472052746056875, 3.604726614523238837, 160.1548597679282295 ) ) ;
#23572 = CARTESIAN_POINT ( 'NONE',  ( 26.75643035624999655, 7.049594010296217766E-16, -1.378124999385471616 ) ) ;
#23573 = CARTESIAN_POINT ( 'NONE',  ( 12.50000000000000355, 75.48981371789855643, -0.1745138560722771515 ) ) ;
#23574 = CARTESIAN_POINT ( 'NONE',  ( 13.62178482187499640, 198.8093750006145513, -23.59362340125807123 ) ) ;
#23575 = ORIENTED_EDGE ( 'NONE', *, *, #29347, .F. ) ;
#23576 =( BOUNDED_CURVE ( )  B_SPLINE_CURVE ( 2, ( #29488, #17943, #12434, #32706, #20602, #11866, #26834, #6371, #23625 ),
 .UNSPECIFIED., .F., .F. ) 
 B_SPLINE_CURVE_WITH_KNOTS ( ( 3, 2, 2, 2, 3 ),
 ( 0.3152173913043477826, 0.3188405797101449002, 0.3260869565217391353, 0.3333333333333333148, 0.3369565217391304324 ),
 .UNSPECIFIED. ) 
 CURVE ( )  GEOMETRIC_REPRESENTATION_ITEM ( )  RATIONAL_B_SPLINE_CURVE ( ( 0.9330127018922191873, 0.9330127018922187432, 1.000000000000000000, 0.8660254037844387076, 1.000000000000000000, 0.8660254037844387076, 1.000000000000000000, 0.9330127018922194093, 0.9330127018922194093 ) ) 
 REPRESENTATION_ITEM ( '' )  );
#23577 = ORIENTED_EDGE ( 'NONE', *, *, #17015, .F. ) ;
#23578 = CARTESIAN_POINT ( 'NONE',  ( 23.87821517812499650, 4.985214923628404904, -5.240624999385462779 ) ) ;
#23579 = CARTESIAN_POINT ( 'NONE',  ( 37.02404643378602600, 7.347880794884125653E-16, 164.3134093660401618 ) ) ;
#23580 = CARTESIAN_POINT ( 'NONE',  ( 18.12178482187500350, 247.5718750006145115, 4.985214923628407568 ) ) ;
#23581 = CARTESIAN_POINT ( 'NONE',  ( -12.53471296425194836, 40.02268628210143930, 2.311890736173176641 ) ) ;
#23582 = EDGE_CURVE ( 'NONE', #33833, #1210, #11900, .T. ) ;
#23583 = CARTESIAN_POINT ( 'NONE',  ( -45.84002896937850124, 204.4285982733020433, 3.350049139982171020 ) ) ;
#23584 =( NAMED_UNIT ( * ) PLANE_ANGLE_UNIT ( ) SI_UNIT ( $, .RADIAN. ) );
#23585 = CARTESIAN_POINT ( 'NONE',  ( -67.61086230271183695, 213.1499508600178387, -5.686928522499747451 ) ) ;
#23586 = CARTESIAN_POINT ( 'NONE',  ( 27.72819177541068214, 5.196152422706630247, 161.3247236329709153 ) ) ;
#23587 = CARTESIAN_POINT ( 'NONE',  ( 2.311890736173452865, 101.0773137178985621, -12.53471296425189152 ) ) ;
#23588 = CARTESIAN_POINT ( 'NONE',  ( -57.12872103062156270, 205.4690446883607535, 1.090244570138264368 ) ) ;
#23589 = CARTESIAN_POINT ( 'NONE',  ( -66.43080436395490551, 203.5000000000000000, -0.1155267958017335561 ) ) ;
#23590 = CARTESIAN_POINT ( 'NONE',  ( 15.24356964374999990, 0.000000000000000000, -7.453124999385495997 ) ) ;
#23591 = CARTESIAN_POINT ( 'NONE',  ( 26.99999999999999289, 0.000000000000000000, -8.000000000000000000 ) ) ;
#23592 = CARTESIAN_POINT ( 'NONE',  ( -15.53471296425188442, 71.17731371789855643, -2.908627838312459080 ) ) ;
#23593 = CARTESIAN_POINT ( 'NONE',  ( -63.85044563604516554, 203.6929966515019430, -6.137860380172892150 ) ) ;
#23594 = ORIENTED_EDGE ( 'NONE', *, *, #36699, .T. ) ;
#23595 = CARTESIAN_POINT ( 'NONE',  ( -6.422845572874366304, 142.9999999999996305, 10.72508787064079172 ) ) ;
#23596 = CARTESIAN_POINT ( 'NONE',  ( -12.46528703574805697, 95.79768628210143788, -2.660918448318280838 ) ) ;
#23597 = CARTESIAN_POINT ( 'NONE',  ( -2.908627838312119351, 51.52268628210144641, -15.53471296425195369 ) ) ;
#23598 = CARTESIAN_POINT ( 'NONE',  ( 24.43731768191911513, 0.000000000000000000, 160.9256486073069539 ) ) ;
#23599 = CARTESIAN_POINT ( 'NONE',  ( 8.632099005475504683, 64.74768628210144072, 13.23911966647218996 ) ) ;
#23600 = LINE ( 'NONE', #35145, #1826 ) ;
#23601 = CARTESIAN_POINT ( 'NONE',  ( 19.68408634441910721, 5.407089921784857367, -8.390624999385531524 ) ) ;
#23602 = FACE_OUTER_BOUND ( 'NONE', #32617, .T. ) ;
#23603 = CARTESIAN_POINT ( 'NONE',  ( -50.00372103062157692, 216.5309553116391612, -1.626142955000564383 ) ) ;
#23604 = CARTESIAN_POINT ( 'NONE',  ( 20.99999999999999289, 248.9874999999999829, -5.999999999999997335 ) ) ;
#23605 = CARTESIAN_POINT ( 'NONE',  ( 7.228626920339068285, 34.27268628210144641, -10.49813415415989581 ) ) ;
#23606 = CARTESIAN_POINT ( 'NONE',  ( -6.594114490232312775, 4.660186282101435928, -6.840914352312096547 ) ) ;
#23607 = CARTESIAN_POINT ( 'NONE',  ( 15.24356964375000167, 247.1968750006145115, 3.323476615752272600 ) ) ;
#23608 = AXIS2_PLACEMENT_3D ( 'NONE', #30696, #10591, #13823 ) ;
#23609 = VERTEX_POINT ( 'NONE', #16112 ) ;
#23610 = CARTESIAN_POINT ( 'NONE',  ( 21.00000000000000000, 6.928203230275506996, -8.212500000000009237 ) ) ;
#23611 =( BOUNDED_CURVE ( )  B_SPLINE_CURVE ( 2, ( #35859, #7814, #13308, #10092, #7627, #21662, #19202, #15978, #16345 ),
 .UNSPECIFIED., .F., .F. ) 
 B_SPLINE_CURVE_WITH_KNOTS ( ( 3, 2, 2, 2, 3 ),
 ( 0.4673913043478261087, 0.4710144927536231707, 0.4782608695652174058, 0.4855072463768115854, 0.4891304347826087029 ),
 .UNSPECIFIED. ) 
 CURVE ( )  GEOMETRIC_REPRESENTATION_ITEM ( )  RATIONAL_B_SPLINE_CURVE ( ( 0.9330127018922194093, 0.9330127018922198534, 1.000000000000000000, 0.8660254037844387076, 1.000000000000000000, 0.8660254037844387076, 1.000000000000000000, 0.9330127018922194093, 0.9330127018922194093 ) ) 
 REPRESENTATION_ITEM ( '' )  );
#23612 = FACE_OUTER_BOUND ( 'NONE', #1401, .T. ) ;
#23613 = B_SPLINE_CURVE_WITH_KNOTS ( 'NONE', 1,
 ( #29561, #21241 ),
 .UNSPECIFIED., .F., .F.,
 ( 2, 2 ),
 ( 0.000000000000000000, 1.000000000000000000 ),
 .UNSPECIFIED. ) ;
#23614 = DIRECTION ( 'NONE',  ( -4.130293990420971855E-17, 1.000000000000000000, 0.000000000000000000 ) ) ;
#23615 = CARTESIAN_POINT ( 'NONE',  ( 10.31873187879411091, 0.000000000000000000, -5.090624999385534366 ) ) ;
#23616 = CARTESIAN_POINT ( 'NONE',  ( 28.13389026342440857, 5.407089921784856479, 167.3592026939881237 ) ) ;
#23617 = CARTESIAN_POINT ( 'NONE',  ( 15.00000000000000000, 240.5125000000000171, -3.464101615137752166 ) ) ;
#23618 = EDGE_CURVE ( 'NONE', #13079, #21280, #16485, .T. ) ;
#23619 = CARTESIAN_POINT ( 'NONE',  ( 27.00000000000000355, 198.8750000000000284, -3.306546357697854128E-15 ) ) ;
#23620 = CARTESIAN_POINT ( 'NONE',  ( 4.944772684328679446, 52.38518628210145067, -11.48171059495397373 ) ) ;
#23621 = EDGE_LOOP ( 'NONE', ( #35446, #416, #1419, #6986, #24555, #17230, #22050, #16774, #19631, #1591, #12597, #30380, #20774, #5823, #8860, #22238, #28568, #20934, #34295, #30576, #19166, #16498, #1283, #3332, #33684, #14685, #32550, #27929, #6701, #30149, #25388, #1558, #32845, #24184, #13686, #33388, #33086, #23566, #33126, #37400, #18308, #3755, #11679, #7964, #33768, #22516, #13159, #32130 ) ) ;
#23622 = VERTEX_POINT ( 'NONE', #4720 ) ;
#23623 = CARTESIAN_POINT ( 'NONE',  ( 10.49999999999999467, 237.0000000000000000, 2.500000000000000000 ) ) ;
#23624 = ADVANCED_FACE ( 'NONE', ( #24449 ), #1876, .T. ) ;
#23625 = CARTESIAN_POINT ( 'NONE',  ( 21.00000000000000000, 246.5124999999999602, 5.999999999999998224 ) ) ;
#23626 = CARTESIAN_POINT ( 'NONE',  ( 15.00000000000000178, 248.2375000000000398, 3.464101615137757051 ) ) ;
#23627 = CARTESIAN_POINT ( 'NONE',  ( 18.12178482187500350, -4.985214923628407568, -6.365624999385477878 ) ) ;
#23628 = AXIS2_PLACEMENT_3D ( 'NONE', #608, #18647, #1372 ) ;
#23629 = CARTESIAN_POINT ( 'NONE',  ( -8.962234695871760692, 94.36018628210145209, 8.715434833791933400 ) ) ;
#23630 = CARTESIAN_POINT ( 'NONE',  ( -0.1745138560722442889, 17.98981371789853867, -15.50000000000000533 ) ) ;
#23631 = EDGE_CURVE ( 'NONE', #17495, #12159, #1688, .T. ) ;
#23632 = DIRECTION ( 'NONE',  ( 0.000000000000000000, 0.000000000000000000, 1.000000000000000000 ) ) ;
#23633 = CARTESIAN_POINT ( 'NONE',  ( 18.12178482187499640, 240.7843750006145171, -4.985214923628404904 ) ) ;
#23634 = CARTESIAN_POINT ( 'NONE',  ( -66.42336230271182274, 213.9548777149308023, 2.149950860017852960 ) ) ;
#23635 = DIRECTION ( 'NONE',  ( 0.000000000000000000, 0.000000000000000000, -1.000000000000000000 ) ) ;
#23636 = CARTESIAN_POINT ( 'NONE',  ( 33.74088742350031822, -5.407089921784861808, 159.8105457733328478 ) ) ;
#23637 = CARTESIAN_POINT ( 'NONE',  ( -5.233372021372612259, 14.25231371789853618, 8.152565276336593669 ) ) ;
#23638 = CARTESIAN_POINT ( 'NONE',  ( -63.06622103062156981, 211.6261429550005744, 6.530955311639227823 ) ) ;
#23639 = CARTESIAN_POINT ( 'NONE',  ( -30.00669563604516554, 209.8844732041981729, -8.500000000000003553 ) ) ;
#23640 = DIRECTION ( 'NONE',  ( 0.000000000000000000, 0.000000000000000000, 1.000000000000000000 ) ) ;
#23641 = COLOUR_RGB ( '',0.8941176470588234615, 0.8941176470588234615, 0.8941176470588234615 ) ;
#23642 = CARTESIAN_POINT ( 'NONE',  ( 27.11680205743124361, 195.0000000000000284, 0.9911108661349460336 ) ) ;
#23643 = CARTESIAN_POINT ( 'NONE',  ( 13.62178482187499640, 197.0093750006145399, -23.59362340125807123 ) ) ;
#23644 = CARTESIAN_POINT ( 'NONE',  ( 8.632099005475788900, 138.4523137178985621, -13.23911966647199812 ) ) ;
#23645 = CARTESIAN_POINT ( 'NONE',  ( -51.97544563604516554, 214.8429017333602360, 4.673758765035156415 ) ) ;
#23646 = EDGE_LOOP ( 'NONE', ( #7289, #34064 ) ) ;
#23647 = CARTESIAN_POINT ( 'NONE',  ( -6.932735513423968321, 50.94768628210144357, -10.69584247140445221 ) ) ;
#23648 = DIRECTION ( 'NONE',  ( -1.734723475976807094E-15, 0.000000000000000000, 1.000000000000000000 ) ) ;
#23649 = CARTESIAN_POINT ( 'NONE',  ( 22.74267999994772538, 5.498826287438556726, -8.000000000000001776 ) ) ;
#23650 = CARTESIAN_POINT ( 'NONE',  ( 25.10079077358561150, 3.604726614523240613, 168.5091807465304043 ) ) ;
#23651 = CARTESIAN_POINT ( 'NONE',  ( 21.00000000000000000, -6.928203230275506996, -2.531249998770942700 ) ) ;
#23652 = CARTESIAN_POINT ( 'NONE',  ( 22.80587116629410716, 7.646167579472015790E-16, -0.8156249993855335667 ) ) ;
#23653 = CARTESIAN_POINT ( 'NONE',  ( -8.843639120294326972, 67.33518628210143220, 3.474262827703335166 ) ) ;
#23654 = DIRECTION ( 'NONE',  ( -0.5887012860850802110, 0.8083506638593008775, 0.000000000000000000 ) ) ;
#23655 = CARTESIAN_POINT ( 'NONE',  ( 23.99999999999999645, 244.9000000000000057, -5.196152422706631135 ) ) ;
#23656 = CARTESIAN_POINT ( 'NONE',  ( 11.48171059495397728, 91.48518628210145209, 4.944772684328674117 ) ) ;
#23657 = CARTESIAN_POINT ( 'NONE',  ( 26.99999999999999645, 199.4750000012290343, -15.58845726811990495 ) ) ;
#23658 = CARTESIAN_POINT ( 'NONE',  ( 10.31873187879410914, 0.000000000000000000, -0.1968749993855323233 ) ) ;
#23659 = VERTEX_POINT ( 'NONE', #30322 ) ;
#23660 = CARTESIAN_POINT ( 'NONE',  ( 36.81974367828161121, -3.604726614523235284, 159.1835699372888087 ) ) ;
#23661 = CARTESIAN_POINT ( 'NONE',  ( 18.12178482187499640, 4.985214923628404904, -9.215624999385468641 ) ) ;
#23662 = CARTESIAN_POINT ( 'NONE',  ( 0.3500000000000100253, 244.5000000000000000, 5.000000000000000888 ) ) ;
#23663 = CARTESIAN_POINT ( 'NONE',  ( 24.79029844004710625, 0.000000000000000000, 164.9602371345785343 ) ) ;
#23664 = CARTESIAN_POINT ( 'NONE',  ( 34.02892565880470954, -5.196152422706635576, 164.5001619919262055 ) ) ;
#23665 = DIRECTION ( 'NONE',  ( -0.000000000000000000, 0.000000000000000000, 1.000000000000000000 ) ) ;
#23666 = CARTESIAN_POINT ( 'NONE',  ( 15.00000000000000000, 249.0624999999999716, -3.464101615137752166 ) ) ;
#23667 = CARTESIAN_POINT ( 'NONE',  ( 13.62178482187501416, 196.8031250006145285, 23.59362340125806767 ) ) ;
#23668 = CARTESIAN_POINT ( 'NONE',  ( -12.50000000000000355, 107.6898137178985735, 0.1745138560722786503 ) ) ;
#23669 = CARTESIAN_POINT ( 'NONE',  ( -10.69584247140444866, 131.4476862821014720, 6.932735513423972762 ) ) ;
#23671 = ORIENTED_EDGE ( 'NONE', *, *, #30568, .T. ) ;
#23670 = ORIENTED_EDGE ( 'NONE', *, *, #35754, .T. ) ;
#23672 = CARTESIAN_POINT ( 'NONE',  ( 27.24356964374999635, 196.4656250006145228, -15.72908226750539029 ) ) ;
#23673 = CARTESIAN_POINT ( 'NONE',  ( 15.24356964374999990, 239.8093750006145228, -3.323476615752268604 ) ) ;
#23674 = CARTESIAN_POINT ( 'NONE',  ( -6.092822981423666739, 72.61481371789855643, -14.25334919248795096 ) ) ;
#23675 = CARTESIAN_POINT ( 'NONE',  ( 18.12178482187500350, -4.985214923628407568, -5.128124999385475391 ) ) ;
#23676 = CARTESIAN_POINT ( 'NONE',  ( 18.12178482187499640, 247.0843750006145285, -4.985214923628404904 ) ) ;
#23677 = CARTESIAN_POINT ( 'NONE',  ( -9.534712964251941258, 95.22268628210143504, 1.715153634034234154 ) ) ;
#23678 = CARTESIAN_POINT ( 'NONE',  ( 26.99999999999999645, 196.7750000012290741, -15.58845726811990495 ) ) ;
#23679 = CARTESIAN_POINT ( 'NONE',  ( 7.954856959092311719, 83.82731371789856212, -5.529263428287300108 ) ) ;
#23680 = CARTESIAN_POINT ( 'NONE',  ( 10.31873187879410914, 0.000000000000000000, -5.990624999385518734 ) ) ;
#23681 = EDGE_CURVE ( 'NONE', #23017, #21628, #3281, .T. ) ;
#23682 = CARTESIAN_POINT ( 'NONE',  ( 23.87821517812500005, 242.2468750006145228, 4.985214923628404016 ) ) ;
#23683 = CARTESIAN_POINT ( 'NONE',  ( 10.69584247140429589, 39.55231371789855643, 6.932735513424201024 ) ) ;
#23684 = DIRECTION ( 'NONE',  ( 0.9961946980917461003, 0.000000000000000000, -0.08715574274765142126 ) ) ;
#23685 = CARTESIAN_POINT ( 'NONE',  ( -2.311890736173176641, 106.7226862821014635, -12.53471296425194836 ) ) ;
#23686 = CARTESIAN_POINT ( 'NONE',  ( 22.56230152254410015, 3.464101615137755275, -5.474999998770977427 ) ) ;
#23687 = CARTESIAN_POINT ( 'NONE',  ( -34.96205436395488420, 214.6737587650352168, 4.842901733360204908 ) ) ;
#23688 = DIRECTION ( 'NONE',  ( 0.08715574274765150453, 0.000000000000000000, 0.9961946980917461003 ) ) ;
#23689 = CARTESIAN_POINT ( 'NONE',  ( 37.10082094864278446, 3.604726614523238837, 162.3962978386346663 ) ) ;
#23690 = AXIS2_PLACEMENT_3D ( 'NONE', #6814, #29559, #3597 ) ;
#23691 = CARTESIAN_POINT ( 'NONE',  ( -2.908627838312119351, 88.32268628210142936, -15.53471296425195369 ) ) ;
#23692 = CARTESIAN_POINT ( 'NONE',  ( 19.68408634441911076, 5.407089921784862696, -3.496874999385557459 ) ) ;
#23693 = LINE ( 'NONE', #29744, #10918 ) ;
#23694 = CARTESIAN_POINT ( 'NONE',  ( 19.56230152254410370, 5.196152422706631135, -7.237499998771018461 ) ) ;
#23695 = CARTESIAN_POINT ( 'NONE',  ( 27.00000000000001421, 198.3875000000000171, 15.58845726811988897 ) ) ;
#23696 = CARTESIAN_POINT ( 'NONE',  ( 7.954856959092191815, 119.3726862821014265, 5.529263428287477744 ) ) ;
#23697 = CARTESIAN_POINT ( 'NONE',  ( 27.00000000000001421, 198.9500000012290002, 15.58845726811988897 ) ) ;
#23698 = ADVANCED_FACE ( 'NONE', ( #14007 ), #918, .F. ) ;
#23699 = CARTESIAN_POINT ( 'NONE',  ( 8.632099005475504683, 9.547686282101452093, 13.23911966647218996 ) ) ;
#23700 = CARTESIAN_POINT ( 'NONE',  ( 5.778771075727756162E-15, 195.9218750006145342, 31.45816453501075927 ) ) ;
#23701 = CARTESIAN_POINT ( 'NONE',  ( 26.75643035624999655, 242.8093750006144944, -3.323476615752271712 ) ) ;
#23702 = ORIENTED_EDGE ( 'NONE', *, *, #15057, .F. ) ;
#23703 = EDGE_CURVE ( 'NONE', #10385, #23800, #7187, .T. ) ;
#23704 = CARTESIAN_POINT ( 'NONE',  ( 24.94881294716940090, 3.604726614523236616, 166.7720662417328583 ) ) ;
#23705 = CARTESIAN_POINT ( 'NONE',  ( 23.87821517812500005, -4.985214923628404016, -4.040624999385455496 ) ) ;
#23706 = CARTESIAN_POINT ( 'NONE',  ( 22.56230152254505228, -3.464101615137219259, -4.762500000000051692 ) ) ;
#23707 = CARTESIAN_POINT ( 'NONE',  ( 20.99999999999999645, 185.0294372515228645, 0.000000000000000000 ) ) ;
#23708 = CARTESIAN_POINT ( 'NONE',  ( 38.04237167757703020, 114.1383727779938511, 2.500000000000000000 ) ) ;
#23709 = CARTESIAN_POINT ( 'NONE',  ( 37.10902328307243181, -3.464101615137552326, 165.2846991979039046 ) ) ;
#23710 = DIRECTION ( 'NONE',  ( 0.000000000000000000, 0.000000000000000000, -1.000000000000000000 ) ) ;
#23711 = CARTESIAN_POINT ( 'NONE',  ( -7.954856959092309943, 24.02731371789854364, 5.529263428287300108 ) ) ;
#23712 = CARTESIAN_POINT ( 'NONE',  ( 27.24356964375000345, 199.1843750006145228, -3.336375036156643733E-15 ) ) ;
#23713 = ORIENTED_EDGE ( 'NONE', *, *, #35777, .F. ) ;
#23714 = CARTESIAN_POINT ( 'NONE',  ( 23.87821517812499650, 246.8968750006145285, -4.985214923628404904 ) ) ;
#23716 = AXIS2_PLACEMENT_3D ( 'NONE', #17502, #34549, #20160 ) ;
#23715 = CARTESIAN_POINT ( 'NONE',  ( 2.660918448318003282, 49.90231371789855075, 12.46528703574811558 ) ) ;
#23717 = CARTESIAN_POINT ( 'NONE',  ( 18.12178482187499640, 4.985214923628404904, -1.115624999385472771 ) ) ;
#23718 = CARTESIAN_POINT ( 'NONE',  ( -11.61527771782809282, 7.064813717898549505, -4.622313124798832717 ) ) ;
#23719 = EDGE_CURVE ( 'NONE', #33922, #22630, #31436, .T. ) ;
#23720 = CARTESIAN_POINT ( 'NONE',  ( 15.00000000000000000, 0.000000000000000000, -8.043749998770943321 ) ) ;
#23721 = FACE_OUTER_BOUND ( 'NONE', #29246, .T. ) ;
#23722 = VERTEX_POINT ( 'NONE', #25374 ) ;
#23723 = CARTESIAN_POINT ( 'NONE',  ( 19.68408634441911076, 5.407089921784862696, -3.946874999385563410 ) ) ;
#23724 = AXIS2_PLACEMENT_3D ( 'NONE', #22310, #16440, #8092 ) ;
#23725 = CARTESIAN_POINT ( 'NONE',  ( 13.62178482187501416, 198.6031250006145399, 23.59362340125806767 ) ) ;
#23726 = CARTESIAN_POINT ( 'NONE',  ( 31.05913452161298949, -7.209453229046482114, 164.9764337025573866 ) ) ;
#23727 = EDGE_CURVE ( 'NONE', #33209, #17126, #32061, .T. ) ;
#23728 = CARTESIAN_POINT ( 'NONE',  ( -65.23586230271183695, 205.8500491399821613, 7.418979330068642852 ) ) ;
#23729 = CARTESIAN_POINT ( 'NONE',  ( 15.24356964374999990, 248.8468750006145171, 0.000000000000000000 ) ) ;
#23730 = LINE ( 'NONE', #5525, #9133 ) ;
#23731 = CARTESIAN_POINT ( 'NONE',  ( -63.05877896937850835, 211.0902445701383101, -4.530955311639234040 ) ) ;
#23732 = CARTESIAN_POINT ( 'NONE',  ( 34.22950430627932406, 5.407089921784857367, 165.3954622995096599 ) ) ;
#23733 = ORIENTED_EDGE ( 'NONE', *, *, #23549, .F. ) ;
#23734 = CARTESIAN_POINT ( 'NONE',  ( 26.99999999999999645, 248.0687500012290627, -3.464101615137755275 ) ) ;
#23735 = CARTESIAN_POINT ( 'NONE',  ( 8.632099005475788900, 9.652313717898541867, -13.23911966647199812 ) ) ;
#23736 = CARTESIAN_POINT ( 'NONE',  ( -65.24330436395489130, 210.1155267958016850, -8.500000000000003553 ) ) ;
#23737 = AXIS2_PLACEMENT_3D ( 'NONE', #13074, #4163, #6632 ) ;
#23738 = CARTESIAN_POINT ( 'NONE',  ( 8.843639120294328748, 136.3351862821014606, -3.474262827703334722 ) ) ;
#23739 = DIRECTION ( 'NONE',  ( -0.000000000000000000, -0.000000000000000000, -1.000000000000000000 ) ) ;
#23740 = CARTESIAN_POINT ( 'NONE',  ( 0.1745138560725515708, 33.41018628210144925, -12.50000000000000355 ) ) ;
#23741 = CARTESIAN_POINT ( 'NONE',  ( 13.56230152254410548, 5.196152422706636465, -6.825000000000025935 ) ) ;
#23742 = ORIENTED_EDGE ( 'NONE', *, *, #28696, .T. ) ;
#23743 = CARTESIAN_POINT ( 'NONE',  ( -34.56622103062156270, 211.6261429550005744, 6.530955311639228711 ) ) ;
#23744 = CARTESIAN_POINT ( 'NONE',  ( 5.770363421893814682, 129.4351862821014549, 14.38691631536207183 ) ) ;
#23745 = CARTESIAN_POINT ( 'NONE',  ( 10.56230152254411081, 0.000000000000000000, -5.287499998771011178 ) ) ;
#23746 = CARTESIAN_POINT ( 'NONE',  ( 3.796722387233182339, 141.6148137178985849, 8.710071997420207879 ) ) ;
#23747 = CARTESIAN_POINT ( 'NONE',  ( -27.24356964375001056, 194.8857344423495874, -9.915847621322177119 ) ) ;
#23748 = FACE_OUTER_BOUND ( 'NONE', #16819, .T. ) ;
#23749 = CARTESIAN_POINT ( 'NONE',  ( 22.17721121674838614, -2.360623836386564811, -10.00000000000000178 ) ) ;
#23750 = DIRECTION ( 'NONE',  ( -1.000000000000000000, 0.000000000000000000, -0.000000000000000000 ) ) ;
#23751 = CARTESIAN_POINT ( 'NONE',  ( 30.82136276087599214, 6.928203230275514990, 162.2586900412136686 ) ) ;
#23752 = CARTESIAN_POINT ( 'NONE',  ( 18.12178482187499640, 242.1343750006145115, -4.985214923628404904 ) ) ;
#23753 = CARTESIAN_POINT ( 'NONE',  ( 8.843639120294245259, 76.06481371789855928, 3.474262827703527901 ) ) ;
#23754 = CARTESIAN_POINT ( 'NONE',  ( 15.24356964374999990, 239.9593750006145285, 0.000000000000000000 ) ) ;
#23755 = ORIENTED_EDGE ( 'NONE', *, *, #33797, .T. ) ;
#23756 = CARTESIAN_POINT ( 'NONE',  ( 21.00000000000000000, 246.1187500012290172, 6.928203230275506996 ) ) ;
#23757 = CARTESIAN_POINT ( 'NONE',  ( -4.944772684328424539, 91.01481371789856212, -11.48171059495408031 ) ) ;
#23758 = CARTESIAN_POINT ( 'NONE',  ( 19.68408634441912142, -5.407089921784861808, -3.646874999385540939 ) ) ;
#23759 = CARTESIAN_POINT ( 'NONE',  ( 20.99999999999997513, 246.7375000000000114, -5.999999999999999112 ) ) ;
#23760 = CARTESIAN_POINT ( 'NONE',  ( 18.12178482187500350, -4.985214923628407568, -2.878124999385472726 ) ) ;
#23761 = CARTESIAN_POINT ( 'NONE',  ( 7.228626920338837358, 67.72731371789856780, 10.49813415416005036 ) ) ;
#23762 = CARTESIAN_POINT ( 'NONE',  ( 27.24356964375000345, 197.3843750006145399, -3.336375036156643733E-15 ) ) ;
#23763 = ORIENTED_EDGE ( 'NONE', *, *, #19158, .F. ) ;
#23764 = ORIENTED_EDGE ( 'NONE', *, *, #18128, .T. ) ;
#23765 = CARTESIAN_POINT ( 'NONE',  ( 15.24356964374999990, 0.000000000000000000, -4.190624999385467397 ) ) ;
#23766 = CARTESIAN_POINT ( 'NONE',  ( 19.56230152254412147, 5.196152422706637353, -1.050000000000023137 ) ) ;
#23767 = CARTESIAN_POINT ( 'NONE',  ( 26.75643035624999655, 247.2718750006145001, -7.049594010296217766E-16 ) ) ;
#23768 = EDGE_CURVE ( 'NONE', #36556, #17083, #27569, .T. ) ;
#23769 = CARTESIAN_POINT ( 'NONE',  ( 4.944772684328679446, 33.98518628210143788, -11.48171059495397373 ) ) ;
#23770 = AXIS2_PLACEMENT_3D ( 'NONE', #35800, #27655, #18385 ) ;
#23771 = CARTESIAN_POINT ( 'NONE',  ( -34.36086230271183695, 213.1499508600178387, -5.686928522499747451 ) ) ;
#23772 = CARTESIAN_POINT ( 'NONE',  ( 12.98158921324743176, 213.0069040450241005, -5.206989594062311433 ) ) ;
#23773 = CARTESIAN_POINT ( 'NONE',  ( -34.36086230271182984, 212.1499508600178387, -3.954877714930852495 ) ) ;
#23774 = B_SPLINE_CURVE_WITH_KNOTS ( 'NONE', 3,
 ( #33590, #7629, #4774, #27896, #25793, #22779, #19944, #11951, #14805, #26164, #20682, #31852, #23520, #5697, #32228, #29188, #37342, #35066 ),
 .UNSPECIFIED., .F., .F.,
 ( 4, 2, 2, 2, 2, 2, 2, 2, 4 ),
 ( 0.000000000000000000, 0.002646020752430532173, 0.005292041504861064345, 0.007938062257291596951, 0.009261072633506861954, 0.01058408300972212696, 0.01587612451458319390, 0.01852214526701372391, 0.02116816601944425738 ),
 .UNSPECIFIED. ) ;
#23775 = CARTESIAN_POINT ( 'NONE',  ( 33.80341017455227615, -5.196152422706629359, 161.9225082118381920 ) ) ;
#23776 = CARTESIAN_POINT ( 'NONE',  ( 12.53471296425189330, 94.17731371789857064, 2.311890736173451977 ) ) ;
#23777 = CARTESIAN_POINT ( 'NONE',  ( -58.31622103062156981, 211.0902445701382533, 4.530955311639240257 ) ) ;
#23778 =( BOUNDED_CURVE ( )  B_SPLINE_CURVE ( 2, ( #3709, #35548, #2633, #34480, #22935, #37314, #26833 ),
 .UNSPECIFIED., .F., .F. ) 
 B_SPLINE_CURVE_WITH_KNOTS ( ( 3, 2, 2, 3 ),
 ( 0.1956521739130406834, 0.2028985507246359177, 0.2101449275362311242, 0.2173913043478263585 ),
 .UNSPECIFIED. ) 
 CURVE ( )  GEOMETRIC_REPRESENTATION_ITEM ( )  RATIONAL_B_SPLINE_CURVE ( ( 1.000000000000051736, 0.8660254037843868602, 1.000000000000000000, 0.8660254037844387076, 1.000000000000000000, 0.8660254037844336006, 1.000000000000005107 ) ) 
 REPRESENTATION_ITEM ( '' )  );
#23779 = CARTESIAN_POINT ( 'NONE',  ( -69.00372103062157692, 216.5309553116391612, -1.626142955000564383 ) ) ;
#23780 = CARTESIAN_POINT ( 'NONE',  ( 26.75643035624999655, -3.323476615752267271, -7.715624999385478411 ) ) ;
#23781 = CARTESIAN_POINT ( 'NONE',  ( 20.99999999999999645, 185.0294372515228645, 0.000000000000000000 ) ) ;
#23782 = CARTESIAN_POINT ( 'NONE',  ( 11.08355503943118769, 58.23981371789854222, 10.83675517735179028 ) ) ;
#23783 = CARTESIAN_POINT ( 'NONE',  ( -53.36086230271183695, 214.1499508600178387, -7.418979330068641964 ) ) ;
#23784 = CARTESIAN_POINT ( 'NONE',  ( 26.99999999999985789, -3.464101615137830770, -0.6562499987709674576 ) ) ;
#23785 = CARTESIAN_POINT ( 'NONE',  ( 8.962234695871762469, 89.76018628210144357, -8.715434833791931624 ) ) ;
#23786 = CARTESIAN_POINT ( 'NONE',  ( 0.1745138560725837118, 42.61018628210144499, -15.50000000000000533 ) ) ;
#23787 = CARTESIAN_POINT ( 'NONE',  ( 19.56230152254412147, -5.196152422706635576, -0.7500000000000839329 ) ) ;
#23788 = CARTESIAN_POINT ( 'NONE',  ( 24.40136593803570975, -3.604726614523244610, 160.5147182943441067 ) ) ;
#23789 = CARTESIAN_POINT ( 'NONE',  ( -14.38691631536207183, 48.93518628210144072, 5.770363421893814682 ) ) ;
#23790 = EDGE_CURVE ( 'NONE', #25286, #16548, #11036, .T. ) ;
#23791 = CARTESIAN_POINT ( 'NONE',  ( 22.80587116629411071, -3.604726614523235284, -9.853124999385531879 ) ) ;
#23792 = CARTESIAN_POINT ( 'NONE',  ( 2.999999999999997335, 244.5000000000000000, -10.00000000000000000 ) ) ;
#23793 = CARTESIAN_POINT ( 'NONE',  ( -54.35788769728821279, 216.4690446883607535, 1.857196546604031662 ) ) ;
#23794 = CARTESIAN_POINT ( 'NONE',  ( 10.74238581874539022, 1.953770193659143395, -10.00000000000000178 ) ) ;
#23795 = CARTESIAN_POINT ( 'NONE',  ( -12.50000000000000355, 21.91018628210143859, -0.1745138560725492671 ) ) ;
#23796 =( BOUNDED_CURVE ( )  B_SPLINE_CURVE ( 2, ( #487, #12053, #3526, #32515, #24003, #671, #18134 ),
 .UNSPECIFIED., .F., .F. ) 
 B_SPLINE_CURVE_WITH_KNOTS ( ( 3, 2, 2, 3 ),
 ( 0.2826086956521750015, 0.2898550724637684040, 0.2971014492753618064, 0.3043478260869552088 ),
 .UNSPECIFIED. ) 
 CURVE ( )  GEOMETRIC_REPRESENTATION_ITEM ( )  RATIONAL_B_SPLINE_CURVE ( ( 0.9999999999999794609, 0.8660254037844592467, 1.000000000000000000, 0.8660254037844387076, 1.000000000000000000, 0.8660254037844633546, 0.9999999999999753530 ) ) 
 REPRESENTATION_ITEM ( '' )  );
#23797 = CARTESIAN_POINT ( 'NONE',  ( 18.00000000000000000, 247.2812500012290400, -5.196152422706630247 ) ) ;
#23798 = CARTESIAN_POINT ( 'NONE',  ( 6.840914352311949109, 141.0398137178985678, 6.594114490232462877 ) ) ;
#23799 = CARTESIAN_POINT ( 'NONE',  ( 18.12178482187499640, 247.0843750006145285, -4.985214923628404904 ) ) ;
#23800 = VERTEX_POINT ( 'NONE', #19524 ) ;
#23801 = CARTESIAN_POINT ( 'NONE',  ( 26.99999999999999645, 3.464101615137755275, -6.037499999999993427 ) ) ;
#23802 = PRODUCT_DEFINITION_SHAPE ( 'NONE', 'NONE',  #37506 ) ;
#23803 = CARTESIAN_POINT ( 'NONE',  ( -3.253724281355068545E-15, 197.6374999999999602, -27.00000000000000000 ) ) ;
#23804 = CARTESIAN_POINT ( 'NONE',  ( 16.56230152254411081, 7.209453229046475009, -4.303124999385498306 ) ) ;
#23805 = CARTESIAN_POINT ( 'NONE',  ( 37.37536153829788077, 3.604726614523238837, 165.5343111376236607 ) ) ;
#23806 = CARTESIAN_POINT ( 'NONE',  ( 15.00000000000000000, 240.0999999999999943, 0.000000000000000000 ) ) ;
#23807 = CARTESIAN_POINT ( 'NONE',  ( -9.244144843276098200, 218.8666023059713268, 3.366928170503552309 ) ) ;
#23808 = CARTESIAN_POINT ( 'NONE',  ( -8.715434833791929847, 41.46018628210144641, -8.962234695871762469 ) ) ;
#23809 = EDGE_LOOP ( 'NONE', ( #18823, #28035, #23904, #32042 ) ) ;
#23810 = ORIENTED_EDGE ( 'NONE', *, *, #26862, .T. ) ;
#23811 = CARTESIAN_POINT ( 'NONE',  ( 26.99999999999999645, 7.347880794884117764E-16, -2.475000000000004974 ) ) ;
#23812 = CARTESIAN_POINT ( 'NONE',  ( -4.694659320240884604E-14, 197.4124999999999943, 27.00000000000000000 ) ) ;
#23814 = CARTESIAN_POINT ( 'NONE',  ( 20.99999999999995026, 243.1375000000000455, -5.999999999999998224 ) ) ;
#23813 = COLOUR_RGB ( '',0.8941176470588234615, 0.8941176470588234615, 0.8941176470588234615 ) ;
#23815 = CARTESIAN_POINT ( 'NONE',  ( 21.00000000000000000, 6.646953231504538984, -6.553124999385445903 ) ) ;
#23816 = CARTESIAN_POINT ( 'NONE',  ( 12.46528703574805874, 91.19768628210145778, 2.660918448318279950 ) ) ;
#23817 = CARTESIAN_POINT ( 'NONE',  ( -14.25334919248795096, 15.11481371789854933, 6.092822981423662299 ) ) ;
#23818 = CARTESIAN_POINT ( 'NONE',  ( 26.99999999999999645, 249.2874999999999943, 3.464101615137751278 ) ) ;
#23819 = CARTESIAN_POINT ( 'NONE',  ( 26.75643035624999655, 240.6343750006145115, -7.049594010296217766E-16 ) ) ;
#23820 = CARTESIAN_POINT ( 'NONE',  ( -65.63169563604516554, 210.1155267958017703, 4.499999999999996447 ) ) ;
#23821 = DIRECTION ( 'NONE',  ( 0.9961946980917462113, 0.000000000000000000, -0.08715574274765118534 ) ) ;
#23822 = CARTESIAN_POINT ( 'NONE',  ( 37.38356387272718706, -3.464101615137751278, 168.4227124968929559 ) ) ;
#23823 = CARTESIAN_POINT ( 'NONE',  ( -3.796722387233185003, 8.214813717898532985, -8.710071997420207879 ) ) ;
#23824 = CARTESIAN_POINT ( 'NONE',  ( -62.07663769728823411, 204.3130714775002730, 3.149950860017883603 ) ) ;
#23825 = CARTESIAN_POINT ( 'NONE',  ( -33.37127896937850124, 218.5309553116392465, 2.162041339862725842 ) ) ;
#23826 = VECTOR ( 'NONE', #20719, 1000.000000000000000 ) ;
#23827 = SHAPE_DEFINITION_REPRESENTATION ( #17744, #10836 ) ;
#23828 = CARTESIAN_POINT ( 'NONE',  ( 18.12178482187500350, -4.985214923628407568, -0.6281249993854709501 ) ) ;
#23829 = CARTESIAN_POINT ( 'NONE',  ( -27.24356964374999990, 198.8656250006145569, -15.72908226750537786 ) ) ;
#23830 = CARTESIAN_POINT ( 'NONE',  ( -15.50000000000000533, 135.2898137178985394, 0.1745138560722471477 ) ) ;
#23831 = CARTESIAN_POINT ( 'NONE',  ( -58.30877896937847993, 211.6261429550004607, -6.530955311639245586 ) ) ;
#23832 = EDGE_CURVE ( 'NONE', #20636, #6128, #2806, .T. ) ;
#23833 = VERTEX_POINT ( 'NONE', #22543 ) ;
#23834 = CARTESIAN_POINT ( 'NONE',  ( -2.311890736173176641, 42.32268628210145067, -12.53471296425194836 ) ) ;
#23835 = CARTESIAN_POINT ( 'NONE',  ( 22.60769515458672885, 245.2388461906613486, 5.999999999999997335 ) ) ;
#23836 = CARTESIAN_POINT ( 'NONE',  ( 19.39230484541324628, 247.2075961894323086, -5.999999999999989342 ) ) ;
#23837 = CARTESIAN_POINT ( 'NONE',  ( 37.48158259977161322, -3.604726614523238837, 166.7484234259230220 ) ) ;
#23838 = CARTESIAN_POINT ( 'NONE',  ( 10.83675517735155225, 110.4601862821014606, 11.08355503943142573 ) ) ;
#23839 =( BOUNDED_CURVE ( )  B_SPLINE_CURVE ( 2, ( #25503, #2190, #19468, #25318, #25691, #28897, #26057 ),
 .UNSPECIFIED., .F., .F. ) 
 B_SPLINE_CURVE_WITH_KNOTS ( ( 3, 2, 2, 3 ),
 ( 0.6304347826086960094, 0.6376811594202902445, 0.6449275362318845906, 0.6521739130434789367 ),
 .UNSPECIFIED. ) 
 CURVE ( )  GEOMETRIC_REPRESENTATION_ITEM ( )  RATIONAL_B_SPLINE_CURVE ( ( 0.9999999999999938938, 0.8660254037844448138, 1.000000000000000000, 0.8660254037844387076, 1.000000000000000000, 0.8660254037844263841, 1.000000000000012212 ) ) 
 REPRESENTATION_ITEM ( '' )  );
#23840 = CARTESIAN_POINT ( 'NONE',  ( -64.05580436395490551, 216.5000000000000000, 0.1155267958017343610 ) ) ;
#23841 = ADVANCED_FACE ( 'NONE', ( #20261 ), #2248, .T. ) ;
#23842 = CARTESIAN_POINT ( 'NONE',  ( 19.68408634441910721, 5.407089921784857367, -0.7406249993855418268 ) ) ;
#23843 = CARTESIAN_POINT ( 'NONE',  ( -5.529263428287477744, 66.47268628210146346, 7.954856959092191815 ) ) ;
#23844 = DIRECTION ( 'NONE',  ( 0.000000000000000000, 0.000000000000000000, 1.000000000000000000 ) ) ;
#23845 = DIRECTION ( 'NONE',  ( -0.000000000000000000, -0.000000000000000000, 1.000000000000000000 ) ) ;
#23846 = VECTOR ( 'NONE', #25703, 1000.000000000000000 ) ;
#23847 = EDGE_CURVE ( 'NONE', #11542, #13979, #31071, .T. ) ;
#23848 = CARTESIAN_POINT ( 'NONE',  ( -2.660918448318275509, 102.6976862821014720, 12.46528703574805874 ) ) ;
#23849 = CARTESIAN_POINT ( 'NONE',  ( -35.67863628793906372, 245.9410842096246199, -2.499999999999999556 ) ) ;
#23850 = CARTESIAN_POINT ( 'NONE',  ( 1.120210788295102201E-13, 195.0500000012290798, -27.00000000000000711 ) ) ;
#23851 = ORIENTED_EDGE ( 'NONE', *, *, #4027, .T. ) ;
#23852 = CARTESIAN_POINT ( 'NONE',  ( 36.90472052746056875, 3.604726614523238837, 160.1548597679282295 ) ) ;
#23853 = CARTESIAN_POINT ( 'NONE',  ( 26.99999999999999645, 7.347880794884117764E-16, -0.6750000000000089262 ) ) ;
#23854 = CARTESIAN_POINT ( 'NONE',  ( -13.49999999999998401, 198.3875000012290286, 23.38268590217985476 ) ) ;
#23855 = CARTESIAN_POINT ( 'NONE',  ( 34.14616162727688931, 5.407089921784862696, 164.4428511194594478 ) ) ;
#23856 = CARTESIAN_POINT ( 'NONE',  ( 27.88834045260238526, -5.196152422706638241, 163.1552313894900976 ) ) ;
#23857 = LINE ( 'NONE', #27760, #15034 ) ;
#23858 = CARTESIAN_POINT ( 'NONE',  ( 24.00000000000000000, 247.9000000000000057, 5.196152422706629359 ) ) ;
#23859 = CARTESIAN_POINT ( 'NONE',  ( 13.62178482187499640, 196.5031250006145456, -23.59362340125807123 ) ) ;
#23860 = CARTESIAN_POINT ( 'NONE',  ( 8.715434833792128799, 111.1398137178985621, -8.962234695871567070 ) ) ;
#23861 = CARTESIAN_POINT ( 'NONE',  ( 12.53471296425194659, 109.0226862821014606, -2.311890736173178418 ) ) ;
#23862 = ORIENTED_EDGE ( 'NONE', *, *, #36066, .T. ) ;
#23863 = CARTESIAN_POINT ( 'NONE',  ( 27.24356964375000345, 195.0781250006145342, -3.336375036156643733E-15 ) ) ;
#23864 = CARTESIAN_POINT ( 'NONE',  ( 26.75643035624999655, 240.4843750006145058, 3.323476615752267715 ) ) ;
#23865 = CARTESIAN_POINT ( 'NONE',  ( -15.53471296425188442, 80.37731371789853085, -2.908627838312459080 ) ) ;
#23866 = CARTESIAN_POINT ( 'NONE',  ( 21.00000000000000000, 6.646953231504538984, -4.415624999385457272 ) ) ;
#23867 = CARTESIAN_POINT ( 'NONE',  ( 23.87821517812500005, 247.3093750006145228, 4.985214923628404016 ) ) ;
#23868 = CARTESIAN_POINT ( 'NONE',  ( 5.233372021372432847, 92.34768628210142083, 8.152565276336710909 ) ) ;
#23869 = VECTOR ( 'NONE', #33677, 1000.000000000000000 ) ;
#23870 = AXIS2_PLACEMENT_3D ( 'NONE', #32156, #23640, #17399 ) ;
#23871 = CARTESIAN_POINT ( 'NONE',  ( -20.68320086892770604, 194.6619763917542514, -17.35526438333879540 ) ) ;
#23872 = CARTESIAN_POINT ( 'NONE',  ( -9.534712964251895073, 71.17731371789855643, -1.715153634034446428 ) ) ;
#23873 = CARTESIAN_POINT ( 'NONE',  ( 10.31873187879411269, 3.604726614523236616, -4.228124999385537208 ) ) ;
#23874 = AXIS2_PLACEMENT_3D ( 'NONE', #28699, #8988, #14674 ) ;
#23875 = CARTESIAN_POINT ( 'NONE',  ( -5.529263428287297444, 118.3273137178985763, -7.954856959092311719 ) ) ;
#23876 = CARTESIAN_POINT ( 'NONE',  ( 15.24356964374999990, 242.9593750006145001, -3.323476615752268604 ) ) ;
#23877 = CARTESIAN_POINT ( 'NONE',  ( 7.228626920338837358, 49.32731371789855501, 10.49813415416005036 ) ) ;
#23878 = CARTESIAN_POINT ( 'NONE',  ( 16.56230152254410726, 0.000000000000000000, -10.00000000000000000 ) ) ;
#23879 = CARTESIAN_POINT ( 'NONE',  ( 10.69584247140445221, 99.24768628210146915, -6.932735513423970097 ) ) ;
#23880 = CARTESIAN_POINT ( 'NONE',  ( 22.56230152254411081, -3.464101615137751278, -6.899999998771022547 ) ) ;
#23881 = CARTESIAN_POINT ( 'NONE',  ( -66.03497103062157692, 206.1606490808709111, -2.350049139982163027 ) ) ;
#23882 = CARTESIAN_POINT ( 'NONE',  ( -6.932735513423968321, 133.7476862821014549, -10.69584247140445221 ) ) ;
#23883 = CARTESIAN_POINT ( 'NONE',  ( 27.93778984224218931, 5.407089921784856479, 165.1177646232817153 ) ) ;
#23884 = CARTESIAN_POINT ( 'NONE',  ( 3.257655550457285720, 88.89768628210146062, -15.46528703574804986 ) ) ;
#23885 = CARTESIAN_POINT ( 'NONE',  ( 16.56230152254411081, 7.209453229046482114, -3.909374999385482496 ) ) ;
#23886 = CARTESIAN_POINT ( 'NONE',  ( 5.649999999999987921, 244.5000000000000000, 5.000000000000000000 ) ) ;
#23887 = CARTESIAN_POINT ( 'NONE',  ( 26.99999999999999645, 7.347880794884117764E-16, -7.424999999999987388 ) ) ;
#23888 = CARTESIAN_POINT ( 'NONE',  ( -13.49999999999998401, 199.1750000000000114, 23.38268590217985476 ) ) ;
#23889 = CARTESIAN_POINT ( 'NONE',  ( 9.465287035748067623, 109.5976862821014493, 2.064181346179272847 ) ) ;
#23890 = CARTESIAN_POINT ( 'NONE',  ( 19.39230484541326405, 248.3486538117967370, 5.999999999999995559 ) ) ;
#23891 = CARTESIAN_POINT ( 'NONE',  ( -10.83675517735155047, 13.86018628210145032, -11.08355503943142750 ) ) ;
#23892 = CARTESIAN_POINT ( 'NONE',  ( -27.24356964374999635, 195.3968750006145569, 15.72908226750539384 ) ) ;
#23893 = CARTESIAN_POINT ( 'NONE',  ( 15.24356964375000167, 243.0343750006144887, 3.323476615752272600 ) ) ;
#23894 = ORIENTED_EDGE ( 'NONE', *, *, #21219, .T. ) ;
#23895 = CARTESIAN_POINT ( 'NONE',  ( 37.45053336641773711, 7.646167579472015790E-16, 166.3935290647278009 ) ) ;
#23896 = CARTESIAN_POINT ( 'NONE',  ( 21.00000000000000000, 6.646953231504538984, -2.053124999385488092 ) ) ;
#23897 = CARTESIAN_POINT ( 'NONE',  ( 0.000000000000000000, 0.000000000000000000, -5.000000000000000000 ) ) ;
#23898 = DIRECTION ( 'NONE',  ( 0.08715574274765150453, 0.000000000000000000, 0.9961946980917461003 ) ) ;
#23899 = CARTESIAN_POINT ( 'NONE',  ( 16.56230152254411081, 6.928203230275506996, -5.849999998771011178 ) ) ;
#23900 = CARTESIAN_POINT ( 'NONE',  ( 18.00000000000000355, -5.196152422706632912, -7.518749998770946519 ) ) ;
#23901 = CARTESIAN_POINT ( 'NONE',  ( 26.99999999999999645, 198.4625000000000057, -15.58845726811990495 ) ) ;
#23902 = CARTESIAN_POINT ( 'NONE',  ( -3.796722387233185003, 26.61481371789854933, -8.710071997420207879 ) ) ;
#23903 = CARTESIAN_POINT ( 'NONE',  ( -27.24356964375000345, 197.1593750006145456, 0.000000000000000000 ) ) ;
#23905 = ORIENTED_EDGE ( 'NONE', *, *, #5262, .F. ) ;
#23904 = ORIENTED_EDGE ( 'NONE', *, *, #30346, .T. ) ;
#23906 = CARTESIAN_POINT ( 'NONE',  ( 26.75643035624999655, 246.7843750006145171, 3.323476615752267715 ) ) ;
#23907 = CARTESIAN_POINT ( 'NONE',  ( 8.962234695871567070, 21.43981371789854862, 8.715434833792127023 ) ) ;
#23908 = CARTESIAN_POINT ( 'NONE',  ( 18.12178482187500350, -4.985214923628407568, -0.9656249993854615354 ) ) ;
#23909 = CARTESIAN_POINT ( 'NONE',  ( 15.50000000000000533, 139.8898137178985621, -0.1745138560722452326 ) ) ;
#23910 = CARTESIAN_POINT ( 'NONE',  ( 24.00000000000000000, -5.196152422706629359, -7.893749998770960730 ) ) ;
#23911 =( BOUNDED_CURVE ( )  B_SPLINE_CURVE ( 2, ( #15566, #12717, #9688, #21079, #958 ),
 .UNSPECIFIED., .F., .F. ) 
 B_SPLINE_CURVE_WITH_KNOTS ( ( 3, 2, 3 ),
 ( 0.000000000000000000, 0.01388888888888888985, 0.02083333333333333565 ),
 .UNSPECIFIED. ) 
 CURVE ( )  GEOMETRIC_REPRESENTATION_ITEM ( )  RATIONAL_B_SPLINE_CURVE ( ( 1.000000000000000000, 0.8660254037844387076, 1.000000000000000000, 0.9330127018922192983, 0.9330127018922194093 ) ) 
 REPRESENTATION_ITEM ( '' )  );
#23912 = CARTESIAN_POINT ( 'NONE',  ( 20.99999999999999645, 0.000000000000000000, -8.000000000000000000 ) ) ;
#23913 = VERTEX_POINT ( 'NONE', #16673 ) ;
#23914 = CARTESIAN_POINT ( 'NONE',  ( 22.80587116629411781, 3.604726614523243278, -4.434374999385503280 ) ) ;
#23915 = VERTEX_POINT ( 'NONE', #13827 ) ;
#23916 = CARTESIAN_POINT ( 'NONE',  ( -27.24356964374999635, 195.7906250006145115, 15.72908226750539384 ) ) ;
#23917 = CARTESIAN_POINT ( 'NONE',  ( 34.13308826586474254, -5.407089921784861808, 164.2934219147456929 ) ) ;
#23918 = CARTESIAN_POINT ( 'NONE',  ( -35.35044563604516554, 205.1570982666397072, -4.673758765035155527 ) ) ;
#23919 = CARTESIAN_POINT ( 'NONE',  ( 15.24356964374999990, 249.7093750006145285, -3.323476615752268604 ) ) ;
#23920 =( NAMED_UNIT ( * ) PLANE_ANGLE_UNIT ( ) SI_UNIT ( $, .RADIAN. ) );
#23921 = CARTESIAN_POINT ( 'NONE',  ( 3.551475717527324030E-15, 210.0000000000000284, 28.99999999999999645 ) ) ;
#23922 = CARTESIAN_POINT ( 'NONE',  ( -40.29836230271183695, 206.0451222850691977, -2.149950860017851184 ) ) ;
#23923 = CARTESIAN_POINT ( 'NONE',  ( -32.78497103062156981, 204.4285982733020148, -3.350049139982115509 ) ) ;
#23924 = CARTESIAN_POINT ( 'NONE',  ( 37.41458162253433528, 3.604726614523238837, 165.9825987517649253 ) ) ;
#23925 = ORIENTED_EDGE ( 'NONE', *, *, #8524, .T. ) ;
#23926 = CARTESIAN_POINT ( 'NONE',  ( 20.99999999999999645, 185.0294372515228645, -5.999999999999999112 ) ) ;
#23927 = CARTESIAN_POINT ( 'NONE',  ( -10.83675517735155047, 133.4601862821014606, -11.08355503943142750 ) ) ;
#23928 = CARTESIAN_POINT ( 'NONE',  ( -48.61830436395490551, 209.8844732041983150, 8.500000000000003553 ) ) ;
#23929 = CARTESIAN_POINT ( 'NONE',  ( 3.796722387233379514, 125.9851862821014521, -8.710071997420127943 ) ) ;
#23930 = CARTESIAN_POINT ( 'NONE',  ( 20.99999999999995026, 241.3375000000000341, -5.999999999999998224 ) ) ;
#23931 = CARTESIAN_POINT ( 'NONE',  ( 10.49813415415989581, 36.57268628210145067, 7.228626920339068285 ) ) ;
#23932 = CARTESIAN_POINT ( 'NONE',  ( 16.56230152254411081, -6.928203230275514990, -6.187500000000013323 ) ) ;
#23933 = VERTEX_POINT ( 'NONE', #28220 ) ;
#23934 = CARTESIAN_POINT ( 'NONE',  ( 7.234628195640295800, 197.5450961906613827, 27.00000000000001066 ) ) ;
#23935 = CARTESIAN_POINT ( 'NONE',  ( -3.257655550457281723, 121.0976862821014635, 15.46528703574804986 ) ) ;
#23936 = CARTESIAN_POINT ( 'NONE',  ( 10.56230152254410903, 0.000000000000000000, -6.187499998771023080 ) ) ;
#23937 = CARTESIAN_POINT ( 'NONE',  ( -9.500000000000005329, 3.510186282101451560, -0.1745138560725176813 ) ) ;
#23938 = CARTESIAN_POINT ( 'NONE',  ( -27.24356964375000345, 198.9031250006145228, 0.000000000000000000 ) ) ;
#23939 = CARTESIAN_POINT ( 'NONE',  ( 7.234628195640269155, 195.7450961906613713, 27.00000000000003197 ) ) ;
#23940 = CYLINDRICAL_SURFACE ( 'NONE', #14410, 5.999999999999994671 ) ;
#23941 = CARTESIAN_POINT ( 'NONE',  ( 25.17923094205850276, 3.604726614523240613, 169.4057559748129336 ) ) ;
#23942 = CARTESIAN_POINT ( 'NONE',  ( 16.56230152254410726, 0.000000000000000000, -10.00000000000000000 ) ) ;
#23943 = CARTESIAN_POINT ( 'NONE',  ( -9.465287035748106703, 70.60231371789853938, 2.064181346179061460 ) ) ;
#23944 = FACE_OUTER_BOUND ( 'NONE', #27900, .T. ) ;
#23945 = VERTEX_POINT ( 'NONE', #19713 ) ;
#23946 = VECTOR ( 'NONE', #34056, 1000.000000000000000 ) ;
#23947 = CARTESIAN_POINT ( 'NONE',  ( 21.00000000000000000, 243.6437500012290513, -6.928203230275506996 ) ) ;
#23948 = CARTESIAN_POINT ( 'NONE',  ( 7.228626920338837358, 86.12731371789855928, 10.49813415416005036 ) ) ;
#23949 = CARTESIAN_POINT ( 'NONE',  ( 10.31873187879410558, 3.604726614523240613, -2.934374999385496618 ) ) ;
#23950 = PLANE ( 'NONE',  #5779 ) ;
#23951 = CARTESIAN_POINT ( 'NONE',  ( 23.87821517812500005, -4.985214923628404016, -4.603124999385476812 ) ) ;
#23952 = CARTESIAN_POINT ( 'NONE',  ( -12.46528703574811558, 52.20231371789855501, 2.660918448318003726 ) ) ;
#23953 = CARTESIAN_POINT ( 'NONE',  ( -27.24356964374999990, 198.9218750006145626, -15.72908226750537786 ) ) ;
#23954 = AXIS2_PLACEMENT_3D ( 'NONE', #14861, #34756, #32283 ) ;
#23955 = VERTEX_POINT ( 'NONE', #31253 ) ;
#23956 = VERTEX_POINT ( 'NONE', #23849 ) ;
#23957 = CARTESIAN_POINT ( 'NONE',  ( 18.12178482187499640, 4.985214923628404904, -6.065624999385454963 ) ) ;
#23958 = CARTESIAN_POINT ( 'NONE',  ( 26.75643035624999655, 244.0843750006145285, 3.323476615752267715 ) ) ;
#23959 = CARTESIAN_POINT ( 'NONE',  ( -12.46528703574805697, 31.39768628210144641, -2.660918448318280838 ) ) ;
#23960 = EDGE_CURVE ( 'NONE', #31128, #17848, #14916, .T. ) ;
#23961 = CARTESIAN_POINT ( 'NONE',  ( -32.97544563604516554, 214.8429017333602360, 4.673758765035156415 ) ) ;
#23962 = CARTESIAN_POINT ( 'NONE',  ( 13.44051670066911086, 5.407089921784856479, -0.2156249993855441360 ) ) ;
#23963 = CARTESIAN_POINT ( 'NONE',  ( -62.86086230271182984, 213.1499508600178387, -5.686928522499747451 ) ) ;
#23964 = APPLICATION_PROTOCOL_DEFINITION ( 'draft international standard', 'automotive_design', 1998, #26742 ) ;
#23965 = CARTESIAN_POINT ( 'NONE',  ( 27.66282496834995186, -5.196152422706632912, 160.5775776094020557 ) ) ;
#23966 = CARTESIAN_POINT ( 'NONE',  ( 11.48171059495408208, 93.31481371789855928, -4.944772684328420986 ) ) ;
#23967 = CARTESIAN_POINT ( 'NONE',  ( -47.62872103062157692, 205.4690446883607535, 1.090244570138264368 ) ) ;
#23968 = CARTESIAN_POINT ( 'NONE',  ( -34.17038769728823411, 207.6069050685337913, 8.469044688360781947 ) ) ;
#23969 = EDGE_CURVE ( 'NONE', #20636, #13931, #22676, .T. ) ;
#23970 = CARTESIAN_POINT ( 'NONE',  ( 23.87821517812500005, -4.985214923628404016, -7.303124999385484983 ) ) ;
#23971 = CYLINDRICAL_SURFACE ( 'NONE', #36749, 2.649999999999999467 ) ;
#23972 = CARTESIAN_POINT ( 'NONE',  ( 5.770363421894130873, 64.56481371789854506, -14.38691631536193860 ) ) ;
#23973 = CARTESIAN_POINT ( 'NONE',  ( -55.34002896937850124, 202.6965474657332038, 4.350049139982197666 ) ) ;
#23974 = DIRECTION ( 'NONE',  ( 0.9933043639548628789, -0.1155267958017759528, 0.000000000000000000 ) ) ;
#23975 = CARTESIAN_POINT ( 'NONE',  ( -12.53471296425194836, 86.02268628210146062, 2.311890736173176641 ) ) ;
#23976 = CARTESIAN_POINT ( 'NONE',  ( 8.927990412390657937, 25.07268628210145067, -13.04141134922759804 ) ) ;
#23977 = MECHANICAL_DESIGN_GEOMETRIC_PRESENTATION_REPRESENTATION (  '', ( #26392 ), #10659 ) ;
#23978 = CARTESIAN_POINT ( 'NONE',  ( 10.56230152254410726, 0.000000000000000000, -3.150000000000041656 ) ) ;
#23979 = CARTESIAN_POINT ( 'NONE',  ( 30.64732363713033081, 7.209453229046482114, 160.2694137540738950 ) ) ;
#23980 = CARTESIAN_POINT ( 'NONE',  ( -3.257655550457281723, 47.49768628210145494, 15.46528703574804986 ) ) ;
#23981 = CARTESIAN_POINT ( 'NONE',  ( -13.62178482187498396, 196.7281250006145399, 23.59362340125808188 ) ) ;
#23982 = EDGE_CURVE ( 'NONE', #28452, #36517, #29137, .T. ) ;
#23983 = CARTESIAN_POINT ( 'NONE',  ( 0.000000000000000000, -20.00000000000000000, 0.000000000000000000 ) ) ;
#23984 = CARTESIAN_POINT ( 'NONE',  ( 10.56230152254410726, 0.000000000000000000, -7.650000000000045652 ) ) ;
#23985 = CARTESIAN_POINT ( 'NONE',  ( -37.33705436395490551, 205.3262412349647263, -4.842901733360204020 ) ) ;
#23986 = CARTESIAN_POINT ( 'NONE',  ( -7.234628195640263826, 195.4075961894323825, -27.00000000000003553 ) ) ;
#23987 = CARTESIAN_POINT ( 'NONE',  ( -10.49813415415989581, 13.57268628210145600, -7.228626920339068285 ) ) ;
#23988 = CARTESIAN_POINT ( 'NONE',  ( 26.75643035624999655, 249.6718750006145342, -3.323476615752271712 ) ) ;
#23989 = CARTESIAN_POINT ( 'NONE',  ( -1.715153634034442431, 133.2773137178985507, 9.534712964251900402 ) ) ;
#23990 = CARTESIAN_POINT ( 'NONE',  ( 15.24356964374999990, 246.6718750006145342, -3.323476615752268604 ) ) ;
#23991 = ORIENTED_EDGE ( 'NONE', *, *, #12882, .T. ) ;
#23992 = CARTESIAN_POINT ( 'NONE',  ( 26.99999999999999645, 3.464101615137755275, -6.937499999999985789 ) ) ;
#23993 = CARTESIAN_POINT ( 'NONE',  ( 18.00000000000000355, -5.196152422706632912, -4.425000000000012257 ) ) ;
#23994 = CARTESIAN_POINT ( 'NONE',  ( 16.56230152254411081, -7.209453229046475009, -7.678124999385515181 ) ) ;
#23995 = CARTESIAN_POINT ( 'NONE',  ( 31.12286715849720409, 7.209453229046475009, 165.7049010755369807 ) ) ;
#23996 = CARTESIAN_POINT ( 'NONE',  ( 10.56230152254273413, -3.464101615136960355, -2.549999998771006471 ) ) ;
#23997 = CARTESIAN_POINT ( 'NONE',  ( 27.00000000000001066, 199.2875000000000227, 15.58845726811988897 ) ) ;
#23998 = CARTESIAN_POINT ( 'NONE',  ( -2.660918448318275509, 47.49768628210144783, 12.46528703574805874 ) ) ;
#23999 = VERTEX_POINT ( 'NONE', #28955 ) ;
#24000 = VERTEX_POINT ( 'NONE', #17606 ) ;
#24001 = CYLINDRICAL_SURFACE ( 'NONE', #1251, 5.999999999999999112 ) ;
#24002 = CARTESIAN_POINT ( 'NONE',  ( 10.56230152254410548, 0.000000000000000000, -4.050000000000054001 ) ) ;
#24003 = CARTESIAN_POINT ( 'NONE',  ( 18.00000000000000355, -5.196152422706632912, -3.468749998770948029 ) ) ;
#24004 = LINE ( 'NONE', #32707, #35345 ) ;
#24005 = CARTESIAN_POINT ( 'NONE',  ( 23.87821517812499650, 4.985214923628404904, -6.590624999385480187 ) ) ;
#24006 = CARTESIAN_POINT ( 'NONE',  ( 0.1745138560725515708, 97.81018628210144072, -12.50000000000000355 ) ) ;
#24007 = CARTESIAN_POINT ( 'NONE',  ( 13.23911966647199812, 21.15231371789855430, 8.632099005475788900 ) ) ;
#24008 =( BOUNDED_CURVE ( )  B_SPLINE_CURVE ( 2, ( #24907, #22449, #31162, #7670, #33996, #4995, #27937, #28123, #13734 ),
 .UNSPECIFIED., .F., .F. ) 
 B_SPLINE_CURVE_WITH_KNOTS ( ( 3, 2, 2, 2, 3 ),
 ( 0.2065217391304347838, 0.2101449275362318736, 0.2173913043478260809, 0.2246376811594202882, 0.2282608695652173780 ),
 .UNSPECIFIED. ) 
 CURVE ( )  GEOMETRIC_REPRESENTATION_ITEM ( )  RATIONAL_B_SPLINE_CURVE ( ( 0.9330127018922194093, 0.9330127018922194093, 1.000000000000000000, 0.8660254037844387076, 1.000000000000000000, 0.8660254037844387076, 1.000000000000000000, 0.9330127018922196314, 0.9330127018922194093 ) ) 
 REPRESENTATION_ITEM ( '' )  );
#24009 = CARTESIAN_POINT ( 'NONE',  ( -13.50000000000000533, 197.2250000000000227, -23.38268590217984411 ) ) ;
#24010 = VECTOR ( 'NONE', #35960, 1000.000000000000000 ) ;
#24011 = CARTESIAN_POINT ( 'NONE',  ( 20.99999999999999289, 243.6437500012290229, -5.999999999999997335 ) ) ;
#24012 = CARTESIAN_POINT ( 'NONE',  ( -64.84002896937849414, 206.1606490808709111, 2.350049139982143931 ) ) ;
#24013 = CARTESIAN_POINT ( 'NONE',  ( 28.39493320743021698, 5.196152422706630247, 168.9456130733727548 ) ) ;
#24014 = CARTESIAN_POINT ( 'NONE',  ( 4.622313124798831829, 138.1648137178985678, -11.61527771782809282 ) ) ;
#24015 = EDGE_CURVE ( 'NONE', #4383, #15329, #34288, .T. ) ;
#24016 = CARTESIAN_POINT ( 'NONE',  ( -62.47247103062156981, 206.6499508600178672, 5.571401726697986057 ) ) ;
#24017 = CARTESIAN_POINT ( 'NONE',  ( -67.22247103062156270, 205.6499508600178956, 7.303452534266880569 ) ) ;
#24018 = CARTESIAN_POINT ( 'NONE',  ( 21.00000000000000000, 241.1125000000000114, 5.999999999999998224 ) ) ;
#24019 = CARTESIAN_POINT ( 'NONE',  ( 27.24356964375000345, 199.5781250006145342, -3.336375036156643733E-15 ) ) ;
#24020 = CARTESIAN_POINT ( 'NONE',  ( -15.53471296425188442, 117.1773137178985706, -2.908627838312459080 ) ) ;
#24021 = CARTESIAN_POINT ( 'NONE',  ( -60.28794563604516554, 205.3262412349647832, 4.842901733360250205 ) ) ;
#24022 = ADVANCED_FACE ( 'NONE', ( #29330 ), #23286, .F. ) ;
#24023 = ORIENTED_EDGE ( 'NONE', *, *, #14020, .F. ) ;
#24024 = CARTESIAN_POINT ( 'NONE',  ( -0.1745138560725500443, 28.81018628210144072, 12.50000000000000355 ) ) ;
#24025 = CARTESIAN_POINT ( 'NONE',  ( 15.00000000000000000, 0.000000000000000000, -6.299999999999999822 ) ) ;
#24026 = DIRECTION ( 'NONE',  ( 0.000000000000000000, 0.000000000000000000, -1.000000000000000000 ) ) ;
#24027 = CARTESIAN_POINT ( 'NONE',  ( 31.21601485855876135, -7.209453229046482114, 166.7695841591225587 ) ) ;
#24028 = CARTESIAN_POINT ( 'NONE',  ( 14.25334919248782661, 100.6851862821014834, 6.092822981423971385 ) ) ;
#24029 = CARTESIAN_POINT ( 'NONE',  ( 29.51984228635672380, 5.908847293266075162, 159.3365288790247121 ) ) ;
#24030 = CARTESIAN_POINT ( 'NONE',  ( 10.31873187879411091, 0.000000000000000000, -5.090624999385534366 ) ) ;
#24031 = CARTESIAN_POINT ( 'NONE',  ( 2.064181346179272847, 52.09768628210144925, -9.465287035748065847 ) ) ;
#24032 = CARTESIAN_POINT ( 'NONE',  ( -14.50000000000000355, 252.0000000000000000, 5.000000000000000000 ) ) ;
#24033 = CARTESIAN_POINT ( 'NONE',  ( -42.87872103062157692, 201.4690446883607819, 2.162041339862843525 ) ) ;
#24034 = CARTESIAN_POINT ( 'NONE',  ( 4.944772684328679446, 79.98518628210145209, -11.48171059495397373 ) ) ;
#24035 = DIRECTION ( 'NONE',  ( 0.000000000000000000, 0.000000000000000000, -1.000000000000000000 ) ) ;
#24036 = LINE ( 'NONE', #7167, #20223 ) ;
#24037 = DIRECTION ( 'NONE',  ( -0.8083506638593009885, -0.5887012860850800999, 1.927470528863119049E-16 ) ) ;
#24038 = CARTESIAN_POINT ( 'NONE',  ( 33.70656984979341786, -5.407089921784855591, 159.4182941109592093 ) ) ;
#24039 = CARTESIAN_POINT ( 'NONE',  ( 23.87821517812499650, 4.985214923628404904, -9.290624999385460825 ) ) ;
#24040 = CARTESIAN_POINT ( 'NONE',  ( 5.438367727407757144E-14, 198.2000000012290002, -27.00000000000000000 ) ) ;
#24041 = CARTESIAN_POINT ( 'NONE',  ( 24.95044711734591658, -3.604726614523244610, 166.7907448923220954 ) ) ;
#24042 = PRODUCT_DEFINITION_CONTEXT ( 'detailed design', #26742, 'design' ) ;
#24043 = CARTESIAN_POINT ( 'NONE',  ( 34.00277893598041601, 5.196152422706637353, 164.2013035824986957 ) ) ;
#24044 = CARTESIAN_POINT ( 'NONE',  ( 18.00000000000000000, 245.8750000000000000, -5.196152422706630247 ) ) ;
#24045 = CARTESIAN_POINT ( 'NONE',  ( -1.926257025242585782E-15, 195.6406250006145342, -31.45816453501076637 ) ) ;
#24046 = CARTESIAN_POINT ( 'NONE',  ( -8.962234695871565293, 99.63981371789856212, -8.715434833792128799 ) ) ;
#24047 = CARTESIAN_POINT ( 'NONE',  ( 7.228626920339069173, 107.8726862821014549, -10.49813415415989404 ) ) ;
#24048 = ORIENTED_EDGE ( 'NONE', *, *, #3104, .F. ) ;
#24049 = VERTEX_POINT ( 'NONE', #21014 ) ;
#24050 = CARTESIAN_POINT ( 'NONE',  ( 13.62178482187501416, 195.9031250006145513, 23.59362340125806767 ) ) ;
#24051 = CARTESIAN_POINT ( 'NONE',  ( 18.12178482187499640, 240.6718750006145058, -4.985214923628404904 ) ) ;
#24052 = CARTESIAN_POINT ( 'NONE',  ( 15.46528703574811736, 75.20231371789854791, -3.257655550456947768 ) ) ;
#24053 = CARTESIAN_POINT ( 'NONE',  ( 23.87821517812500005, -4.985214923628404016, -5.503124999385489602 ) ) ;
#24054 = CARTESIAN_POINT ( 'NONE',  ( 23.87821517812499650, 247.0093750006145399, -4.985214923628404904 ) ) ;
#24055 = CARTESIAN_POINT ( 'NONE',  ( 5.529263428287477744, 107.8726862821014549, -7.954856959092191815 ) ) ;
#24056 = CARTESIAN_POINT ( 'NONE',  ( 27.00000000000001066, 195.3500000012290343, 15.58845726811988897 ) ) ;
#24057 = EDGE_CURVE ( 'NONE', #24921, #25531, #4514, .T. ) ;
#24058 = CARTESIAN_POINT ( 'NONE',  ( 1.715153634034445762, 64.27731371789853654, -9.534712964251895073 ) ) ;
#24059 = CARTESIAN_POINT ( 'NONE',  ( 10.31873187879410736, -3.604726614523240613, -5.053124999385534721 ) ) ;
#24060 = CARTESIAN_POINT ( 'NONE',  ( -1.715153634034442431, 114.8773137178985735, 9.534712964251900402 ) ) ;
#24061 = FACE_OUTER_BOUND ( 'NONE', #30488, .T. ) ;
#24062 = CARTESIAN_POINT ( 'NONE',  ( -12.53471296425189152, 34.37731371789855217, -2.311890736173453753 ) ) ;
#24063 =( BOUNDED_CURVE ( )  B_SPLINE_CURVE ( 2, ( #34587, #20015, #11290, #19655, #17355, #34408, #16616, #10913, #5400 ),
 .UNSPECIFIED., .F., .F. ) 
 B_SPLINE_CURVE_WITH_KNOTS ( ( 3, 2, 2, 2, 3 ),
 ( 0.7065217391304348116, 0.7101449275362319291, 0.7173913043478260532, 0.7246376811594202882, 0.7282608695652174058 ),
 .UNSPECIFIED. ) 
 CURVE ( )  GEOMETRIC_REPRESENTATION_ITEM ( )  RATIONAL_B_SPLINE_CURVE ( ( 0.9330127018922194093, 0.9330127018922194093, 1.000000000000000000, 0.8660254037844387076, 1.000000000000000000, 0.8660254037844387076, 1.000000000000000000, 0.9330127018922194093, 0.9330127018922194093 ) ) 
 REPRESENTATION_ITEM ( '' )  );
#24064 = CARTESIAN_POINT ( 'NONE',  ( 18.00000000000000355, -5.196152422706632912, -3.074999999999994404 ) ) ;
#24065 = CARTESIAN_POINT ( 'NONE',  ( 11.48171059495397728, 82.28518628210146346, 4.944772684328674117 ) ) ;
#24066 = CARTESIAN_POINT ( 'NONE',  ( 16.56230152254411081, 6.928203230275506996, -7.199999998770998388 ) ) ;
#24067 = CARTESIAN_POINT ( 'NONE',  ( 14.99999999999954348, 3.464101615137491930, -1.781249998770933374 ) ) ;
#24068 = CARTESIAN_POINT ( 'NONE',  ( 31.04442699002431993, 7.209453229046475009, 164.8083258472544230 ) ) ;
#24069 = CARTESIAN_POINT ( 'NONE',  ( 13.23911966647218996, 90.04768628210145209, -8.632099005475504683 ) ) ;
#24070 = CARTESIAN_POINT ( 'NONE',  ( 10.31873187879410736, 0.000000000000000000, -5.146874999385541827 ) ) ;
#24071 = PRESENTATION_STYLE_ASSIGNMENT (( #29365 ) ) ;
#24072 = FACE_OUTER_BOUND ( 'NONE', #22507, .T. ) ;
#24073 = LINE ( 'NONE', #3598, #18794 ) ;
#24074 = CARTESIAN_POINT ( 'NONE',  ( 0.1745138560725194299, 107.0101862821014578, -9.500000000000005329 ) ) ;
#24075 = CARTESIAN_POINT ( 'NONE',  ( 27.00000000000001421, 198.9500000012290002, 15.58845726811988897 ) ) ;
#24076 = CARTESIAN_POINT ( 'NONE',  ( 8.715434833791931624, 128.8601862821014663, 8.962234695871760692 ) ) ;
#24077 = CARTESIAN_POINT ( 'NONE',  ( -27.24356964374999990, 196.2218750006145456, -15.72908226750537786 ) ) ;
#24078 = CARTESIAN_POINT ( 'NONE',  ( 15.24356964375000167, 248.9968750006145513, 3.323476615752272600 ) ) ;
#24079 = VERTEX_POINT ( 'NONE', #17976 ) ;
#24080 = CARTESIAN_POINT ( 'NONE',  ( 31.29935753756119965, -7.209453229046475009, 167.7221953391727709 ) ) ;
#24081 = CARTESIAN_POINT ( 'NONE',  ( 15.24356964375000167, -3.323476615752272600, -2.353124999385463489 ) ) ;
#24082 = CARTESIAN_POINT ( 'NONE',  ( 21.00000000000000000, 242.4625000000000057, 5.999999999999998224 ) ) ;
#24083 = DIRECTION ( 'NONE',  ( -1.000000000000000000, 0.000000000000000000, 2.168404344971009484E-17 ) ) ;
#24084 = LINE ( 'NONE', #29380, #1538 ) ;
#24085 = FACE_OUTER_BOUND ( 'NONE', #6996, .T. ) ;
#24086 = CARTESIAN_POINT ( 'NONE',  ( 13.49999999999999645, 198.9500000000000171, -23.38268590217984766 ) ) ;
#24087 = CARTESIAN_POINT ( 'NONE',  ( -0.1745138560723084320, 17.98981371789853867, -9.500000000000005329 ) ) ;
#24088 = CARTESIAN_POINT ( 'NONE',  ( 13.62178482187501416, 196.4093750006145456, 23.59362340125806767 ) ) ;
#24090 = ORIENTED_EDGE ( 'NONE', *, *, #16832, .T. ) ;
#24089 = ORIENTED_EDGE ( 'NONE', *, *, #35141, .F. ) ;
#24091 = CARTESIAN_POINT ( 'NONE',  ( 23.87821517812500005, 247.6468750006145285, 4.985214923628404016 ) ) ;
#24092 = CARTESIAN_POINT ( 'NONE',  ( 2.660918448318003282, 31.50231371789854862, 12.46528703574811558 ) ) ;
#24093 = CARTESIAN_POINT ( 'NONE',  ( 26.75643035624999655, 3.323476615752271712, -2.578124999385477345 ) ) ;
#24094 = CARTESIAN_POINT ( 'NONE',  ( 0.1745138560722461762, 132.9898137178985564, 15.50000000000000533 ) ) ;
#24095 = EDGE_CURVE ( 'NONE', #1464, #31223, #35941, .T. ) ;
#24096 = CARTESIAN_POINT ( 'NONE',  ( 26.99999999999999645, 7.347880794884117764E-16, -8.268749998770946519 ) ) ;
#24097 = DIRECTION ( 'NONE',  ( -1.000000000000000000, -6.123233995736766036E-17, 0.000000000000000000 ) ) ;
#24098 = ORIENTED_EDGE ( 'NONE', *, *, #36365, .T. ) ;
#24099 = CARTESIAN_POINT ( 'NONE',  ( 19.68408634441911431, 5.407089921784862696, -5.296874999385526195 ) ) ;
#24100 = ORIENTED_EDGE ( 'NONE', *, *, #19130, .T. ) ;
#24101 = VECTOR ( 'NONE', #23041, 1000.000000000000000 ) ;
#24102 = CARTESIAN_POINT ( 'NONE',  ( 27.24356964374999635, 196.4656250006145228, -15.72908226750539029 ) ) ;
#24103 = CARTESIAN_POINT ( 'NONE',  ( -10.49813415415989581, 133.1726862821014663, -7.228626920339068285 ) ) ;
#24104 = CARTESIAN_POINT ( 'NONE',  ( 27.81522707900330715, 5.407089921784862696, 163.7168658290902101 ) ) ;
#24105 = ADVANCED_FACE ( 'NONE', ( #15122 ), #12276, .F. ) ;
#24106 = CARTESIAN_POINT ( 'NONE',  ( -49.99627896937850835, 201.4690446883607251, -2.162041339862721845 ) ) ;
#24107 = VECTOR ( 'NONE', #1885, 1000.000000000000000 ) ;
#24108 = CARTESIAN_POINT ( 'NONE',  ( 20.99999999999999645, 247.6093750006145342, 6.646953231504538984 ) ) ;
#24109 = CARTESIAN_POINT ( 'NONE',  ( 26.99999999999999289, 0.000000000000000000, -8.000000000000000000 ) ) ;
#24110 = CARTESIAN_POINT ( 'NONE',  ( -45.24627896937850835, 205.4690446883607535, -1.090244570138286351 ) ) ;
#24111 =( BOUNDED_CURVE ( )  B_SPLINE_CURVE ( 2, ( #16122, #992, #12568, #34101, #28230, #31263, #4732 ),
 .UNSPECIFIED., .F., .F. ) 
 B_SPLINE_CURVE_WITH_KNOTS ( ( 3, 2, 2, 3 ),
 ( 0.4347826086956515512, 0.4420289855072456753, 0.4492753623188397993, 0.4565217391304338679 ),
 .UNSPECIFIED. ) 
 CURVE ( )  GEOMETRIC_REPRESENTATION_ITEM ( )  RATIONAL_B_SPLINE_CURVE ( ( 1.000000000000011102, 0.8660254037844272723, 1.000000000000000000, 0.8660254037844387076, 1.000000000000000000, 0.8660254037844551389, 0.9999999999999835687 ) ) 
 REPRESENTATION_ITEM ( '' )  );
#24112 = DIRECTION ( 'NONE',  ( 1.000000000000000000, 0.000000000000000000, 0.000000000000000000 ) ) ;
#24113 = CARTESIAN_POINT ( 'NONE',  ( 37.33614145406145468, 3.604726614523238837, 165.0860235234823392 ) ) ;
#24114 = VERTEX_POINT ( 'NONE', #35580 ) ;
#24115 = CARTESIAN_POINT ( 'NONE',  ( 25.32790894457507846, -3.464101615137821888, 168.3105050721087537 ) ) ;
#24116 = CARTESIAN_POINT ( 'NONE',  ( -8.927990412390661490, 130.8726862821014834, 13.04141134922759804 ) ) ;
#24117 = CARTESIAN_POINT ( 'NONE',  ( -45.05580436395490551, 218.5000000000000000, 0.1155267958017064944 ) ) ;
#24118 = CARTESIAN_POINT ( 'NONE',  ( -5.529263428287477744, 130.8726862821014834, 7.954856959092191815 ) ) ;
#24119 = CARTESIAN_POINT ( 'NONE',  ( 19.39230484541323918, 241.3575961894323427, -5.999999999999987566 ) ) ;
#24120 = CARTESIAN_POINT ( 'NONE',  ( -12.53471296425194836, 21.62268628210144072, 2.311890736173176641 ) ) ;
#24121 = CARTESIAN_POINT ( 'NONE',  ( 13.56230152254411792, -5.196152422706638241, -7.125000000000075495 ) ) ;
#24122 = EDGE_LOOP ( 'NONE', ( #9017, #16999, #8244, #28370 ) ) ;
#24123 = CARTESIAN_POINT ( 'NONE',  ( 22.56230152254412502, 7.347880794884125653E-16, -3.375000000000044409 ) ) ;
#24124 = CARTESIAN_POINT ( 'NONE',  ( 10.83675517735155225, 128.8601862821014663, 11.08355503943142573 ) ) ;
#24125 = CARTESIAN_POINT ( 'NONE',  ( 22.56230152254410370, 8.572527594031469245E-16, 10.00000000000000000 ) ) ;
#24126 = CARTESIAN_POINT ( 'NONE',  ( -1.715153634034442431, 142.4773137178985678, 9.534712964251900402 ) ) ;
#24127 = CARTESIAN_POINT ( 'NONE',  ( -27.24356964375000345, 199.3531250006145399, 0.000000000000000000 ) ) ;
#24128 = DIRECTION ( 'NONE',  ( 1.000000000000000000, 0.000000000000000000, 0.000000000000000000 ) ) ;
#24129 = CARTESIAN_POINT ( 'NONE',  ( -27.24356964374999990, 199.3718750006145513, -15.72908226750537786 ) ) ;
#24130 = DIRECTION ( 'NONE',  ( 1.000000000000000000, 0.000000000000000000, 0.000000000000000000 ) ) ;
#24131 = CARTESIAN_POINT ( 'NONE',  ( -47.00000000000000711, 244.5000000000000000, 5.000000000000000000 ) ) ;
#24132 =( BOUNDED_CURVE ( )  B_SPLINE_CURVE ( 2, ( #2443, #8695, #14571, #25942, #3185, #29144, #26305, #22740, #34839 ),
 .UNSPECIFIED., .F., .F. ) 
 B_SPLINE_CURVE_WITH_KNOTS ( ( 3, 2, 2, 2, 3 ),
 ( 0.3125000000000000000, 0.3194444444444444198, 0.3333333333333333148, 0.3472222222222222099, 0.3541666666666666852 ),
 .UNSPECIFIED. ) 
 CURVE ( )  GEOMETRIC_REPRESENTATION_ITEM ( )  RATIONAL_B_SPLINE_CURVE ( ( 0.9330127018922194093, 0.9330127018922194093, 1.000000000000000000, 0.8660254037844387076, 1.000000000000000000, 0.8660254037844387076, 1.000000000000000000, 0.9330127018922190762, 0.9330127018922194093 ) ) 
 REPRESENTATION_ITEM ( '' )  );
#24133 = CARTESIAN_POINT ( 'NONE',  ( -7.954856959092309943, 70.02731371789855075, 5.529263428287300108 ) ) ;
#24135 = DIRECTION ( 'NONE',  ( 0.000000000000000000, 0.000000000000000000, 1.000000000000000000 ) ) ;
#24134 = B_SPLINE_CURVE_WITH_KNOTS ( 'NONE', 3,
 ( #10566, #5062, #24784, #19119 ),
 .UNSPECIFIED., .F., .F.,
 ( 4, 4 ),
 ( 0.000000000000000000, 1.000000000000000000 ),
 .UNSPECIFIED. ) ;
#24136 = ORIENTED_EDGE ( 'NONE', *, *, #26746, .F. ) ;
#24137 = CARTESIAN_POINT ( 'NONE',  ( 18.00000000000000355, 243.3812500012290343, 5.196152422706632912 ) ) ;
#24138 = CARTESIAN_POINT ( 'NONE',  ( -7.228626920338836470, 72.32731371789854791, -10.49813415416005213 ) ) ;
#24139 = CARTESIAN_POINT ( 'NONE',  ( 19.68408634441912142, -5.407089921784861808, -3.196874999385534988 ) ) ;
#24140 = CARTESIAN_POINT ( 'NONE',  ( 15.00000000000000000, 242.7999999999999829, 0.000000000000000000 ) ) ;
#24141 = CARTESIAN_POINT ( 'NONE',  ( 26.75643035624999655, 3.323476615752271712, -4.040624999385487470 ) ) ;
#24142 = CARTESIAN_POINT ( 'NONE',  ( -12.46528703574811558, 43.00231371789854506, 2.660918448318003726 ) ) ;
#24143 = ORIENTED_EDGE ( 'NONE', *, *, #5092, .T. ) ;
#24144 = CARTESIAN_POINT ( 'NONE',  ( 26.99999999999999645, 7.347880794884117764E-16, -6.975000000000008527 ) ) ;
#24145 = CARTESIAN_POINT ( 'NONE',  ( 18.12178482187500350, 244.4218750006145058, 4.985214923628407568 ) ) ;
#24146 = CARTESIAN_POINT ( 'NONE',  ( 10.49813415415989581, 18.17268628210144854, 7.228626920339068285 ) ) ;
#24147 = CARTESIAN_POINT ( 'NONE',  ( -36.34002896937850124, 204.4285982733020433, 3.350049139982171020 ) ) ;
#24148 = CARTESIAN_POINT ( 'NONE',  ( -67.01711230271183695, 216.4690446883607535, -1.857196546604089393 ) ) ;
#24149 = CARTESIAN_POINT ( 'NONE',  ( 24.63175244948523002, -3.464101615137757051, 160.3533999223253375 ) ) ;
#24150 = CARTESIAN_POINT ( 'NONE',  ( 12.53471296425189330, 84.97731371789855359, 2.311890736173451977 ) ) ;
#24151 = CARTESIAN_POINT ( 'NONE',  ( -52.37872103062156981, 205.4690446883607535, 1.090244570138264368 ) ) ;
#24152 = CARTESIAN_POINT ( 'NONE',  ( -36.54538769728824121, 212.3930949314662371, -8.469044688360781947 ) ) ;
#24153 = CARTESIAN_POINT ( 'NONE',  ( 26.75643035624999655, 7.049594010296217766E-16, -6.778124999385487293 ) ) ;
#24154 = CARTESIAN_POINT ( 'NONE',  ( 13.56230152254410726, 5.196152422706630247, -0.8624999987709991434 ) ) ;
#24155 = CARTESIAN_POINT ( 'NONE',  ( -14.25334919248795096, 61.11481371789854933, 6.092822981423662299 ) ) ;
#24156 = CARTESIAN_POINT ( 'NONE',  ( -40.10044563604517265, 203.6929966515019430, -6.137860380172892150 ) ) ;
#24157 = CARTESIAN_POINT ( 'NONE',  ( 5.438367727407757144E-14, 198.0875000000000057, -27.00000000000000000 ) ) ;
#24158 = CARTESIAN_POINT ( 'NONE',  ( -4.944772684328673229, 84.58518628210146062, 11.48171059495397728 ) ) ;
#24159 = CARTESIAN_POINT ( 'NONE',  ( -11.08355503943142573, 20.76018628210144001, 10.83675517735155402 ) ) ;
#24160 = CARTESIAN_POINT ( 'NONE',  ( 10.56230152254410726, 3.464101615137757051, -0.9375000000000204281 ) ) ;
#24161 = CARTESIAN_POINT ( 'NONE',  ( 33.70166733926387082, -5.407089921784861808, 159.3622581591915548 ) ) ;
#24162 = ORIENTED_EDGE ( 'NONE', *, *, #18177, .F. ) ;
#24163 = CARTESIAN_POINT ( 'NONE',  ( 15.50000000000000533, 44.91018628210144215, 0.1745138560725827404 ) ) ;
#24164 = CARTESIAN_POINT ( 'NONE',  ( -1.926257025242585782E-15, 197.8906250006145342, -31.45816453501076637 ) ) ;
#24165 = CARTESIAN_POINT ( 'NONE',  ( 24.58926402489574770, 0.000000000000000000, 159.8677550070055702 ) ) ;
#24166 = CARTESIAN_POINT ( 'NONE',  ( 26.99999999999958078, -3.464101615137992862, -1.106249998770966636 ) ) ;
#24167 = CARTESIAN_POINT ( 'NONE',  ( -33.97247103062156270, 206.6499508600178672, 5.571401726697986057 ) ) ;
#24168 = ADVANCED_FACE ( 'NONE', ( #9625 ), #7350, .T. ) ;
#24169 = PLANE ( 'NONE',  #28099 ) ;
#24170 = CARTESIAN_POINT ( 'NONE',  ( -10.69584247140444866, 21.04768628210144854, 6.932735513423972762 ) ) ;
#24171 = CARTESIAN_POINT ( 'NONE',  ( 19.39230484541326760, 247.4486538117967314, 5.999999999999999112 ) ) ;
#24172 = CARTESIAN_POINT ( 'NONE',  ( -7.954856959092309943, 125.2273137178985394, 5.529263428287300108 ) ) ;
#24173 = CARTESIAN_POINT ( 'NONE',  ( 20.99999999999999645, 246.3718750006144944, 6.646953231504538984 ) ) ;
#24174 = EDGE_LOOP ( 'NONE', ( #18964, #10513, #21454, #34888 ) ) ;
#24175 = CARTESIAN_POINT ( 'NONE',  ( 24.00000000000000000, -5.196152422706629359, -7.500000000000007105 ) ) ;
#24176 = FACE_OUTER_BOUND ( 'NONE', #10570, .T. ) ;
#24177 = CARTESIAN_POINT ( 'NONE',  ( 10.69584247140429589, 131.5523137178985849, 6.932735513424201024 ) ) ;
#24178 = CARTESIAN_POINT ( 'NONE',  ( 19.68408634441910721, 5.407089921784857367, -7.040624999385541649 ) ) ;
#24179 = CARTESIAN_POINT ( 'NONE',  ( 37.21521286099908110, 7.646167579472015790E-16, 163.7038033798800711 ) ) ;
#24180 = CARTESIAN_POINT ( 'NONE',  ( 34.39497977834484743, 5.196152422706637353, 168.6841797239115976 ) ) ;
#24181 = CARTESIAN_POINT ( 'NONE',  ( -27.00000000000000355, 199.9625000000000341, -15.58845726811989429 ) ) ;
#24182 = CARTESIAN_POINT ( 'NONE',  ( -11.61527771782819940, 58.13518628210144357, 4.622313124798574258 ) ) ;
#24183 = ORIENTED_EDGE ( 'NONE', *, *, #29640, .F. ) ;
#24184 = ORIENTED_EDGE ( 'NONE', *, *, #14345, .T. ) ;
#24185 = CARTESIAN_POINT ( 'NONE',  ( 1.069080835302379631E-14, 196.6250000012290400, 27.00000000000000000 ) ) ;
#24186 = DIRECTION ( 'NONE',  ( 0.000000000000000000, 0.000000000000000000, 1.000000000000000000 ) ) ;
#24187 = CARTESIAN_POINT ( 'NONE',  ( 29.54925929127992745, 5.908847637349538218, 159.6727443940304738 ) ) ;
#24188 = LINE ( 'NONE', #6183, #772 ) ;
#24189 = CARTESIAN_POINT ( 'NONE',  ( 18.12178482187499640, 4.985214923628404904, -8.315624999385457627 ) ) ;
#24190 = CARTESIAN_POINT ( 'NONE',  ( -6.932735513423968321, 78.54768628210146630, -10.69584247140445221 ) ) ;
#24191 = CARTESIAN_POINT ( 'NONE',  ( -11.08355503943118592, 16.83981371789855430, -10.83675517735179383 ) ) ;
#24192 = CARTESIAN_POINT ( 'NONE',  ( 24.78863278643148149, -3.464101615138032830, 162.1465503788903959 ) ) ;
#24193 = EDGE_CURVE ( 'NONE', #24223, #31540, #18352, .T. ) ;
#24194 = CARTESIAN_POINT ( 'NONE',  ( 17.52409618574002792, 213.4759038142795191, 5.188047882455193438 ) ) ;
#24195 = CARTESIAN_POINT ( 'NONE',  ( -35.95163769728824121, 213.9548777149308592, -2.149950860017830756 ) ) ;
#24196 = CARTESIAN_POINT ( 'NONE',  ( -27.24356964375000345, 199.8312500006145171, 0.000000000000000000 ) ) ;
#24197 = CARTESIAN_POINT ( 'NONE',  ( 25.33444562538816669, 0.000000000000000000, 168.3852196756899957 ) ) ;
#24198 = CARTESIAN_POINT ( 'NONE',  ( 11.61527771782809637, 140.4648137178985792, 4.622313124798827388 ) ) ;
#24199 = CARTESIAN_POINT ( 'NONE',  ( -49.40997103062156981, 215.5714017266979852, 3.350049139982118618 ) ) ;
#24200 = CARTESIAN_POINT ( 'NONE',  ( -65.83705436395491972, 203.8621396198270475, -6.307003348497942419 ) ) ;
#24201 = ADVANCED_FACE ( 'NONE', ( #29901 ), #27059, .F. ) ;
#24202 = CARTESIAN_POINT ( 'NONE',  ( 18.12178482187499640, 4.985214923628404904, -0.3281249993854762348 ) ) ;
#24203 = CARTESIAN_POINT ( 'NONE',  ( 27.24356964374999635, 197.8156250006145171, -15.72908226750539029 ) ) ;
#24204 = CARTESIAN_POINT ( 'NONE',  ( -2.908627838312453306, 105.6773137178985706, 15.53471296425188797 ) ) ;
#24205 = CARTESIAN_POINT ( 'NONE',  ( -40.10044563604517265, 205.1570982666397072, -4.673758765035155527 ) ) ;
#24206 = EDGE_LOOP ( 'NONE', ( #33008, #5889, #10889, #8366 ) ) ;
#24207 = CARTESIAN_POINT ( 'NONE',  ( 8.962234695871762469, 34.56018628210144783, -8.715434833791931624 ) ) ;
#24208 = CARTESIAN_POINT ( 'NONE',  ( 20.99999999999999645, -6.928203230275506996, -6.187500000000013323 ) ) ;
#24209 = FACE_OUTER_BOUND ( 'NONE', #21745, .T. ) ;
#24210 = CARTESIAN_POINT ( 'NONE',  ( 31.29445502703164905, -7.209453229046482114, 167.6661593874051164 ) ) ;
#24211 = AXIS2_PLACEMENT_3D ( 'NONE', #36362, #21985, #2244 ) ;
#24212 = CARTESIAN_POINT ( 'NONE',  ( 5.770363421893814682, 101.8351862821014606, 14.38691631536207183 ) ) ;
#24213 = CARTESIAN_POINT ( 'NONE',  ( -56.93080436395490551, 203.5000000000000000, -0.1155267958017335561 ) ) ;
#24214 = CARTESIAN_POINT ( 'NONE',  ( 16.56230152254410726, 7.209453229046475009, -5.203124999385489780 ) ) ;
#24215 = CARTESIAN_POINT ( 'NONE',  ( -9.500000000000005329, 40.31018628210145494, -0.1745138560725176813 ) ) ;
#24216 = CARTESIAN_POINT ( 'NONE',  ( 1.069080835302379631E-14, 198.8750000012290400, 27.00000000000000000 ) ) ;
#24217 = CARTESIAN_POINT ( 'NONE',  ( -39.31622103062156981, 212.1620413398628671, 8.530955311639223382 ) ) ;
#24218 = CARTESIAN_POINT ( 'NONE',  ( 16.56230152254411436, -7.209453229046482114, -9.534374999385541116 ) ) ;
#24219 = CARTESIAN_POINT ( 'NONE',  ( 10.69584247140445221, 71.64768628210146062, -6.932735513423970097 ) ) ;
#24220 = FACE_OUTER_BOUND ( 'NONE', #15941, .T. ) ;
#24221 = DIRECTION ( 'NONE',  ( 0.000000000000000000, 0.000000000000000000, -1.000000000000000000 ) ) ;
#24223 = VERTEX_POINT ( 'NONE', #12655 ) ;
#24222 = CARTESIAN_POINT ( 'NONE',  ( -8.710071997420127943, 40.88518628210145067, -3.796722387233380402 ) ) ;
#24224 = DIRECTION ( 'NONE',  ( -0.8083506638593008775, -0.5887012860850803220, 0.000000000000000000 ) ) ;
#24225 = CARTESIAN_POINT ( 'NONE',  ( 21.00000000000000000, 6.646953231504538984, -9.253124999385450522 ) ) ;
#24226 = AXIS2_PLACEMENT_3D ( 'NONE', #25054, #30752, #10461 ) ;
#24228 = EDGE_CURVE ( 'NONE', #27974, #9824, #27621, .T. ) ;
#24227 = CARTESIAN_POINT ( 'NONE',  ( 10.56230152254410548, 0.000000000000000000, -6.750000000000061284 ) ) ;
#24229 = CARTESIAN_POINT ( 'NONE',  ( 24.75434669616370442, -3.604726614523244610, 164.5493068216156303 ) ) ;
#24230 = CARTESIAN_POINT ( 'NONE',  ( 27.99292734389955939, 5.196152422706636465, 164.3506650272002219 ) ) ;
#24231 = CARTESIAN_POINT ( 'NONE',  ( 26.99999999999999645, 247.0749999999999886, -7.347880794884117764E-16 ) ) ;
#24232 = CARTESIAN_POINT ( 'NONE',  ( -27.24356964374999279, 195.7906250006145399, 15.72908226750539384 ) ) ;
#24233 = CARTESIAN_POINT ( 'NONE',  ( -2.311890736173448424, 105.6773137178985564, 12.53471296425189330 ) ) ;
#24234 = CARTESIAN_POINT ( 'NONE',  ( 4.622313124798573369, 101.8351862821014464, 11.61527771782819940 ) ) ;
#24235 = ORIENTED_EDGE ( 'NONE', *, *, #28917, .F. ) ;
#24236 = EDGE_LOOP ( 'NONE', ( #30826, #14291, #7222, #28501 ) ) ;
#24237 = CARTESIAN_POINT ( 'NONE',  ( 27.24356964375000700, 195.9406250006145456, 15.72908226750537075 ) ) ;
#24238 = CARTESIAN_POINT ( 'NONE',  ( 24.98146486726017912, 0.000000000000000000, 164.3506311484184437 ) ) ;
#24239 = EDGE_CURVE ( 'NONE', #8675, #22401, #2289, .T. ) ;
#24240 = CARTESIAN_POINT ( 'NONE',  ( 10.83675517735179206, 83.53981371789856780, -11.08355503943118769 ) ) ;
#24241 = CARTESIAN_POINT ( 'NONE',  ( 26.75643035624999655, 3.323476615752271712, -6.290624999385498128 ) ) ;
#24242 = CARTESIAN_POINT ( 'NONE',  ( 21.00000000000000000, 245.0218750006145285, 6.646953231504538984 ) ) ;
#24243 =( GEOMETRIC_REPRESENTATION_CONTEXT ( 3 ) GLOBAL_UNCERTAINTY_ASSIGNED_CONTEXT ( ( #160 ) ) GLOBAL_UNIT_ASSIGNED_CONTEXT ( ( #19760, #28076, #16902 ) ) REPRESENTATION_CONTEXT ( 'NONE', 'WORKASPACE' ) );
#24244 = CARTESIAN_POINT ( 'NONE',  ( -9.500000000000005329, 95.51018628210147199, -0.1745138560725176813 ) ) ;
#24245 = ADVANCED_FACE ( 'NONE', ( #24220 ), #21575, .T. ) ;
#24246 = CARTESIAN_POINT ( 'NONE',  ( 24.93243976185750554, 0.000000000000000000, 163.7902716295174912 ) ) ;
#24247 = CARTESIAN_POINT ( 'NONE',  ( -5.233372021372612259, 60.25231371789854506, 8.152565276336593669 ) ) ;
#24248 = CARTESIAN_POINT ( 'NONE',  ( 13.44051670066911441, -5.407089921784859143, -8.165624999385528326 ) ) ;
#24249 = CARTESIAN_POINT ( 'NONE',  ( 6.840914352311949109, 113.4398137178985593, 6.594114490232462877 ) ) ;
#24250 = CARTESIAN_POINT ( 'NONE',  ( 18.12178482187499640, 240.6718750006145058, -4.985214923628404904 ) ) ;
#24251 = CARTESIAN_POINT ( 'NONE',  ( 8.962234695871567070, 30.63981371789854791, 8.715434833792127023 ) ) ;
#24252 = DIRECTION ( 'NONE',  ( 0.000000000000000000, 0.000000000000000000, 1.000000000000000000 ) ) ;
#24253 = VECTOR ( 'NONE', #9678, 1000.000000000000000 ) ;
#24254 = CARTESIAN_POINT ( 'NONE',  ( -11.48171059495397373, 86.88518628210145778, -4.944772684328680334 ) ) ;
#24255 = CARTESIAN_POINT ( 'NONE',  ( 10.56230152254411081, 0.000000000000000000, -5.287499998771011178 ) ) ;
#24256 = EDGE_CURVE ( 'NONE', #17042, #31449, #6159, .T. ) ;
#24257 = LINE ( 'NONE', #1119, #19561 ) ;
#24258 = CARTESIAN_POINT ( 'NONE',  ( 30.96598682155142868, 7.209453229046475009, 163.9117506189718370 ) ) ;
#24259 = CARTESIAN_POINT ( 'NONE',  ( 16.56230152254411436, -7.209453229046482114, -4.134374999385496352 ) ) ;
#24260 = CARTESIAN_POINT ( 'NONE',  ( 20.99999999999998579, 248.5374999999999659, -5.999999999999997335 ) ) ;
#24261 = FACE_OUTER_BOUND ( 'NONE', #14390, .T. ) ;
#24262 = CARTESIAN_POINT ( 'NONE',  ( 27.00000000000000355, 198.4250000000000114, -3.306546357697854128E-15 ) ) ;
#24263 = CARTESIAN_POINT ( 'NONE',  ( -9.500000000000005329, 104.7101862821014606, -0.1745138560725176813 ) ) ;
#24264 = CARTESIAN_POINT ( 'NONE',  ( 7.234628195640322446, 198.8950961906613770, 26.99999999999999645 ) ) ;
#24265 = CARTESIAN_POINT ( 'NONE',  ( 2.311890736173175753, 138.9226862821014663, 12.53471296425194836 ) ) ;
#24266 = CARTESIAN_POINT ( 'NONE',  ( -6.804952097069882910, 143.0000000000000284, 9.842932490202064955 ) ) ;
#24267 = CARTESIAN_POINT ( 'NONE',  ( 18.12178482187499640, 240.6718750006145058, -4.985214923628404904 ) ) ;
#24268 = ORIENTED_EDGE ( 'NONE', *, *, #26246, .T. ) ;
#24269 = CARTESIAN_POINT ( 'NONE',  ( 31.24052741120653209, 7.209453229046475009, 167.0497639179608313 ) ) ;
#24270 = CARTESIAN_POINT ( 'NONE',  ( 18.12178482187500350, -4.985214923628407568, -3.215624999385463312 ) ) ;
#24271 = ADVANCED_FACE ( 'NONE', ( #4122 ), #10042, .T. ) ;
#24272 = CARTESIAN_POINT ( 'NONE',  ( -27.24356964375000345, 199.4093750006145456, 0.000000000000000000 ) ) ;
#24273 = DIRECTION ( 'NONE',  ( 0.9961946980917462113, 0.000000000000000000, -0.08715574274765118534 ) ) ;
#24274 = CARTESIAN_POINT ( 'NONE',  ( 20.99999999999999645, 185.0294372515228645, 0.000000000000000000 ) ) ;
#24275 = CARTESIAN_POINT ( 'NONE',  ( 20.99999999999999645, 185.0294372515228645, 5.999999999999999112 ) ) ;
#24276 = CARTESIAN_POINT ( 'NONE',  ( 10.31873187879410736, 3.604726614523236616, -0.1781249993854788494 ) ) ;
#24277 = CARTESIAN_POINT ( 'NONE',  ( -6.840914352311947333, 16.83981371789855430, -6.594114490232462877 ) ) ;
#24278 = CARTESIAN_POINT ( 'NONE',  ( 5.778771075727756162E-15, 197.2718750006145569, 31.45816453501076637 ) ) ;
#24280 = EDGE_LOOP ( 'NONE', ( #10846, #16911, #26881, #9235, #8628, #2479 ) ) ;
#24279 = ORIENTED_EDGE ( 'NONE', *, *, #13410, .F. ) ;
#24281 = CARTESIAN_POINT ( 'NONE',  ( 18.12178482187500350, 248.0218750006145001, 4.985214923628407568 ) ) ;
#24282 = CARTESIAN_POINT ( 'NONE',  ( 11.48171059495408208, 28.91481371789854293, -4.944772684328420986 ) ) ;
#24283 = CARTESIAN_POINT ( 'NONE',  ( 21.00000000000000000, 6.646953231504538984, -2.503124999385450966 ) ) ;
#24284 = CARTESIAN_POINT ( 'NONE',  ( -8.927990412390371944, 136.7273137178985110, -13.04141134922778988 ) ) ;
#24285 = CARTESIAN_POINT ( 'NONE',  ( 19.95811728174978228, 5.908847637349563087, -10.39322646479281254 ) ) ;
#24286 = CARTESIAN_POINT ( 'NONE',  ( 20.99999999999999645, 250.0000000000000000, 0.000000000000000000 ) ) ;
#24287 = ORIENTED_EDGE ( 'NONE', *, *, #30910, .F. ) ;
#24288 = CARTESIAN_POINT ( 'NONE',  ( 22.80587116629411781, -3.604726614523238837, -7.209374999385536498 ) ) ;
#24289 = EDGE_CURVE ( 'NONE', #36103, #36641, #7001, .T. ) ;
#24290 = VERTEX_POINT ( 'NONE', #8739 ) ;
#24291 = CARTESIAN_POINT ( 'NONE',  ( -27.24356964374999635, 195.3406250006145513, 15.72908226750539384 ) ) ;
#24292 = CARTESIAN_POINT ( 'NONE',  ( -2.660918448318275509, 130.2976862821014379, 12.46528703574805874 ) ) ;
#24293 = CARTESIAN_POINT ( 'NONE',  ( 34.05464809739185483, -5.407089921784861808, 163.3968466864631068 ) ) ;
#24294 = VECTOR ( 'NONE', #21724, 1000.000000000000000 ) ;
#24295 = CARTESIAN_POINT ( 'NONE',  ( -50.98586230271183695, 205.8500491399821613, 7.418979330068642852 ) ) ;
#24296 = CARTESIAN_POINT ( 'NONE',  ( 18.12178482187500350, 246.2218750006145171, 4.985214923628407568 ) ) ;
#24297 = DIRECTION ( 'NONE',  ( 0.000000000000000000, 1.000000000000000000, 0.000000000000000000 ) ) ;
#24298 = CARTESIAN_POINT ( 'NONE',  ( -45.84002896937850124, 206.1606490808709111, 2.350049139982143931 ) ) ;
#24299 = CARTESIAN_POINT ( 'NONE',  ( 8.715434833791931624, 128.8601862821014663, 8.962234695871760692 ) ) ;
#24300 = CARTESIAN_POINT ( 'NONE',  ( 24.94881294716939379, 3.604726614523236616, 166.7720662417328299 ) ) ;
#24301 = VERTEX_POINT ( 'NONE', #11575 ) ;
#24302 = CARTESIAN_POINT ( 'NONE',  ( -27.99076334771182673, 207.4091998227514182, 7.586839709977279078 ) ) ;
#24303 = CARTESIAN_POINT ( 'NONE',  ( -15.50000000000000533, 141.5101862821014720, -0.1745138560725808530 ) ) ;
#24304 = CARTESIAN_POINT ( 'NONE',  ( -47.03497103062157692, 202.6965474657331185, -4.350049139982091084 ) ) ;
#24305 = CARTESIAN_POINT ( 'NONE',  ( 6.840914352312096547, 117.3601862821014663, -6.594114490232313663 ) ) ;
#24306 = EDGE_CURVE ( 'NONE', #27046, #7496, #26943, .T. ) ;
#24307 = CARTESIAN_POINT ( 'NONE',  ( 15.00000000000000000, 249.1562500012290400, 0.000000000000000000 ) ) ;
#24308 = CARTESIAN_POINT ( 'NONE',  ( 12.50000000000000355, 26.51018628210144357, 0.1745138560725507937 ) ) ;
#24309 = CARTESIAN_POINT ( 'NONE',  ( 22.56230152254412147, -3.464101615137755275, -7.462500000000038547 ) ) ;
#24310 = VERTEX_POINT ( 'NONE', #20497 ) ;
#24311 = CARTESIAN_POINT ( 'NONE',  ( -33.18080436395490551, 203.5000000000000000, -0.1155267958017335561 ) ) ;
#24312 = CARTESIAN_POINT ( 'NONE',  ( -5.770363421893818234, 115.6351862821014436, -14.38691631536207005 ) ) ;
#24313 = CARTESIAN_POINT ( 'NONE',  ( 13.56230152254411436, -5.196152422706632912, -6.112499998771031784 ) ) ;
#24314 = CARTESIAN_POINT ( 'NONE',  ( 3.474262827703335166, 9.835186282101449962, 8.843639120294326972 ) ) ;
#24315 = CARTESIAN_POINT ( 'NONE',  ( 13.62178482187501416, 199.0531250006145285, 23.59362340125806767 ) ) ;
#24316 = FACE_OUTER_BOUND ( 'NONE', #8980, .T. ) ;
#24317 = CARTESIAN_POINT ( 'NONE',  ( -27.00000000000000355, 196.3625000000000114, -15.58845726811989429 ) ) ;
#24318 = CARTESIAN_POINT ( 'NONE',  ( 10.56230152254410726, 0.000000000000000000, -5.400000000000043876 ) ) ;
#24319 = EDGE_CURVE ( 'NONE', #16861, #5932, #6066, .T. ) ;
#24320 = FACE_OUTER_BOUND ( 'NONE', #2630, .T. ) ;
#24321 = CARTESIAN_POINT ( 'NONE',  ( -9.000000000000024869, 204.5000000000000000, 0.000000000000000000 ) ) ;
#24322 = CARTESIAN_POINT ( 'NONE',  ( 8.710071997420211432, 74.91481371789855359, -3.796722387233181895 ) ) ;
#24323 = ORIENTED_EDGE ( 'NONE', *, *, #12839, .F. ) ;
#24324 = CARTESIAN_POINT ( 'NONE',  ( 21.00000000000000000, 243.8687500012290172, 6.928203230275506996 ) ) ;
#24325 = CARTESIAN_POINT ( 'NONE',  ( -8.962234695871565293, 72.03981371789855359, -8.715434833792128799 ) ) ;
#24326 = CARTESIAN_POINT ( 'NONE',  ( 19.68408634441911786, -5.407089921784861808, -4.546874999385525307 ) ) ;
#24327 = DIRECTION ( 'NONE',  ( 0.000000000000000000, -0.000000000000000000, -1.000000000000000000 ) ) ;
#24328 = CARTESIAN_POINT ( 'NONE',  ( 26.75643035624999655, 3.323476615752271712, -3.590624999385491734 ) ) ;
#24329 = CARTESIAN_POINT ( 'NONE',  ( 10.69584247140429589, 48.75231371789854506, 6.932735513424201024 ) ) ;
#24330 =( REPRESENTATION_RELATIONSHIP ('NONE','NONE', #4304, #4527 ) REPRESENTATION_RELATIONSHIP_WITH_TRANSFORMATION ( #15676 )SHAPE_REPRESENTATION_RELATIONSHIP( ) );
#24331 = ORIENTED_EDGE ( 'NONE', *, *, #15931, .T. ) ;
#24332 = CARTESIAN_POINT ( 'NONE',  ( 26.75643035624999655, -3.323476615752267271, -7.603124999385488358 ) ) ;
#24333 = CARTESIAN_POINT ( 'NONE',  ( 26.75643035624999655, 244.5718750006145115, -7.049594010296217766E-16 ) ) ;
#24334 = CARTESIAN_POINT ( 'NONE',  ( -12.46528703574805697, 12.99768628210143362, -2.660918448318280838 ) ) ;
#24335 =( BOUNDED_CURVE ( )  B_SPLINE_CURVE ( 2, ( #37446, #16826, #22704, #11313, #26260, #20039, #8107, #11127, #14344 ),
 .UNSPECIFIED., .F., .F. ) 
 B_SPLINE_CURVE_WITH_KNOTS ( ( 3, 2, 2, 2, 3 ),
 ( 0.2291666666666666574, 0.2361111111111111049, 0.2500000000000000000, 0.2638888888888888951, 0.2708333333333333703 ),
 .UNSPECIFIED. ) 
 CURVE ( )  GEOMETRIC_REPRESENTATION_ITEM ( )  RATIONAL_B_SPLINE_CURVE ( ( 0.9330127018922194093, 0.9330127018922194093, 1.000000000000000000, 0.8660254037844387076, 1.000000000000000000, 0.8660254037844387076, 1.000000000000000000, 0.9330127018922190762, 0.9330127018922194093 ) ) 
 REPRESENTATION_ITEM ( '' )  );
#24336 = CARTESIAN_POINT ( 'NONE',  ( -41.88169563604517265, 210.1155267958017703, 6.500000000000000888 ) ) ;
#24337 = CARTESIAN_POINT ( 'NONE',  ( -53.75669563604516554, 209.8844732041982013, -6.500000000000000888 ) ) ;
#24338 = AXIS2_PLACEMENT_3D ( 'NONE', #12080, #26481, #23463 ) ;
#24339 = CARTESIAN_POINT ( 'NONE',  ( 36.56647878446795374, 3.464101615137755275, 159.0833872022828359 ) ) ;
#24340 = CARTESIAN_POINT ( 'NONE',  ( 12.50000000000000355, 93.88981371789856212, -0.1745138560722771515 ) ) ;
#24341 = CARTESIAN_POINT ( 'NONE',  ( -42.28497103062156270, 206.1606490808709111, -2.350049139982163027 ) ) ;
#24342 = CARTESIAN_POINT ( 'NONE',  ( -56.13913769728823411, 206.8500491399821044, -5.686928522499717253 ) ) ;
#24343 = CARTESIAN_POINT ( 'NONE',  ( 23.87821517812499650, 4.985214923628404904, -5.803124999385484095 ) ) ;
#24344 = CARTESIAN_POINT ( 'NONE',  ( 20.99999999999999645, 246.5124999999999602, 5.999999999999998224 ) ) ;
#24345 = CARTESIAN_POINT ( 'NONE',  ( 3.257655550456945548, 49.90231371789854364, 15.46528703574811736 ) ) ;
#24346 = CARTESIAN_POINT ( 'NONE',  ( -43.26711230271184405, 218.4690446883607535, -2.393094931466363651 ) ) ;
#24347 = CARTESIAN_POINT ( 'NONE',  ( -26.99999999999999645, 198.2375000000000114, 15.58845726811991561 ) ) ;
#24348 = CARTESIAN_POINT ( 'NONE',  ( 10.69584247140445221, 80.84768628210144925, -6.932735513423970097 ) ) ;
#24349 = CARTESIAN_POINT ( 'NONE',  ( -3.257655550457281723, 19.89768628210143930, 15.46528703574804986 ) ) ;
#24350 = CARTESIAN_POINT ( 'NONE',  ( 19.56230152254410370, 5.196152422706631135, -9.937499998770999099 ) ) ;
#24351 =( BOUNDED_CURVE ( )  B_SPLINE_CURVE ( 2, ( #32888, #36101, #7307, #30430, #16030, #6939, #8241 ),
 .UNSPECIFIED., .F., .F. ) 
 B_SPLINE_CURVE_WITH_KNOTS ( ( 3, 2, 2, 3 ),
 ( 0.1739130434782605039, 0.1811594202898547945, 0.1884057971014491129, 0.1956521739130434034 ),
 .UNSPECIFIED. ) 
 CURVE ( )  GEOMETRIC_REPRESENTATION_ITEM ( )  RATIONAL_B_SPLINE_CURVE ( ( 1.000000000000006661, 0.8660254037844320463, 1.000000000000000000, 0.8660254037844387076, 1.000000000000000000, 0.8660254037844402619, 0.9999999999999984457 ) ) 
 REPRESENTATION_ITEM ( '' )  );
#24352 = LINE ( 'NONE', #7472, #1018 ) ;
#24353 = EDGE_LOOP ( 'NONE', ( #26012, #8405, #5065, #2582 ) ) ;
#24354 = CARTESIAN_POINT ( 'NONE',  ( -0.1745138560725817967, 56.41018628210145636, 15.50000000000000533 ) ) ;
#24355 = CARTESIAN_POINT ( 'NONE',  ( 27.24356964375000700, 198.6406250006145342, 15.72908226750537075 ) ) ;
#24356 = DIRECTION ( 'NONE',  ( -0.000000000000000000, -0.000000000000000000, -1.000000000000000000 ) ) ;
#24357 = CARTESIAN_POINT ( 'NONE',  ( -1.045839947578415010E-13, 194.8250000012290570, 27.00000000000000355 ) ) ;
#24358 = CARTESIAN_POINT ( 'NONE',  ( -35.75372103062156981, 216.5309553116391612, -1.626142955000564383 ) ) ;
#24359 = CARTESIAN_POINT ( 'NONE',  ( 11.61527771782819940, 25.93518628210143717, -4.622313124798573369 ) ) ;
#24360 = CARTESIAN_POINT ( 'NONE',  ( 23.87821517812499650, 249.2593750006145399, -4.985214923628404904 ) ) ;
#24361 = CARTESIAN_POINT ( 'NONE',  ( 8.710071997420211432, 139.3148137178985451, -3.796722387233181895 ) ) ;
#24362 = CARTESIAN_POINT ( 'NONE',  ( 23.87821517812499650, 243.8593750006145342, -4.985214923628404904 ) ) ;
#24363 = ORIENTED_EDGE ( 'NONE', *, *, #23535, .F. ) ;
#24364 = DIRECTION ( 'NONE',  ( -0.000000000000000000, -0.000000000000000000, -1.000000000000000000 ) ) ;
#24365 = CARTESIAN_POINT ( 'NONE',  ( 8.715434833792128799, 129.5398137178985678, -8.962234695871567070 ) ) ;
#24366 = CARTESIAN_POINT ( 'NONE',  ( 19.68408634441910721, -5.407089921784855591, -7.190624999385525129 ) ) ;
#24367 = CARTESIAN_POINT ( 'NONE',  ( 27.91164311941789933, -5.407089921784859143, 164.8189062138541772 ) ) ;
#24368 = DIRECTION ( 'NONE',  ( 0.1742906073607703166, -0.9846942592428442609, 0.000000000000000000 ) ) ;
#24369 = CARTESIAN_POINT ( 'NONE',  ( 27.00000000000000355, 197.9750000000000227, -3.306546357697854128E-15 ) ) ;
#24370 = ORIENTED_EDGE ( 'NONE', *, *, #17296, .F. ) ;
#24371 = CARTESIAN_POINT ( 'NONE',  ( 10.49813415415989581, 45.77268628210144641, 7.228626920339069173 ) ) ;
#24372 = ORIENTED_EDGE ( 'NONE', *, *, #10112, .F. ) ;
#24373 = EDGE_LOOP ( 'NONE', ( #2080, #32140, #26628, #35021 ) ) ;
#24374 = CARTESIAN_POINT ( 'NONE',  ( -27.87471972953270338, 210.0000000000000284, 8.000000000000000000 ) ) ;
#24375 = CARTESIAN_POINT ( 'NONE',  ( 15.24356964374999990, 3.323476615752268604, -0.6281249993854746139 ) ) ;
#24376 = CARTESIAN_POINT ( 'NONE',  ( 22.56230152254412147, 7.347880794884125653E-16, -9.225000000000010303 ) ) ;
#24377 = CARTESIAN_POINT ( 'NONE',  ( -3.253724281355068545E-15, 196.2874999999999659, -27.00000000000000000 ) ) ;
#24378 = CARTESIAN_POINT ( 'NONE',  ( 26.75643035624999655, 3.323476615752271712, -7.978124999385458160 ) ) ;
#24379 = CARTESIAN_POINT ( 'NONE',  ( -12.53471296425194836, 76.82268628210145778, 2.311890736173176641 ) ) ;
#24380 = CARTESIAN_POINT ( 'NONE',  ( 8.927990412390371944, 12.52731371789855963, 13.04141134922778811 ) ) ;
#24381 = CARTESIAN_POINT ( 'NONE',  ( -7.234628195640263826, 197.2075961894323370, -27.00000000000003553 ) ) ;
#24382 = CARTESIAN_POINT ( 'NONE',  ( 19.55576478543887831, 211.4442352145762527, 5.894939585073154298 ) ) ;
#24383 = CARTESIAN_POINT ( 'NONE',  ( -50.19419563604517975, 205.4999999999999716, 0.1155267958017633378 ) ) ;
#24384 = CARTESIAN_POINT ( 'NONE',  ( -70.80918835584510873, 215.2843023367891249, 7.500000000000000000 ) ) ;
#24385 = CARTESIAN_POINT ( 'NONE',  ( 28.23805287048444512, 5.196152422706630247, 167.1524626168076111 ) ) ;
#24386 = CARTESIAN_POINT ( 'NONE',  ( -7.228626920338836470, 136.7273137178985678, -10.49813415416005213 ) ) ;
#24387 = CARTESIAN_POINT ( 'NONE',  ( -50.39955436395490551, 214.8429017333601792, -4.673758765035196383 ) ) ;
#24388 = CARTESIAN_POINT ( 'NONE',  ( -63.85788769728821990, 218.4690446883607535, 2.393094931466250408 ) ) ;
#24389 = CARTESIAN_POINT ( 'NONE',  ( 20.99999999999999645, 6.646953231504538984, -0.3656249993854637226 ) ) ;
#24390 = CARTESIAN_POINT ( 'NONE',  ( -27.24356964374999635, 198.0406250006145399, 15.72908226750539384 ) ) ;
#24391 = CARTESIAN_POINT ( 'NONE',  ( -3.257655550456946880, 109.7023137178985479, -15.46528703574811736 ) ) ;
#24392 = CARTESIAN_POINT ( 'NONE',  ( -48.41294563604515133, 214.6737587650350747, -4.842901733360249317 ) ) ;
#24393 = ORIENTED_EDGE ( 'NONE', *, *, #30257, .F. ) ;
#24394 = CARTESIAN_POINT ( 'NONE',  ( 10.69584247140445221, 34.84768628210143504, -6.932735513423970097 ) ) ;
#24395 = CARTESIAN_POINT ( 'NONE',  ( -27.00000000000000355, 196.0250000012290457, -15.58845726811989429 ) ) ;
#24396 = DIRECTION ( 'NONE',  ( -0.000000000000000000, -1.000000000000000000, -0.000000000000000000 ) ) ;
#24397 = CARTESIAN_POINT ( 'NONE',  ( 34.40762885551985306, -5.407089921784861808, 167.4314352137346873 ) ) ;
#24398 = CARTESIAN_POINT ( 'NONE',  ( -10.83675517735155047, 105.8601862821014379, -11.08355503943142750 ) ) ;
#24399 =( BOUNDED_CURVE ( )  B_SPLINE_CURVE ( 2, ( #32214, #17830, #36361, #36174, #24626, #1309, #33158 ),
 .UNSPECIFIED., .F., .F. ) 
 B_SPLINE_CURVE_WITH_KNOTS ( ( 3, 2, 2, 3 ),
 ( 0.06521739130434869858, 0.07246376811594300305, 0.07971014492753727976, 0.08695652173913158423 ),
 .UNSPECIFIED. ) 
 CURVE ( )  GEOMETRIC_REPRESENTATION_ITEM ( )  RATIONAL_B_SPLINE_CURVE ( ( 0.9999999999999837907, 0.8660254037844549169, 1.000000000000000000, 0.8660254037844387076, 1.000000000000000000, 0.8660254037844173913, 1.000000000000021316 ) ) 
 REPRESENTATION_ITEM ( '' )  );
#24400 = CARTESIAN_POINT ( 'NONE',  ( -61.48288769728822700, 203.5309553116391896, -1.857196546604028997 ) ) ;
#24401 = CARTESIAN_POINT ( 'NONE',  ( 16.56230152254411436, 7.209453229046475009, -4.753124999385526017 ) ) ;
#24402 = CARTESIAN_POINT ( 'NONE',  ( 1.715153634034233487, 37.72268628210143504, 9.534712964251941258 ) ) ;
#24403 = CARTESIAN_POINT ( 'NONE',  ( 16.56230152254410726, 0.000000000000000000, -10.00000000000000000 ) ) ;
#24404 = CARTESIAN_POINT ( 'NONE',  ( -36.34747103062156981, 214.3500491399821044, -7.303452534266878793 ) ) ;
#24405 = CARTESIAN_POINT ( 'NONE',  ( 15.00000000000000000, 249.6062500012290570, 0.000000000000000000 ) ) ;
#24406 = CARTESIAN_POINT ( 'NONE',  ( -4.622313124798576922, 78.83518628210146062, -11.61527771782819762 ) ) ;
#24407 = CARTESIAN_POINT ( 'NONE',  ( 27.00000000000001066, 199.7375000000000114, 15.58845726811988897 ) ) ;
#24408 = CARTESIAN_POINT ( 'NONE',  ( 24.00000000000000000, 247.5062500012290627, 5.196152422706629359 ) ) ;
#24410 = ORIENTED_EDGE ( 'NONE', *, *, #6809, .T. ) ;
#24409 = CARTESIAN_POINT ( 'NONE',  ( -8.152565276336710909, 48.64768628210144641, 5.233372021372435512 ) ) ;
#24411 = CARTESIAN_POINT ( 'NONE',  ( 20.99999999999999645, 242.0124999999999886, 5.999999999999998224 ) ) ;
#24412 = VERTEX_POINT ( 'NONE', #3980 ) ;
#24413 = CARTESIAN_POINT ( 'NONE',  ( 21.00000000000000000, 6.928203230275506996, -1.012500000000014388 ) ) ;
#24414 = COLOUR_RGB ( '',0.8941176470588234615, 0.8941176470588234615, 0.8941176470588234615 ) ;
#24415 = CARTESIAN_POINT ( 'NONE',  ( 13.56230152254411792, -5.196152422706638241, -6.675000000000069988 ) ) ;
#24416 = CARTESIAN_POINT ( 'NONE',  ( 24.59746635921792901, -3.604726614523244610, 162.7561563650505434 ) ) ;
#24417 = CARTESIAN_POINT ( 'NONE',  ( 36.74950584413092258, 7.347880794884125653E-16, 161.1753960670511674 ) ) ;
#24418 = CARTESIAN_POINT ( 'NONE',  ( 24.00000000000000000, 245.1999999999999886, 5.196152422706629359 ) ) ;
#24419 = VECTOR ( 'NONE', #12644, 1000.000000000000000 ) ;
#24420 = CARTESIAN_POINT ( 'NONE',  ( -27.24356964374999279, 196.2406250006145285, 15.72908226750539384 ) ) ;
#24421 = CARTESIAN_POINT ( 'NONE',  ( -8.715434833792127023, 78.93981371789855928, 8.962234695871568846 ) ) ;
#24422 = CARTESIAN_POINT ( 'NONE',  ( 10.69584247140445221, 108.4476862821014578, -6.932735513423970097 ) ) ;
#24423 = EDGE_LOOP ( 'NONE', ( #14249, #4944, #15567, #10051 ) ) ;
#24424 = ORIENTED_EDGE ( 'NONE', *, *, #8780, .F. ) ;
#24425 = CARTESIAN_POINT ( 'NONE',  ( 27.00000000000000355, 197.6375000012290286, -3.306546357697854128E-15 ) ) ;
#24426 = CARTESIAN_POINT ( 'NONE',  ( 21.00000000000000000, 240.4093750006145171, 6.646953231504538984 ) ) ;
#24427 = CARTESIAN_POINT ( 'NONE',  ( 5.770363421894130873, 82.96481371789856496, -14.38691631536193860 ) ) ;
#24428 = CARTESIAN_POINT ( 'NONE',  ( 23.87821517812499650, 4.985214923628404904, -6.703124999385495997 ) ) ;
#24429 = CARTESIAN_POINT ( 'NONE',  ( 18.12178482187500350, 245.4343750006145228, 4.985214923628407568 ) ) ;
#24430 = CARTESIAN_POINT ( 'NONE',  ( -3.474262827703337830, 97.23518628210146630, -8.843639120294326972 ) ) ;
#24431 = CARTESIAN_POINT ( 'NONE',  ( 27.00000000000015632, -3.464101615137659351, -6.506249998770940124 ) ) ;
#24432 = CARTESIAN_POINT ( 'NONE',  ( -1.715153634034442431, 50.47731371789854649, 9.534712964251900402 ) ) ;
#24433 = CARTESIAN_POINT ( 'NONE',  ( 22.80587116629410716, 3.604726614523238837, -6.628124999385534899 ) ) ;
#24434 = EDGE_CURVE ( 'NONE', #19674, #22517, #21065, .T. ) ;
#24435 = CARTESIAN_POINT ( 'NONE',  ( -2.064181346179062349, 109.7023137178985479, -9.465287035748106703 ) ) ;
#24436 = CARTESIAN_POINT ( 'NONE',  ( 23.87821517812499650, 240.5968750006145171, -4.985214923628404904 ) ) ;
#24437 = CARTESIAN_POINT ( 'NONE',  ( -11.61527771782809282, 34.66481371789854649, -4.622313124798832717 ) ) ;
#24438 = CARTESIAN_POINT ( 'NONE',  ( 11.61527771782819940, 81.13518628210145778, -4.622313124798573369 ) ) ;
#24439 = CARTESIAN_POINT ( 'NONE',  ( 22.56230152254412147, -3.464101615137751278, -8.249999998771009757 ) ) ;
#24440 = VECTOR ( 'NONE', #28499, 1000.000000000000000 ) ;
#24441 = DIRECTION ( 'NONE',  ( -1.000000000000000000, 0.000000000000000000, 0.000000000000000000 ) ) ;
#24442 = CARTESIAN_POINT ( 'NONE',  ( 34.17721086063072988, -5.407089921784855591, 164.7977454806546120 ) ) ;
#24443 = CARTESIAN_POINT ( 'NONE',  ( 19.68408634441911786, -5.407089921784861808, -4.096874999385518912 ) ) ;
#24444 =( LENGTH_UNIT ( ) NAMED_UNIT ( * ) SI_UNIT ( .MILLI., .METRE. ) );
#24445 = DIRECTION ( 'NONE',  ( 1.045431693899523378E-14, 0.1163425707149433469, -0.9932091452657081376 ) ) ;
#24446 = CARTESIAN_POINT ( 'NONE',  ( 19.39230484541326760, 244.2424038105676516, 5.999999999999999112 ) ) ;
#24447 = CARTESIAN_POINT ( 'NONE',  ( 3.796722387233379514, 89.18518628210145494, -8.710071997420127943 ) ) ;
#24448 = CARTESIAN_POINT ( 'NONE',  ( 11.48171059495397728, 137.4851862821014663, 4.944772684328674117 ) ) ;
#24449 = FACE_OUTER_BOUND ( 'NONE', #4293, .T. ) ;
#24450 = CARTESIAN_POINT ( 'NONE',  ( 23.87821517812499650, 240.5968750006145171, -4.985214923628404904 ) ) ;
#24451 = ORIENTED_EDGE ( 'NONE', *, *, #2440, .T. ) ;
#24452 = CARTESIAN_POINT ( 'NONE',  ( 34.26872439051576436, 5.407089921784857367, 165.8437499136509814 ) ) ;
#24453 = CARTESIAN_POINT ( 'NONE',  ( 15.24356964374999990, 0.000000000000000000, -3.740624999385461003 ) ) ;
#24454 = EDGE_CURVE ( 'NONE', #37366, #4785, #18218, .T. ) ;
#24455 = CARTESIAN_POINT ( 'NONE',  ( 26.99999999999999645, 242.5374999999999943, 3.464101615137751278 ) ) ;
#24456 = CARTESIAN_POINT ( 'NONE',  ( 19.97221621173429540, 239.9536485273282835, -5.828891293067281154 ) ) ;
#24457 = CARTESIAN_POINT ( 'NONE',  ( 0.000000000000000000, 148.0000000000000000, 0.000000000000000000 ) ) ;
#24458 = CARTESIAN_POINT ( 'NONE',  ( 23.99999999999999645, 5.196152422706631135, -3.243749998770945275 ) ) ;
#24459 = CARTESIAN_POINT ( 'NONE',  ( 21.00000000000000000, 241.8718750006145228, 6.646953231504538984 ) ) ;
#24460 = CARTESIAN_POINT ( 'NONE',  ( 22.80587116629410716, 3.604726614523238837, -1.678124999385518068 ) ) ;
#24461 = CARTESIAN_POINT ( 'NONE',  ( -8.152565276336593669, 25.75231371789854506, -5.233372021372610483 ) ) ;
#24462 = CARTESIAN_POINT ( 'NONE',  ( 5.778771075727756162E-15, 198.1718750006145342, 31.45816453501076637 ) ) ;
#24464 = EDGE_LOOP ( 'NONE', ( #11267, #7231, #12923, #3047 ) ) ;
#24463 = ORIENTED_EDGE ( 'NONE', *, *, #27701, .T. ) ;
#24465 = AXIS2_PLACEMENT_3D ( 'NONE', #17260, #28801, #11190 ) ;
#24466 =( GEOMETRIC_REPRESENTATION_CONTEXT ( 3 ) GLOBAL_UNCERTAINTY_ASSIGNED_CONTEXT ( ( #29713 ) ) GLOBAL_UNIT_ASSIGNED_CONTEXT ( ( #36211, #1721, #36586 ) ) REPRESENTATION_CONTEXT ( 'NONE', 'WORKASPACE' ) );
#24467 = CARTESIAN_POINT ( 'NONE',  ( 26.75643035624999655, 247.2718750006145001, -7.049594010296217766E-16 ) ) ;
#24468 = CARTESIAN_POINT ( 'NONE',  ( -12.50000000000000355, 24.88981371789854435, 0.1745138560722786503 ) ) ;
#24469 = CARTESIAN_POINT ( 'NONE',  ( 23.87821517812499650, 4.985214923628404904, -1.640624999385470462 ) ) ;
#24470 = CARTESIAN_POINT ( 'NONE',  ( -14.25334919248795096, 125.5148137178985763, 6.092822981423662299 ) ) ;
#24471 = AXIS2_PLACEMENT_3D ( 'NONE', #30545, #27871, #1903 ) ;
#24472 = CARTESIAN_POINT ( 'NONE',  ( 23.87821517812500005, -4.985214923628404016, -0.5531249993854792102 ) ) ;
#24473 = ORIENTED_EDGE ( 'NONE', *, *, #22391, .T. ) ;
#24474 = CARTESIAN_POINT ( 'NONE',  ( 10.31873187879410736, -3.604726614523244610, -6.009374999385536320 ) ) ;
#24475 = EDGE_LOOP ( 'NONE', ( #25631, #16134, #12481, #29245 ) ) ;
#24476 = CARTESIAN_POINT ( 'NONE',  ( 27.24356964375000345, 196.4281250006145569, -3.336375036156643733E-15 ) ) ;
#24477 = CARTESIAN_POINT ( 'NONE',  ( 6.932735513423970097, 129.1476862821014890, 10.69584247140445044 ) ) ;
#24478 = CARTESIAN_POINT ( 'NONE',  ( 37.16782192588006239, -3.604726614523238837, 163.1621225127927062 ) ) ;
#24479 = CARTESIAN_POINT ( 'NONE',  ( -50.78794563604517975, 203.8621396198271043, 6.307003348498029460 ) ) ;
#24480 = CARTESIAN_POINT ( 'NONE',  ( 23.87821517812499650, 247.7968750006145058, -4.985214923628404904 ) ) ;
#24481 = PRESENTATION_STYLE_ASSIGNMENT (( #27692 ) ) ;
#24482 = CARTESIAN_POINT ( 'NONE',  ( 15.02283181144952628, 7.347880794884122694E-16, 50.52293445648592751 ) ) ;
#24483 = CARTESIAN_POINT ( 'NONE',  ( -49.60044563604517265, 206.6211998817775566, -3.209657149897419348 ) ) ;
#24484 = CARTESIAN_POINT ( 'NONE',  ( -12.46528703574805697, 132.5976862821014777, -2.660918448318280838 ) ) ;
#24485 = CARTESIAN_POINT ( 'NONE',  ( 37.33287311370841621, 7.646167579472015790E-16, 165.0486662223039218 ) ) ;
#24486 = ORIENTED_EDGE ( 'NONE', *, *, #29019, .F. ) ;
#24487 = CARTESIAN_POINT ( 'NONE',  ( -27.00000000000000355, 195.1250000012290400, -15.58845726811989429 ) ) ;
#24488 = CARTESIAN_POINT ( 'NONE',  ( 6.092822981423978490, 135.1851862821014549, -14.25334919248782306 ) ) ;
#24489 = VECTOR ( 'NONE', #25330, 1000.000000000000000 ) ;
#24490 = CARTESIAN_POINT ( 'NONE',  ( -52.37872103062156981, 201.4690446883607819, 2.162041339862843525 ) ) ;
#24491 = CARTESIAN_POINT ( 'NONE',  ( 3.796722387233379514, 116.7851862821014635, -8.710071997420127943 ) ) ;
#24492 = DIRECTION ( 'NONE',  ( 0.000000000000000000, 0.000000000000000000, 1.000000000000000000 ) ) ;
#24493 = CARTESIAN_POINT ( 'NONE',  ( 11.48171059495397728, 8.685186282101437172, 4.944772684328674117 ) ) ;
#24494 = CARTESIAN_POINT ( 'NONE',  ( 19.56230152254412147, 5.196152422706637353, -6.900000000000044764 ) ) ;
#24495 = UNCERTAINTY_MEASURE_WITH_UNIT (LENGTH_MEASURE( 1.000000000000000082E-05 ), #13895, 'distance_accuracy_value', 'NONE');
#24496 = ORIENTED_EDGE ( 'NONE', *, *, #22827, .T. ) ;
#24497 = CARTESIAN_POINT ( 'NONE',  ( 7.234628195640337545, 197.7299038117967029, -26.99999999999999289 ) ) ;
#24498 = CARTESIAN_POINT ( 'NONE',  ( -13.23911966647218463, 113.0476862821014663, 8.632099005475506459 ) ) ;
#24499 = LINE ( 'NONE', #7072, #623 ) ;
#24500 = CARTESIAN_POINT ( 'NONE',  ( 8.843639120294245259, 140.4648137178985507, 3.474262827703527901 ) ) ;
#24501 = CARTESIAN_POINT ( 'NONE',  ( 27.24356964375000700, 199.5406250006145683, 15.72908226750537075 ) ) ;
#24502 = CARTESIAN_POINT ( 'NONE',  ( 5.778771075727756162E-15, 199.0718750006145399, 31.45816453501075927 ) ) ;
#24503 = LINE ( 'NONE', #32645, #10167 ) ;
#24504 = CARTESIAN_POINT ( 'NONE',  ( 2.999999999999997335, 252.0000000000000000, -2.500000000000000000 ) ) ;
#24505 = CARTESIAN_POINT ( 'NONE',  ( 0.1745138560723095977, 68.58981371789855075, 9.500000000000005329 ) ) ;
#24506 = VERTEX_POINT ( 'NONE', #14803 ) ;
#24507 = CARTESIAN_POINT ( 'NONE',  ( 15.00000000000000178, 243.7937500012290570, 3.464101615137757051 ) ) ;
#24508 = CARTESIAN_POINT ( 'NONE',  ( 8.962234695871567070, 85.83981371789856496, 8.715434833792127023 ) ) ;
#24509 = CARTESIAN_POINT ( 'NONE',  ( 22.80587116629411781, 7.646167579472024665E-16, -4.921874999385511984 ) ) ;
#24510 = CARTESIAN_POINT ( 'NONE',  ( -7.145391844330089448, 143.0000000000000284, 10.79229366378071298 ) ) ;
#24511 = CARTESIAN_POINT ( 'NONE',  ( 21.00000000000000000, 6.646953231504538984, -3.965624999385493510 ) ) ;
#24512 = CARTESIAN_POINT ( 'NONE',  ( -2.311890736173448424, 50.47731371789855359, 12.53471296425189330 ) ) ;
#24513 = ORIENTED_EDGE ( 'NONE', *, *, #26495, .F. ) ;
#24514 = CARTESIAN_POINT ( 'NONE',  ( 20.99999999999999645, -6.646953231504538984, -6.328124999385495109 ) ) ;
#24515 = CARTESIAN_POINT ( 'NONE',  ( 23.87821517812500005, 244.0468750006145058, 4.985214923628404016 ) ) ;
#24516 = CARTESIAN_POINT ( 'NONE',  ( 4.622313124798573369, 19.03518628210144925, 11.61527771782819940 ) ) ;
#24517 = CARTESIAN_POINT ( 'NONE',  ( -42.27752896937850124, 213.3500491399821613, 5.571401726697954970 ) ) ;
#24518 = CARTESIAN_POINT ( 'NONE',  ( -58.50669563604516554, 209.8844732041982013, -6.500000000000000888 ) ) ;
#24519 = CARTESIAN_POINT ( 'NONE',  ( 24.58926402489574770, 0.000000000000000000, 159.8677550070055702 ) ) ;
#24520 = CARTESIAN_POINT ( 'NONE',  ( 4.944772684328420986, 77.21481371789855075, 11.48171059495408208 ) ) ;
#24521 = ADVANCED_FACE ( 'NONE', ( #35250, #17844 ), #6266, .F. ) ;
#24522 = CARTESIAN_POINT ( 'NONE',  ( -46.44122103062156981, 208.9097554298617752, -4.530955311639240257 ) ) ;
#24524 = EDGE_CURVE ( 'NONE', #7551, #31196, #24084, .T. ) ;
#24523 = CARTESIAN_POINT ( 'NONE',  ( -59.70163769728823411, 215.6869285224996986, -3.149950860017881382 ) ) ;
#24525 = CARTESIAN_POINT ( 'NONE',  ( 0.000000000000000000, 2.000000000000000000, -25.00000000000000000 ) ) ;
#24526 = CARTESIAN_POINT ( 'NONE',  ( 14.25334919248795451, 56.51481371789856212, -6.092822981423661410 ) ) ;
#24527 = CARTESIAN_POINT ( 'NONE',  ( -43.46502896937849414, 217.3034525342667962, -4.350049139982195001 ) ) ;
#24528 = LINE ( 'NONE', #30777, #18374 ) ;
#24529 = CARTESIAN_POINT ( 'NONE',  ( -11.61527771782819940, 76.53518628210146346, 4.622313124798574258 ) ) ;
#24530 = CARTESIAN_POINT ( 'NONE',  ( 0.1745138560725837118, 24.21018628210144996, -15.50000000000000533 ) ) ;
#24532 = EDGE_CURVE ( 'NONE', #10609, #25022, #23519, .T. ) ;
#24531 = CARTESIAN_POINT ( 'NONE',  ( 10.56230152254410726, 3.464101615137757051, -0.4875000000000247469 ) ) ;
#24533 = CARTESIAN_POINT ( 'NONE',  ( -28.51642293503100944, 203.9737468885152794, -5.287141534248642749 ) ) ;
#24534 = VERTEX_POINT ( 'NONE', #20681 ) ;
#24535 = CARTESIAN_POINT ( 'NONE',  ( -6.092822981423970496, 56.98518628210145209, 14.25334919248782661 ) ) ;
#24536 = CARTESIAN_POINT ( 'NONE',  ( 13.62178482187501416, 196.8031250006145285, 23.59362340125806767 ) ) ;
#24537 = LINE ( 'NONE', #12601, #18064 ) ;
#24538 = CARTESIAN_POINT ( 'NONE',  ( -42.68080436395489841, 203.5000000000000000, -0.1155267958017335561 ) ) ;
#24539 = DIRECTION ( 'NONE',  ( 0.000000000000000000, 1.000000000000000000, 0.000000000000000000 ) ) ;
#24540 = CARTESIAN_POINT ( 'NONE',  ( -8.962234695871760692, 20.76018628210144001, 8.715434833791933400 ) ) ;
#24541 = VECTOR ( 'NONE', #35629, 1000.000000000000000 ) ;
#24542 = DIRECTION ( 'NONE',  ( -1.000000000000000000, -6.123233995736766036E-17, 0.000000000000000000 ) ) ;
#24543 = CARTESIAN_POINT ( 'NONE',  ( 6.594114490232462877, 129.5398137178985678, -6.840914352311949109 ) ) ;
#24544 = CARTESIAN_POINT ( 'NONE',  ( 15.24356964374999990, 244.4593750006145569, 0.000000000000000000 ) ) ;
#24545 = ORIENTED_EDGE ( 'NONE', *, *, #29347, .T. ) ;
#24546 = CARTESIAN_POINT ( 'NONE',  ( 21.00000000000000000, 245.2187500012290116, 5.999999999999998224 ) ) ;
#24547 = CARTESIAN_POINT ( 'NONE',  ( -8.962234695871565293, 127.2398137178985564, -8.715434833792128799 ) ) ;
#24548 = CARTESIAN_POINT ( 'NONE',  ( 13.44051670066911086, 5.407089921784856479, -6.515624999385543958 ) ) ;
#24549 = CARTESIAN_POINT ( 'NONE',  ( 37.25116460488249004, -3.604726614523235284, 164.1147336928429468 ) ) ;
#24550 =( BOUNDED_CURVE ( )  B_SPLINE_CURVE ( 2, ( #18993, #5122, #31101, #22573, #33937, #25028, #4755 ),
 .UNSPECIFIED., .F., .F. ) 
 B_SPLINE_CURVE_WITH_KNOTS ( ( 3, 2, 2, 3 ),
 ( 0.6739130434782617529, 0.6811594202898560990, 0.6884057971014503341, 0.6956521739130446802 ),
 .UNSPECIFIED. ) 
 CURVE ( )  GEOMETRIC_REPRESENTATION_ITEM ( )  RATIONAL_B_SPLINE_CURVE ( ( 0.9999999999999835687, 0.8660254037844551389, 1.000000000000000000, 0.8660254037844387076, 1.000000000000000000, 0.8660254037844161701, 1.000000000000022649 ) ) 
 REPRESENTATION_ITEM ( '' )  );
#24551 = CARTESIAN_POINT ( 'NONE',  ( 37.37702719191401002, 7.347880794884125653E-16, 168.3479978933117422 ) ) ;
#24552 = CARTESIAN_POINT ( 'NONE',  ( -1.909035429704832693E-15, 197.6375000000000171, -31.17691453623979214 ) ) ;
#24553 = ORIENTED_EDGE ( 'NONE', *, *, #18725, .F. ) ;
#24554 = CARTESIAN_POINT ( 'NONE',  ( 12.46528703574805874, 35.99768628210144072, 2.660918448318279950 ) ) ;
#24555 = ORIENTED_EDGE ( 'NONE', *, *, #36792, .T. ) ;
#24556 = EDGE_LOOP ( 'NONE', ( #20542, #15266, #30008, #8784 ) ) ;
#24557 = CARTESIAN_POINT ( 'NONE',  ( 15.00000000000000000, 0.000000000000000000, -4.893749998770957177 ) ) ;
#24558 = DIRECTION ( 'NONE',  ( -1.000000000000000000, -6.123233995736766036E-17, 0.000000000000000000 ) ) ;
#24559 = CARTESIAN_POINT ( 'NONE',  ( 14.99999999999999289, 204.0000000000000000, 0.000000000000000000 ) ) ;
#24560 = CARTESIAN_POINT ( 'NONE',  ( 20.99999999999999645, 0.000000000000000000, -8.000000000000000000 ) ) ;
#24561 = CARTESIAN_POINT ( 'NONE',  ( 26.75643035624999655, 3.323476615752271712, -8.878124999385482496 ) ) ;
#24562 = CARTESIAN_POINT ( 'NONE',  ( -8.962234695871760692, 85.16018628210144925, 8.715434833791933400 ) ) ;
#24563 = CARTESIAN_POINT ( 'NONE',  ( -15.46528703574804986, 132.5976862821014493, -3.257655550457287497 ) ) ;
#24564 = CARTESIAN_POINT ( 'NONE',  ( 20.99999999999999645, 210.0000000000000000, 5.999999999999996447 ) ) ;
#24565 = CARTESIAN_POINT ( 'NONE',  ( -49.99627896937850835, 205.4690446883607535, -1.090244570138286351 ) ) ;
#24566 = CARTESIAN_POINT ( 'NONE',  ( 34.23483110115314787, -5.196152422706629359, 166.8536719673923017 ) ) ;
#24567 = CARTESIAN_POINT ( 'NONE',  ( 1.715153634034445762, 9.077313717898549683, -9.534712964251895073 ) ) ;
#24568 = CARTESIAN_POINT ( 'NONE',  ( -48.22247103062156270, 206.6499508600178672, 5.571401726697986057 ) ) ;
#24570 = ADVANCED_FACE ( 'NONE', ( #32978 ), #9676, .F. ) ;
#24569 = CARTESIAN_POINT ( 'NONE',  ( -61.48288769728824121, 201.5309553116392181, -2.393094931466246855 ) ) ;
#24571 = AXIS2_PLACEMENT_3D ( 'NONE', #3149, #26266, #32332 ) ;
#24572 =( BOUNDED_CURVE ( )  B_SPLINE_CURVE ( 2, ( #26006, #11421, #20146, #22988, #34538, #14083, #8577 ),
 .UNSPECIFIED., .F., .F. ) 
 B_SPLINE_CURVE_WITH_KNOTS ( ( 3, 2, 2, 3 ),
 ( 0.6739130434782618639, 0.6811594202898562100, 0.6884057971014503341, 0.6956521739130446802 ),
 .UNSPECIFIED. ) 
 CURVE ( )  GEOMETRIC_REPRESENTATION_ITEM ( )  RATIONAL_B_SPLINE_CURVE ( ( 0.9999999999999815703, 0.8660254037844571373, 1.000000000000000000, 0.8660254037844387076, 1.000000000000000000, 0.8660254037844161701, 1.000000000000022649 ) ) 
 REPRESENTATION_ITEM ( '' )  );
#24573 = CARTESIAN_POINT ( 'NONE',  ( 36.74950584413092258, 7.347880794884125653E-16, 161.1753960670511674 ) ) ;
#24574 = CARTESIAN_POINT ( 'NONE',  ( -27.24356964375000345, 198.9031250006145228, 0.000000000000000000 ) ) ;
#24575 = CARTESIAN_POINT ( 'NONE',  ( 15.46528703574811736, 121.2023137178985479, -3.257655550456947768 ) ) ;
#24576 = CARTESIAN_POINT ( 'NONE',  ( -50.78794563604515133, 205.3262412349647832, 4.842901733360250205 ) ) ;
#24577 = ORIENTED_EDGE ( 'NONE', *, *, #19662, .F. ) ;
#24578 = CARTESIAN_POINT ( 'NONE',  ( 24.74614436184151955, 0.000000000000000000, 161.6609054635707423 ) ) ;
#24579 = CARTESIAN_POINT ( 'NONE',  ( 0.1745138560725515708, 134.6101862821014663, -12.50000000000000355 ) ) ;
#24580 = LINE ( 'NONE', #9616, #26541 ) ;
#24581 = CARTESIAN_POINT ( 'NONE',  ( 24.82625018393050809, 3.604726614523240613, 165.3711674475413531 ) ) ;
#24582 = CARTESIAN_POINT ( 'NONE',  ( 15.53471296425195369, 99.82268628210142936, -2.908627838312120684 ) ) ;
#24583 = CARTESIAN_POINT ( 'NONE',  ( -60.88913769728823411, 206.8500491399821044, -5.686928522499717253 ) ) ;
#24584 = CARTESIAN_POINT ( 'NONE',  ( 19.68408634441910721, 5.407089921784857367, -3.890624999385555505 ) ) ;
#24585 = CARTESIAN_POINT ( 'NONE',  ( -3.474262827703337830, 42.03518628210144925, -8.843639120294326972 ) ) ;
#24586 = CARTESIAN_POINT ( 'NONE',  ( 0.000000000000000000, 0.000000000000000000, 7.500000000000000000 ) ) ;
#24587 = CARTESIAN_POINT ( 'NONE',  ( -38.32663769728823411, 202.5810206699313767, 4.149950860017909804 ) ) ;
#24588 = CARTESIAN_POINT ( 'NONE',  ( 36.70701741954223252, -3.464101615137295642, 160.6897511517313717 ) ) ;
#24589 = CARTESIAN_POINT ( 'NONE',  ( 6.932735513423970097, 83.14768628210144641, 10.69584247140445044 ) ) ;
#24590 = CARTESIAN_POINT ( 'NONE',  ( 27.00000000000000355, 199.3249999999999886, -3.306546357697854128E-15 ) ) ;
#24591 = DIRECTION ( 'NONE',  ( -0.000000000000000000, 1.000000000000000000, -0.000000000000000000 ) ) ;
#24593 = CARTESIAN_POINT ( 'NONE',  ( 22.56230152254277499, 3.464101615138533763, -1.987500000000047118 ) ) ;
#24592 = CARTESIAN_POINT ( 'NONE',  ( 6.840914352312096547, 43.76018628210144357, -6.594114490232313663 ) ) ;
#24594 = CARTESIAN_POINT ( 'NONE',  ( 21.00000000000000000, 242.0124999999999886, 5.999999999999998224 ) ) ;
#24595 = ORIENTED_EDGE ( 'NONE', *, *, #10646, .T. ) ;
#24596 = CARTESIAN_POINT ( 'NONE',  ( 21.00000000000000000, 6.928203230275506996, -2.362500000000001155 ) ) ;
#24597 = CARTESIAN_POINT ( 'NONE',  ( -66.62872103062152007, 203.4690446883607535, 1.626142955000567936 ) ) ;
#24598 = CARTESIAN_POINT ( 'NONE',  ( 30.96108431102187808, 7.209453229046482114, 163.8557146672041824 ) ) ;
#24599 = CARTESIAN_POINT ( 'NONE',  ( 30.82136276087599214, 6.928203230275514990, 162.2586900412136686 ) ) ;
#24600 = CARTESIAN_POINT ( 'NONE',  ( 15.00000000000000000, 246.3625000000000114, -3.464101615137752166 ) ) ;
#24601 = DIRECTION ( 'NONE',  ( 0.8083506638593001004, 0.5887012860850814322, -0.000000000000000000 ) ) ;
#24602=STYLED_ITEM('',(#37542),#21172);
#24603 = CARTESIAN_POINT ( 'NONE',  ( 2.660918448318002838, 77.50231371789855928, 12.46528703574811558 ) ) ;
#24604 = CARTESIAN_POINT ( 'NONE',  ( -0.1745138560725500443, 84.01018628210145778, 12.50000000000000355 ) ) ;
#24605 = ORIENTED_EDGE ( 'NONE', *, *, #23303, .T. ) ;
#24606 = ORIENTED_EDGE ( 'NONE', *, *, #31239, .T. ) ;
#24607 = CARTESIAN_POINT ( 'NONE',  ( 13.50000000000001421, 198.4625000012290172, 23.38268590217984055 ) ) ;
#24608 = DIRECTION ( 'NONE',  ( -0.8083506638593009885, -0.5887012860850802110, 0.000000000000000000 ) ) ;
#24609 = CARTESIAN_POINT ( 'NONE',  ( -14.25334919248795096, 61.11481371789854933, 6.092822981423662299 ) ) ;
#24610 = CARTESIAN_POINT ( 'NONE',  ( 26.75643035624999655, 3.323476615752271712, -7.190624999385489602 ) ) ;
#24611 = CARTESIAN_POINT ( 'NONE',  ( 21.00000000000000000, 245.6968750006145399, -6.646953231504538984 ) ) ;
#24612 = CARTESIAN_POINT ( 'NONE',  ( -57.32663769728824121, 206.0451222850691408, 2.149950860017832532 ) ) ;
#24613 =( BOUNDED_CURVE ( )  B_SPLINE_CURVE ( 2, ( #22075, #18684, #10873, #19245, #7293, #33627, #4437, #16574, #7477 ),
 .UNSPECIFIED., .F., .F. ) 
 B_SPLINE_CURVE_WITH_KNOTS ( ( 3, 2, 2, 2, 3 ),
 ( 0.2282608695652173780, 0.2318840579710144956, 0.2391304347826087029, 0.2463768115942029102, 0.2500000000000000000 ),
 .UNSPECIFIED. ) 
 CURVE ( )  GEOMETRIC_REPRESENTATION_ITEM ( )  RATIONAL_B_SPLINE_CURVE ( ( 0.9330127018922194093, 0.9330127018922190762, 1.000000000000000000, 0.8660254037844387076, 1.000000000000000000, 0.8660254037844387076, 1.000000000000000000, 0.9330127018922196314, 0.9330127018922194093 ) ) 
 REPRESENTATION_ITEM ( '' )  );
#24614 = AXIS2_PLACEMENT_3D ( 'NONE', #11006, #8174, #14596 ) ;
#24615 = PLANE ( 'NONE',  #23413 ) ;
#24616 = CARTESIAN_POINT ( 'NONE',  ( -9.465287035748106703, 61.40231371789855785, 2.064181346179061460 ) ) ;
#24617 = CARTESIAN_POINT ( 'NONE',  ( 22.80587116629410360, 7.646167579472015790E-16, -6.665624999385527438 ) ) ;
#24618 = CARTESIAN_POINT ( 'NONE',  ( -1.715153634034442431, 105.6773137178985706, 9.534712964251900402 ) ) ;
#24619 = CARTESIAN_POINT ( 'NONE',  ( 20.00041244883536606, 239.7473985345926053, -5.668978318349186196 ) ) ;
#24620 = CARTESIAN_POINT ( 'NONE',  ( -10.69584247140429412, 25.75231371789854506, -6.932735513424201024 ) ) ;
#24621 = CARTESIAN_POINT ( 'NONE',  ( 12.53471296425194836, 81.42268628210145209, -2.311890736173178418 ) ) ;
#24622 = CARTESIAN_POINT ( 'NONE',  ( 13.56230152254410548, 5.196152422706630247, -8.962499998770995902 ) ) ;
#24623 = CARTESIAN_POINT ( 'NONE',  ( 1.120210788295102201E-13, 195.0500000012290513, -27.00000000000000711 ) ) ;
#24624 = CARTESIAN_POINT ( 'NONE',  ( 24.52392870127459545, -3.604726614523240613, 161.9156170885356403 ) ) ;
#24625 = CARTESIAN_POINT ( 'NONE',  ( 22.80587116629411426, 7.646167579472024665E-16, -6.271874999385529392 ) ) ;
#24626 = CARTESIAN_POINT ( 'NONE',  ( 18.00000000000000355, -5.196152422706632912, -0.8249999999999924061 ) ) ;
#24627 = FACE_OUTER_BOUND ( 'NONE', #10259, .T. ) ;
#24628 = CARTESIAN_POINT ( 'NONE',  ( 29.49486714975617474, 6.148716665048037378, 159.5363409456820136 ) ) ;
#24629 = CARTESIAN_POINT ( 'NONE',  ( -1.715153634034234598, 88.32268628210142936, -9.534712964251941258 ) ) ;
#24630 = CARTESIAN_POINT ( 'NONE',  ( 27.00000000000000355, 198.9875000012290229, -3.306546357697854128E-15 ) ) ;
#24631 = CARTESIAN_POINT ( 'NONE',  ( -4.622313124798576922, 134.0351862821014493, -11.61527771782819762 ) ) ;
#24632 = CARTESIAN_POINT ( 'NONE',  ( 15.24356964374999990, 240.2593750006145115, -3.323476615752268604 ) ) ;
#24633 = VERTEX_POINT ( 'NONE', #29572 ) ;
#24634 = CARTESIAN_POINT ( 'NONE',  ( 27.95086320365434318, -5.407089921784859143, 165.2671938279954702 ) ) ;
#24635 = CARTESIAN_POINT ( 'NONE',  ( 15.24356964374999990, 0.000000000000000000, -5.090624999385479299 ) ) ;
#24636 = CARTESIAN_POINT ( 'NONE',  ( -13.62178482187498396, 198.1343750006145399, 23.59362340125808188 ) ) ;
#24637 = CARTESIAN_POINT ( 'NONE',  ( 25.44230085693126497, 0.000000000000000000, 169.6180106133541869 ) ) ;
#24638 = CARTESIAN_POINT ( 'NONE',  ( 15.00000000000000000, 239.7062500012290513, 0.000000000000000000 ) ) ;
#24639 = CARTESIAN_POINT ( 'NONE',  ( 15.24356964374999990, 243.5218750006145569, -3.323476615752268604 ) ) ;
#24640 = ADVANCED_FACE ( 'NONE', ( #384, #26536 ), #21438, .T. ) ;
#24641 = CARTESIAN_POINT ( 'NONE',  ( -6.932735513424201912, 143.0523137178985564, 10.69584247140429412 ) ) ;
#24642 = CARTESIAN_POINT ( 'NONE',  ( -1.926257025242585782E-15, 197.4968750006145513, -31.45816453501076637 ) ) ;
#24644 = ORIENTED_EDGE ( 'NONE', *, *, #30986, .F. ) ;
#24643 = VERTEX_POINT ( 'NONE', #3229 ) ;
#24645 = CARTESIAN_POINT ( 'NONE',  ( 21.00000000000000000, 244.6843750006144944, -6.646953231504538984 ) ) ;
#24646 = CARTESIAN_POINT ( 'NONE',  ( 11.61527771782809637, 30.06481371789855572, 4.622313124798827388 ) ) ;
#24647 = CARTESIAN_POINT ( 'NONE',  ( 15.24356964374999990, 3.323476615752268604, -3.778124999385444660 ) ) ;
#24648 = CARTESIAN_POINT ( 'NONE',  ( -14.38691631536193860, 108.2648137178985621, -5.770363421894132649 ) ) ;
#24649 = CARTESIAN_POINT ( 'NONE',  ( 18.00000000000000355, -5.196152422706632912, -8.868749998770963927 ) ) ;
#24650 = VERTEX_POINT ( 'NONE', #26722 ) ;
#24651 = CARTESIAN_POINT ( 'NONE',  ( 10.31873187879410736, -3.604726614523244610, -5.559374999385508609 ) ) ;
#24652 = ORIENTED_EDGE ( 'NONE', *, *, #1028, .F. ) ;
#24653 = CARTESIAN_POINT ( 'NONE',  ( 27.24356964375000700, 196.8406250006145513, 15.72908226750537075 ) ) ;
#24654 = CARTESIAN_POINT ( 'NONE',  ( 10.69584247140445221, 136.0476862821014379, -6.932735513423970097 ) ) ;
#24655 = CARTESIAN_POINT ( 'NONE',  ( 10.31873187879410914, 0.000000000000000000, -1.490624999385542493 ) ) ;
#24656 = CARTESIAN_POINT ( 'NONE',  ( 24.55824627498148160, -3.604726614523244610, 162.3078687509092788 ) ) ;
#24657 = ADVANCED_FACE ( 'NONE', ( #566 ), #14986, .F. ) ;
#24658 = CARTESIAN_POINT ( 'NONE',  ( -51.57961230271184405, 212.3930949314663792, 8.469044688360751749 ) ) ;
#24659 = CARTESIAN_POINT ( 'NONE',  ( 15.24356964374999990, 247.9093750006145171, -3.323476615752268604 ) ) ;
#24660 = CARTESIAN_POINT ( 'NONE',  ( 1.255007937094097924E-14, 199.1000000012290627, -27.00000000000000000 ) ) ;
#24661 = CARTESIAN_POINT ( 'NONE',  ( -42.87127896937849414, 214.5309553116392749, 1.090244570138288127 ) ) ;
#24662 = CARTESIAN_POINT ( 'NONE',  ( -7.228626920339069173, 140.0726862821014720, 10.49813415415989581 ) ) ;
#24663 = CARTESIAN_POINT ( 'NONE',  ( 10.56230152254410903, -3.464101615137757051, -2.099999998770993415 ) ) ;
#24665 = VERTEX_POINT ( 'NONE', #15366 ) ;
#24664 = EDGE_CURVE ( 'NONE', #28768, #17657, #6643, .T. ) ;
#24666 = DIRECTION ( 'NONE',  ( 0.000000000000000000, 0.000000000000000000, -1.000000000000000000 ) ) ;
#24667 = CARTESIAN_POINT ( 'NONE',  ( 15.53471296425195369, 127.4226862821014521, -2.908627838312120684 ) ) ;
#24668 = CARTESIAN_POINT ( 'NONE',  ( -51.58705436395489841, 203.8621396198270475, -6.307003348497942419 ) ) ;
#24669 = CARTESIAN_POINT ( 'NONE',  ( -2.064181346179269738, 111.8976862821014606, 9.465287035748067623 ) ) ;
#24670 = FACE_OUTER_BOUND ( 'NONE', #7223, .T. ) ;
#24671 = CARTESIAN_POINT ( 'NONE',  ( -6.932735513423968321, 14.14768628210144463, -10.69584247140445221 ) ) ;
#24672 = CARTESIAN_POINT ( 'NONE',  ( 10.56230152254410903, -3.464101615137761048, -8.512500000000050804 ) ) ;
#24673 = ORIENTED_EDGE ( 'NONE', *, *, #7888, .T. ) ;
#24674 = CARTESIAN_POINT ( 'NONE',  ( 22.56230152254411792, 7.347880794884125653E-16, -7.875000000000048850 ) ) ;
#24675 = CARTESIAN_POINT ( 'NONE',  ( -7.954856959092191815, 77.97268628210142083, -5.529263428287477744 ) ) ;
#24676 = LINE ( 'NONE', #26764, #18211 ) ;
#24677 = CARTESIAN_POINT ( 'NONE',  ( -0.1745138560723084320, 128.3898137178985621, -9.500000000000005329 ) ) ;
#24678 = CARTESIAN_POINT ( 'NONE',  ( 13.62178482187499640, 196.9531250006145342, -23.59362340125807123 ) ) ;
#24679 = DIRECTION ( 'NONE',  ( 0.000000000000000000, 0.000000000000000000, 1.000000000000000000 ) ) ;
#24680 = CARTESIAN_POINT ( 'NONE',  ( 5.778771075727756162E-15, 196.8218750006145399, 31.45816453501075927 ) ) ;
#24681 = LINE ( 'NONE', #16165, #28310 ) ;
#24682 = CARTESIAN_POINT ( 'NONE',  ( 22.56230152254412147, 7.347880794884125653E-16, -3.825000000000050804 ) ) ;
#24683 = CARTESIAN_POINT ( 'NONE',  ( -8.843639120294245259, 62.26481371789854791, -3.474262827703533230 ) ) ;
#24684 = ORIENTED_EDGE ( 'NONE', *, *, #14588, .F. ) ;
#24685 = CARTESIAN_POINT ( 'NONE',  ( 18.00000000000000000, 243.2312500012290570, -5.196152422706630247 ) ) ;
#24686 = CARTESIAN_POINT ( 'NONE',  ( -6.932735513424201912, 87.85231371789856780, 10.69584247140429412 ) ) ;
#24687 = EDGE_CURVE ( 'NONE', #28127, #13088, #30333, .T. ) ;
#24688 = CARTESIAN_POINT ( 'NONE',  ( 10.31873187879410736, 3.604726614523240613, -7.434374999385486404 ) ) ;
#24689 = DIRECTION ( 'NONE',  ( 0.000000000000000000, 0.000000000000000000, -1.000000000000000000 ) ) ;
#24690 = CARTESIAN_POINT ( 'NONE',  ( 15.24356964374999990, 3.323476615752268604, -7.490624999385497418 ) ) ;
#24691 = CARTESIAN_POINT ( 'NONE',  ( -11.48171059495408208, 42.71481371789855075, 4.944772684328421875 ) ) ;
#24692 = ORIENTED_EDGE ( 'NONE', *, *, #14594, .F. ) ;
#24693 = AXIS2_PLACEMENT_3D ( 'NONE', #10647, #13877, #25426 ) ;
#24694 = CARTESIAN_POINT ( 'NONE',  ( 18.12178482187500350, -4.985214923628407568, -6.815624999385455851 ) ) ;
#24695 = CARTESIAN_POINT ( 'NONE',  ( 8.715434833791931624, 27.66018628210144215, 8.962234695871760692 ) ) ;
#24696 = ADVANCED_FACE ( 'NONE', ( #35441 ), #21254, .F. ) ;
#24697 = CARTESIAN_POINT ( 'NONE',  ( 34.45992230116843302, 5.407089921784862696, 168.0291520325897636 ) ) ;
#24698 = CARTESIAN_POINT ( 'NONE',  ( -57.51711230271181563, 216.4690446883607535, -1.857196546604089393 ) ) ;
#24699 = ADVANCED_FACE ( 'NONE', ( #15554 ), #7032, .F. ) ;
#24700 = CARTESIAN_POINT ( 'NONE',  ( 24.62848410913218800, 0.000000000000000000, 160.3160426211468348 ) ) ;
#24701 = CARTESIAN_POINT ( 'NONE',  ( 0.1745138560722779009, 68.58981371789856496, 12.50000000000000355 ) ) ;
#24702 = CARTESIAN_POINT ( 'NONE',  ( -44.65997103062156981, 213.8393509191290889, 2.350049139982164359 ) ) ;
#24703 = CARTESIAN_POINT ( 'NONE',  ( -63.46205436395489841, 214.6737587650352168, 4.842901733360204908 ) ) ;
#24704 = VECTOR ( 'NONE', #23328, 1000.000000000000000 ) ;
#24705 = CARTESIAN_POINT ( 'NONE',  ( 1.069080835302379631E-14, 196.9624999999999773, 27.00000000000000000 ) ) ;
#24706 = CARTESIAN_POINT ( 'NONE',  ( -6.213268057914762998, 222.0587653132713228, -2.500000000000000000 ) ) ;
#24707 = CARTESIAN_POINT ( 'NONE',  ( -8.927990412390371944, 44.72731371789853938, -13.04141134922778988 ) ) ;
#24708 = CARTESIAN_POINT ( 'NONE',  ( -51.18377896937850835, 207.8379586601372750, 8.530955311639258909 ) ) ;
#24709 = CARTESIAN_POINT ( 'NONE',  ( -77.00000000000002842, 210.0000000000000000, -2.499999999999998668 ) ) ;
#24710 = CARTESIAN_POINT ( 'NONE',  ( -8.715434833791929847, 69.06018628210145494, -8.962234695871762469 ) ) ;
#24711 = CARTESIAN_POINT ( 'NONE',  ( -8.927990412390661490, 29.67268628210143788, 13.04141134922759804 ) ) ;
#24712 = CARTESIAN_POINT ( 'NONE',  ( 22.56230152254412147, -3.464101615137755275, -2.962500000000017675 ) ) ;
#24713 = CARTESIAN_POINT ( 'NONE',  ( -28.15924032180904035, 205.9842294738515420, -6.938746391785683976 ) ) ;
#24714 = ORIENTED_EDGE ( 'NONE', *, *, #36536, .F. ) ;
#24715 = AXIS2_PLACEMENT_3D ( 'NONE', #4632, #30426, #26492 ) ;
#24716 = CARTESIAN_POINT ( 'NONE',  ( -8.927990412390661490, 38.87268628210144072, 13.04141134922759804 ) ) ;
#24717 = CARTESIAN_POINT ( 'NONE',  ( 27.24356964374999279, 196.4656250006145797, -15.72908226750539207 ) ) ;
#24718 = DIRECTION ( 'NONE',  ( -0.8660254037844613562, -0.4999999999999605871, 0.000000000000000000 ) ) ;
#24719 = CARTESIAN_POINT ( 'NONE',  ( -42.28497103062156270, 204.4285982733020148, -3.350049139982115509 ) ) ;
#24720 = DIRECTION ( 'NONE',  ( -0.9925324990730152175, 0.1219804832088933616, 0.000000000000000000 ) ) ;
#24721 = CARTESIAN_POINT ( 'NONE',  ( 25.10239346032281560, -3.464101615137910262, 165.7328512920207402 ) ) ;
#24722 = CARTESIAN_POINT ( 'NONE',  ( 23.87821517812500005, 246.8593750006145342, 4.985214923628404016 ) ) ;
#24723 = CARTESIAN_POINT ( 'NONE',  ( -9.465287035748106703, 125.8023137178985706, 2.064181346179061460 ) ) ;
#24724 = CARTESIAN_POINT ( 'NONE',  ( 15.24356964374999990, 243.5593750006145228, 0.000000000000000000 ) ) ;
#24725 = ORIENTED_EDGE ( 'NONE', *, *, #1013, .F. ) ;
#24726 = PRESENTATION_STYLE_ASSIGNMENT (( #1789 ) ) ;
#24727 = CARTESIAN_POINT ( 'NONE',  ( -1.045839947578415010E-13, 196.5125000000000455, 27.00000000000000355 ) ) ;
#24728 = ADVANCED_FACE ( 'NONE', ( #11950 ), #36006, .F. ) ;
#24729 = CARTESIAN_POINT ( 'NONE',  ( 12.50000000000000355, 139.8898137178985621, -0.1745138560722771515 ) ) ;
#24730 = CARTESIAN_POINT ( 'NONE',  ( 10.31873187879410736, 0.000000000000000000, -6.440624999385525129 ) ) ;
#24731 = CARTESIAN_POINT ( 'NONE',  ( 30.90715669519676467, -7.209453229046475009, 163.2393191977598974 ) ) ;
#24732 = CARTESIAN_POINT ( 'NONE',  ( 0.5000000000000000000, 244.5000000000000000, -10.00000000000000000 ) ) ;
#24733 = CARTESIAN_POINT ( 'NONE',  ( 27.00000000000001066, 197.9375000000000284, 15.58845726811988897 ) ) ;
#24734 = ORIENTED_EDGE ( 'NONE', *, *, #14549, .F. ) ;
#24735 = CARTESIAN_POINT ( 'NONE',  ( 6.932735513423970097, 27.94768628210144001, 10.69584247140445044 ) ) ;
#24736 = ORIENTED_EDGE ( 'NONE', *, *, #10404, .F. ) ;
#24737 = VECTOR ( 'NONE', #34454, 1000.000000000000000 ) ;
#24738 = EDGE_LOOP ( 'NONE', ( #17801, #15277, #9639, #26592 ) ) ;
#24739 = CARTESIAN_POINT ( 'NONE',  ( 15.00000000000000000, 0.000000000000000000, -4.443749998770951670 ) ) ;
#24740 = CARTESIAN_POINT ( 'NONE',  ( 26.75643035624999655, -3.323476615752267271, -1.303124999385484095 ) ) ;
#24741 = DIRECTION ( 'NONE',  ( -0.000000000000000000, -1.000000000000000000, -0.000000000000000000 ) ) ;
#24742 = CARTESIAN_POINT ( 'NONE',  ( 0.000000000000000000, 195.0000000000000000, -28.99999999999999645 ) ) ;
#24743 = CARTESIAN_POINT ( 'NONE',  ( 23.87821517812500005, -4.985214923628404016, -9.890624999385478233 ) ) ;
#24744 = CARTESIAN_POINT ( 'NONE',  ( 12.46528703574805874, 72.79768628210146630, 2.660918448318279950 ) ) ;
#24745 = CARTESIAN_POINT ( 'NONE',  ( -15.50000000000000533, 6.489813717898557321, 0.1745138560722471477 ) ) ;
#24746 = CARTESIAN_POINT ( 'NONE',  ( 20.99999999999999289, 243.6437500012290229, -5.999999999999997335 ) ) ;
#24747 = CARTESIAN_POINT ( 'NONE',  ( 18.18132103106019315, 212.8186789689243881, 5.491377079899629976 ) ) ;
#24748 = CARTESIAN_POINT ( 'NONE',  ( -51.77752896937850124, 212.3500491399821613, 3.839350919129088435 ) ) ;
#24749 = LINE ( 'NONE', #5025, #16003 ) ;
#24750 = CARTESIAN_POINT ( 'NONE',  ( 25.17429694808935992, 3.464101615137752166, 166.5547119179464346 ) ) ;
#24751 = CARTESIAN_POINT ( 'NONE',  ( 4.944772684328420986, 123.2148137178985650, 11.48171059495408208 ) ) ;
#24752 = CARTESIAN_POINT ( 'NONE',  ( -49.80580436395490551, 216.5000000000000000, 0.1155267958017343610 ) ) ;
#24753 = CARTESIAN_POINT ( 'NONE',  ( -51.19122103062157692, 207.8379586601371329, -8.530955311639223382 ) ) ;
#24754 = CARTESIAN_POINT ( 'NONE',  ( 26.75643035624999655, 3.323476615752271268, -0.8906249993854854496 ) ) ;
#24755 = CARTESIAN_POINT ( 'NONE',  ( 27.24356964374999635, 196.4656250006145228, -15.72908226750539029 ) ) ;
#24756 = CARTESIAN_POINT ( 'NONE',  ( 13.23911966647199812, 122.3523137178985394, 8.632099005475788900 ) ) ;
#24757 = CARTESIAN_POINT ( 'NONE',  ( -48.21502896937850124, 215.5714017266979567, -3.350049139982168800 ) ) ;
#24758 = ORIENTED_EDGE ( 'NONE', *, *, #32027, .T. ) ;
#24759 = CARTESIAN_POINT ( 'NONE',  ( -47.00000000000000711, 252.0000000000000000, 5.000000000000000000 ) ) ;
#24760 = CARTESIAN_POINT ( 'NONE',  ( -2.660918448318275509, 130.2976862821014379, 12.46528703574805874 ) ) ;
#24761 = CARTESIAN_POINT ( 'NONE',  ( -5.770363421893818234, 78.83518628210146062, -14.38691631536207005 ) ) ;
#24762 = DIRECTION ( 'NONE',  ( 0.000000000000000000, 0.000000000000000000, -1.000000000000000000 ) ) ;
#24763 = CARTESIAN_POINT ( 'NONE',  ( 31.05913452161298949, -7.209453229046482114, 164.9764337025573866 ) ) ;
#24764 = CARTESIAN_POINT ( 'NONE',  ( 5.770363421893814682, 92.63518628210147199, 14.38691631536207183 ) ) ;
#24765 = CARTESIAN_POINT ( 'NONE',  ( -51.78497103062156981, 204.4285982733020148, -3.350049139982115509 ) ) ;
#24766 = CARTESIAN_POINT ( 'NONE',  ( 22.80587116629410360, 3.604726614523238837, -4.828124999385519978 ) ) ;
#24767 =( BOUNDED_CURVE ( )  B_SPLINE_CURVE ( 2, ( #9290, #9848, #32216, #7019, #1311, #26907, #20864 ),
 .UNSPECIFIED., .F., .F. ) 
 B_SPLINE_CURVE_WITH_KNOTS ( ( 3, 2, 2, 3 ),
 ( 0.5000000000000013323, 0.5072463768115947902, 0.5144927536231880261, 0.5217391304347814840 ),
 .UNSPECIFIED. ) 
 CURVE ( )  GEOMETRIC_REPRESENTATION_ITEM ( )  RATIONAL_B_SPLINE_CURVE ( ( 0.9999999999999753530, 0.8660254037844633546, 1.000000000000000000, 0.8660254037844387076, 1.000000000000000000, 0.8660254037844592467, 0.9999999999999794609 ) ) 
 REPRESENTATION_ITEM ( '' )  );
#24768 = CARTESIAN_POINT ( 'NONE',  ( 8.152565276336714462, 44.04768628210143788, -5.233372021372432847 ) ) ;
#24769 = ADVANCED_FACE ( 'NONE', ( #36188 ), #33542, .T. ) ;
#24770 = CARTESIAN_POINT ( 'NONE',  ( 18.00000000000000000, 246.3249999999999886, -5.196152422706630247 ) ) ;
#24771 = CARTESIAN_POINT ( 'NONE',  ( -42.08705436395490551, 203.8621396198270475, -6.307003348497942419 ) ) ;
#24772 = DIRECTION ( 'NONE',  ( 0.9961946980917462113, 0.000000000000000000, -0.08715574274765118534 ) ) ;
#24773 = CARTESIAN_POINT ( 'NONE',  ( -8.715434833791929847, 69.06018628210145494, -8.962234695871762469 ) ) ;
#24774 = DIRECTION ( 'NONE',  ( 0.000000000000000000, 0.000000000000000000, 1.000000000000000000 ) ) ;
#24775 = PLANE ( 'NONE',  #12336 ) ;
#24777 = CARTESIAN_POINT ( 'NONE',  ( 22.80587116629411781, 7.646167579472024665E-16, -1.321874999385519445 ) ) ;
#24776 = CARTESIAN_POINT ( 'NONE',  ( 8.710071997420127943, 36.28518628210144215, 3.796722387233375073 ) ) ;
#24778 = DIRECTION ( 'NONE',  ( 0.000000000000000000, -0.000000000000000000, -1.000000000000000000 ) ) ;
#24779 = EDGE_LOOP ( 'NONE', ( #25936, #12900, #17097, #12238, #30337, #25097 ) ) ;
#24780 = CARTESIAN_POINT ( 'NONE',  ( 26.99999999999999645, 7.347880794884117764E-16, -1.574999999999993072 ) ) ;
#24781 = CARTESIAN_POINT ( 'NONE',  ( 37.12860184164362209, -3.604726614523238837, 162.7138348986514131 ) ) ;
#24782 = CARTESIAN_POINT ( 'NONE',  ( 24.73307100032225136, 3.464101615137757051, 161.5114762576325802 ) ) ;
#24783 = CARTESIAN_POINT ( 'NONE',  ( 15.00000000000000000, 245.0499999999999829, 0.000000000000000000 ) ) ;
#24784 = CARTESIAN_POINT ( 'NONE',  ( 29.49992229830193935, 6.068759932216713615, 159.4323797615155058 ) ) ;
#24785 = ADVANCED_FACE ( 'NONE', ( #7771 ), #33973, .F. ) ;
#24786 = CARTESIAN_POINT ( 'NONE',  ( 11.48171059495408208, 84.11481371789855643, -4.944772684328420986 ) ) ;
#24787 = CARTESIAN_POINT ( 'NONE',  ( -7.228626920339070061, 94.07268628210145778, 10.49813415415989404 ) ) ;
#24788 = ORIENTED_EDGE ( 'NONE', *, *, #35521, .F. ) ;
#24789 = ORIENTED_EDGE ( 'NONE', *, *, #21788, .T. ) ;
#24790 = CARTESIAN_POINT ( 'NONE',  ( 13.50000000000001421, 198.0125000012290286, 23.38268590217984055 ) ) ;
#24791 = CARTESIAN_POINT ( 'NONE',  ( 18.00000000000000355, -5.196152422706632912, -3.975000000000006306 ) ) ;
#24792 = CARTESIAN_POINT ( 'NONE',  ( 5.770363421894130873, 64.56481371789854506, -14.38691631536193860 ) ) ;
#24793 = CARTESIAN_POINT ( 'NONE',  ( 26.75643035624999655, 3.323476615752271712, -7.640624999385485339 ) ) ;
#24794 = CARTESIAN_POINT ( 'NONE',  ( 23.87821517812499650, 244.3093750006145228, -4.985214923628404904 ) ) ;
#24795 =( BOUNDED_CURVE ( )  B_SPLINE_CURVE ( 2, ( #11270, #28324, #28690, #22841, #34388, #19999, #31543 ),
 .UNSPECIFIED., .F., .F. ) 
 B_SPLINE_CURVE_WITH_KNOTS ( ( 3, 2, 2, 3 ),
 ( 0.9130434782608709554, 0.9202898550724650795, 0.9275362318840590925, 0.9347826086956532166 ),
 .UNSPECIFIED. ) 
 CURVE ( )  GEOMETRIC_REPRESENTATION_ITEM ( )  RATIONAL_B_SPLINE_CURVE ( ( 0.9999999999999733546, 0.8660254037844653530, 1.000000000000000000, 0.8660254037844387076, 1.000000000000000000, 0.8660254037844202779, 1.000000000000018430 ) ) 
 REPRESENTATION_ITEM ( '' )  );
#24796 = CARTESIAN_POINT ( 'NONE',  ( -61.87872103062156981, 205.4690446883607535, 1.090244570138264368 ) ) ;
#24797 = CARTESIAN_POINT ( 'NONE',  ( 31.36063891923419789, -6.928203230275506996, 168.4226447368806987 ) ) ;
#24798 = CARTESIAN_POINT ( 'NONE',  ( 1.715153634034445762, 36.67731371789854933, -9.534712964251895073 ) ) ;
#24799 = CARTESIAN_POINT ( 'NONE',  ( 16.56230152254410726, -7.209453229046475009, -6.778124999385522820 ) ) ;
#24800 = CARTESIAN_POINT ( 'NONE',  ( 9.465287035748106703, 102.8023137178985422, -2.064181346179063237 ) ) ;
#24801 = CARTESIAN_POINT ( 'NONE',  ( 5.778771075727756162E-15, 198.6218750006145513, 31.45816453501075927 ) ) ;
#24802 = CARTESIAN_POINT ( 'NONE',  ( -12.46528703574811558, 24.60231371789854649, 2.660918448318003726 ) ) ;
#24803 = CARTESIAN_POINT ( 'NONE',  ( -8.962234695871760692, 75.96018628210144641, 8.715434833791933400 ) ) ;
#24804 = CARTESIAN_POINT ( 'NONE',  ( 13.56230152254411259, -5.196152422706632912, -8.812499998771039955 ) ) ;
#24805 = DIRECTION ( 'NONE',  ( 0.000000000000000000, 0.000000000000000000, -1.000000000000000000 ) ) ;
#24806 = CARTESIAN_POINT ( 'NONE',  ( 27.70246933682352974, 5.407089921784856479, 162.4280389384339855 ) ) ;
#24807 = CARTESIAN_POINT ( 'NONE',  ( 15.00000000000000000, 0.000000000000000000, -0.8437499987709595750 ) ) ;
#24808 = CARTESIAN_POINT ( 'NONE',  ( 22.80587116629411426, 3.604726614523243278, -7.134374999385543425 ) ) ;
#24809 = FACE_OUTER_BOUND ( 'NONE', #8154, .T. ) ;
#24810 = VECTOR ( 'NONE', #6988, 1000.000000000000000 ) ;
#24811 = CYLINDRICAL_SURFACE ( 'NONE', #24211, 4.899999999999999467 ) ;
#24812 = CARTESIAN_POINT ( 'NONE',  ( 8.843639120294328748, 90.33518628210144641, -3.474262827703334722 ) ) ;
#24813 = DIRECTION ( 'NONE',  ( 0.000000000000000000, 0.000000000000000000, 1.000000000000000000 ) ) ;
#24814 = CARTESIAN_POINT ( 'NONE',  ( 0.1745138560725515708, 125.4101862821014635, -12.50000000000000355 ) ) ;
#24815 = CARTESIAN_POINT ( 'NONE',  ( -98.52697526167153796, 63.53212182842481326, 5.000000000000000000 ) ) ;
#24816 = CARTESIAN_POINT ( 'NONE',  ( 23.87821517812499650, 249.2593750006145399, -4.985214923628404904 ) ) ;
#24817 = ORIENTED_EDGE ( 'NONE', *, *, #19453, .T. ) ;
#24818 = CARTESIAN_POINT ( 'NONE',  ( 27.99008328789078703, -5.407089921784859143, 165.7154814421367348 ) ) ;
#24819 = CARTESIAN_POINT ( 'NONE',  ( 15.24356964374999990, 3.323476615752268604, -4.678124999385468108 ) ) ;
#24820 = CARTESIAN_POINT ( 'NONE',  ( -13.62178482187500528, 196.6343750006145399, -23.59362340125807123 ) ) ;
#24821 = CARTESIAN_POINT ( 'NONE',  ( 28.46356835473687852, 5.196152422706636465, 169.7301163968956530 ) ) ;
#24822 = CYLINDRICAL_SURFACE ( 'NONE', #15634, 2.649999999999992806 ) ;
#24823 = CARTESIAN_POINT ( 'NONE',  ( 15.24356964374999990, 242.6593750006145171, 0.000000000000000000 ) ) ;
#24824 = CARTESIAN_POINT ( 'NONE',  ( 22.56230152254410370, 7.347880794884117764E-16, -6.862499998771004250 ) ) ;
#24825 = CARTESIAN_POINT ( 'NONE',  ( 8.962234695871567070, 131.8398137178985792, 8.715434833792127023 ) ) ;
#24826 = CARTESIAN_POINT ( 'NONE',  ( 27.24356964375000345, 195.1343750006145399, -3.336375036156643733E-15 ) ) ;
#24828 = EDGE_LOOP ( 'NONE', ( #19124, #3634, #4267, #29221 ) ) ;
#24827 = VERTEX_POINT ( 'NONE', #29049 ) ;
#24829 =( BOUNDED_CURVE ( )  B_SPLINE_CURVE ( 2, ( #27005, #21524, #27377, #18869, #1407, #9575, #18686 ),
 .UNSPECIFIED., .F., .F. ) 
 B_SPLINE_CURVE_WITH_KNOTS ( ( 3, 2, 2, 3 ),
 ( 0.1304347826086954820, 0.1376811594202895228, 0.1449275362318835914, 0.1521739130434776321 ),
 .UNSPECIFIED. ) 
 CURVE ( )  GEOMETRIC_REPRESENTATION_ITEM ( )  RATIONAL_B_SPLINE_CURVE ( ( 1.000000000000002887, 0.8660254037844354880, 1.000000000000000000, 0.8660254037844387076, 1.000000000000000000, 0.8660254037844504760, 0.9999999999999882316 ) ) 
 REPRESENTATION_ITEM ( '' )  );
#24830 = CARTESIAN_POINT ( 'NONE',  ( 23.87821517812500005, 244.9468750006145115, 4.985214923628404016 ) ) ;
#24831 = CARTESIAN_POINT ( 'NONE',  ( -81.00000000000002842, 206.0000000000000000, -2.499999999999998668 ) ) ;
#24832 = CARTESIAN_POINT ( 'NONE',  ( 21.00000000000000000, -6.646953231504538984, -4.528124999385448213 ) ) ;
#24833 = CARTESIAN_POINT ( 'NONE',  ( 10.83675517735179206, 111.1398137178985621, -11.08355503943118769 ) ) ;
#24834 = FACE_OUTER_BOUND ( 'NONE', #14634, .T. ) ;
#24835 = CARTESIAN_POINT ( 'NONE',  ( 18.00000000000000355, -5.196152422706632912, -9.318749998770941900 ) ) ;
#24836 = EDGE_CURVE ( 'NONE', #2146, #28321, #2752, .T. ) ;
#24837 = CARTESIAN_POINT ( 'NONE',  ( 13.44051670066911264, -5.407089921784865361, -5.971874999385562433 ) ) ;
#24838 = ORIENTED_EDGE ( 'NONE', *, *, #23044, .T. ) ;
#24839 = CARTESIAN_POINT ( 'NONE',  ( 5.727106289114498080E-15, 197.9750000012290343, 31.17691453623979214 ) ) ;
#24840 = VECTOR ( 'NONE', #29681, 1000.000000000000000 ) ;
#24841 = CARTESIAN_POINT ( 'NONE',  ( -10.49813415415989581, 123.9726862821014493, -7.228626920339068285 ) ) ;
#24842 = CARTESIAN_POINT ( 'NONE',  ( 10.31873187879411091, 3.604726614523236616, -1.078124999385534410 ) ) ;
#24843 = CARTESIAN_POINT ( 'NONE',  ( 27.61912665782109499, 5.407089921784862696, 161.4754277583837734 ) ) ;
#24844 = CARTESIAN_POINT ( 'NONE',  ( -52.96502896937850124, 217.3034525342667962, -4.350049139982195001 ) ) ;
#24845 = CARTESIAN_POINT ( 'NONE',  ( 15.24356964374999990, 247.9468750006145115, 0.000000000000000000 ) ) ;
#24846 = FILL_AREA_STYLE ('',( #19879 ) ) ;
#24847 = CARTESIAN_POINT ( 'NONE',  ( 24.00000000000000000, 240.2500000000000000, 5.196152422706629359 ) ) ;
#24848 = CARTESIAN_POINT ( 'NONE',  ( -36.93377896937849414, 208.9097554298617183, 4.530955311639234040 ) ) ;
#24850 = EDGE_CURVE ( 'NONE', #2674, #13240, #4197, .T. ) ;
#24849 = CARTESIAN_POINT ( 'NONE',  ( -12.53471296425194836, 132.0226862821014606, 2.311890736173176641 ) ) ;
#24851 = CARTESIAN_POINT ( 'NONE',  ( 13.56230152254410726, 5.196152422706630247, -0.8624999987709991434 ) ) ;
#24852 = EDGE_LOOP ( 'NONE', ( #28850, #24268, #8283, #15490 ) ) ;
#24853 = DIRECTION ( 'NONE',  ( -0.000000000000000000, -1.000000000000000000, -0.000000000000000000 ) ) ;
#24854 = AXIS2_PLACEMENT_3D ( 'NONE', #7632, #2488, #36609 ) ;
#24855 = CARTESIAN_POINT ( 'NONE',  ( 18.00000000000000000, 244.5250000000000057, -5.196152422706630247 ) ) ;
#24856 = EDGE_CURVE ( 'NONE', #5512, #6657, #9354, .T. ) ;
#24857 = CARTESIAN_POINT ( 'NONE',  ( 15.46528703574804986, 127.9976862821014265, 3.257655550457285720 ) ) ;
#24858 = DIRECTION ( 'NONE',  ( -0.000000000000000000, -0.000000000000000000, 1.000000000000000000 ) ) ;
#24859 = CARTESIAN_POINT ( 'NONE',  ( 2.660918448318279950, 15.29768628210143078, -12.46528703574805697 ) ) ;
#24860 = CARTESIAN_POINT ( 'NONE',  ( 22.56230152254411792, 7.347880794884125653E-16, -9.675000000000045119 ) ) ;
#24861 = ORIENTED_EDGE ( 'NONE', *, *, #19120, .T. ) ;
#24862 = CARTESIAN_POINT ( 'NONE',  ( 10.56230152254549104, -3.464101615138557300, -8.062500000000003553 ) ) ;
#24863 = CARTESIAN_POINT ( 'NONE',  ( 3.474262827703335166, 74.23518628210142367, 8.843639120294326972 ) ) ;
#24864 = DIRECTION ( 'NONE',  ( -0.000000000000000000, 1.000000000000000000, -0.000000000000000000 ) ) ;
#24865 = CARTESIAN_POINT ( 'NONE',  ( 2.064181346179061460, 132.7023137178985337, 9.465287035748106703 ) ) ;
#24866 = CARTESIAN_POINT ( 'NONE',  ( 13.62178482187499640, 196.0531250006145285, -23.59362340125807123 ) ) ;
#24867 = CARTESIAN_POINT ( 'NONE',  ( 14.99999999999989697, -3.464101615137695767, -2.212500000000015454 ) ) ;
#24868 = CARTESIAN_POINT ( 'NONE',  ( 5.778771075727756162E-15, 198.6218750006145513, 31.45816453501075927 ) ) ;
#24869 = LINE ( 'NONE', #36417, #22297 ) ;
#24870 = CARTESIAN_POINT ( 'NONE',  ( 22.60769515458672885, 242.2174038105676459, -5.999999999999998224 ) ) ;
#24871 = CARTESIAN_POINT ( 'NONE',  ( -5.529263428287297444, 63.12731371789852375, -7.954856959092311719 ) ) ;
#24872 = CARTESIAN_POINT ( 'NONE',  ( 21.00000000000000000, -6.928203230275506996, -9.337499999999982592 ) ) ;
#24873 = EDGE_LOOP ( 'NONE', ( #13933, #25798 ) ) ;
#24874 = CARTESIAN_POINT ( 'NONE',  ( 26.99999999999999645, 240.3812500012290343, -7.347880794884117764E-16 ) ) ;
#24875 = CARTESIAN_POINT ( 'NONE',  ( -11.48171059495408208, 70.31481371789854506, 4.944772684328421875 ) ) ;
#24876 = CARTESIAN_POINT ( 'NONE',  ( 19.68408634441911431, 5.407089921784862696, -7.096874999385549998 ) ) ;
#24877 = CARTESIAN_POINT ( 'NONE',  ( -8.668585281157772826, 143.0000000000000568, 10.14709209106742627 ) ) ;
#24878 = CARTESIAN_POINT ( 'NONE',  ( 21.00000000000000000, -6.646953231504538984, -6.440624999385486049 ) ) ;
#24879 = CARTESIAN_POINT ( 'NONE',  ( -10.69584247140429412, 34.95231371789854791, -6.932735513424201024 ) ) ;
#24880 = ADVANCED_FACE ( 'NONE', ( #809, #12380 ), #23950, .T. ) ;
#24881 = VECTOR ( 'NONE', #29550, 1000.000000000000000 ) ;
#24882 = ORIENTED_EDGE ( 'NONE', *, *, #128, .F. ) ;
#24883 = CARTESIAN_POINT ( 'NONE',  ( 23.87821517812500005, -4.985214923628404016, -7.190624999385470062 ) ) ;
#24884 = CARTESIAN_POINT ( 'NONE',  ( -8.962234695871760692, 20.76018628210144001, 8.715434833791933400 ) ) ;
#24885 = CARTESIAN_POINT ( 'NONE',  ( -30.99627896937850480, 203.4690446883607535, -1.626142955000504209 ) ) ;
#24886 = CARTESIAN_POINT ( 'NONE',  ( -55.53794563604516554, 205.3262412349647832, 4.842901733360250205 ) ) ;
#24887 =( NAMED_UNIT ( * ) SI_UNIT ( $, .STERADIAN. ) SOLID_ANGLE_UNIT ( ) );
#24888 = CARTESIAN_POINT ( 'NONE',  ( 16.56230152254411792, 6.928203230275514990, -9.562500000000060396 ) ) ;
#24889 = CARTESIAN_POINT ( 'NONE',  ( -2.660918448318004614, 72.90231371789855075, -12.46528703574811558 ) ) ;
#24890 = CARTESIAN_POINT ( 'NONE',  ( -39.71205436395491262, 213.2096571498974242, 3.378800118222489601 ) ) ;
#24892 = EDGE_CURVE ( 'NONE', #16979, #15602, #32842, .T. ) ;
#24891 = CARTESIAN_POINT ( 'NONE',  ( -55.54538769728823411, 211.8571965466039444, -6.469044688360768625 ) ) ;
#24893 = CARTESIAN_POINT ( 'NONE',  ( 16.56230152254411081, 6.928203230275506996, -1.799999998770985377 ) ) ;
#24894 = CARTESIAN_POINT ( 'NONE',  ( 10.56230152254410726, 0.000000000000000000, -6.300000000000055778 ) ) ;
#24895 = CARTESIAN_POINT ( 'NONE',  ( -15.53471296425188442, 43.57731371789854080, -2.908627838312459080 ) ) ;
#24896 = CARTESIAN_POINT ( 'NONE',  ( -44.65252896937850835, 205.6499508600178103, -7.303452534266820173 ) ) ;
#24897 = CARTESIAN_POINT ( 'NONE',  ( 2.311890736173175753, 65.32268628210144357, 12.53471296425194836 ) ) ;
#24898 = CARTESIAN_POINT ( 'NONE',  ( 6.092822981423978490, 6.385186282101440902, -14.25334919248782306 ) ) ;
#24899 = CARTESIAN_POINT ( 'NONE',  ( 22.56230152254412147, 3.464101615137759271, -1.087500000000040323 ) ) ;
#24900 = CARTESIAN_POINT ( 'NONE',  ( -27.00000000000000355, 197.4125000012290343, 0.000000000000000000 ) ) ;
#24901 = EDGE_LOOP ( 'NONE', ( #31619, #32651 ) ) ;
#24902 = CARTESIAN_POINT ( 'NONE',  ( 14.38691631536207538, 25.93518628210144072, -5.770363421893813793 ) ) ;
#24903 = CARTESIAN_POINT ( 'NONE',  ( -27.00000000000000355, 196.0250000012290457, -15.58845726811989429 ) ) ;
#24904 = CARTESIAN_POINT ( 'NONE',  ( 27.24356964374999635, 198.3218750006145399, -15.72908226750539029 ) ) ;
#24905 = CYLINDRICAL_SURFACE ( 'NONE', #14764, 3.500000000000002220 ) ;
#24906 = CARTESIAN_POINT ( 'NONE',  ( 15.00000000000000000, 0.000000000000000000, -5.343749998770963572 ) ) ;
#24907 = CARTESIAN_POINT ( 'NONE',  ( 21.00000000000000000, 247.8624999999999545, 5.999999999999998224 ) ) ;
#24908 = CARTESIAN_POINT ( 'NONE',  ( 21.00000000000000000, 248.6218750006145228, 6.646953231504538984 ) ) ;
#24909 = CARTESIAN_POINT ( 'NONE',  ( 1.715153634034445762, 110.2773137178985650, -9.534712964251895073 ) ) ;
#24910 = CARTESIAN_POINT ( 'NONE',  ( 20.99999999999999645, 243.2218750006145456, 6.646953231504538984 ) ) ;
#24911 = ORIENTED_EDGE ( 'NONE', *, *, #1847, .F. ) ;
#24912 = LINE ( 'NONE', #36464, #5079 ) ;
#24913 = EDGE_CURVE ( 'NONE', #1210, #21615, #27208, .T. ) ;
#24914 = CARTESIAN_POINT ( 'NONE',  ( 6.932735513424201024, 138.4523137178985621, -10.69584247140429412 ) ) ;
#24915 = CARTESIAN_POINT ( 'NONE',  ( 19.68408634441910365, 5.407089921784857367, -9.290624999385570959 ) ) ;
#24916 = CARTESIAN_POINT ( 'NONE',  ( 37.17272443640959523, -3.604726614523235284, 163.2181584645603323 ) ) ;
#24917 = CARTESIAN_POINT ( 'NONE',  ( 27.92756053683882911, -5.196152422706638241, 163.6035190036313622 ) ) ;
#24918 = CARTESIAN_POINT ( 'NONE',  ( 27.00000000000001066, 197.0374999999999943, 15.58845726811988897 ) ) ;
#24919 = ORIENTED_EDGE ( 'NONE', *, *, #13623, .F. ) ;
#24920 = CARTESIAN_POINT ( 'NONE',  ( -0.1745138560725500443, 38.01018628210144357, 12.50000000000000355 ) ) ;
#24921 = VERTEX_POINT ( 'NONE', #18653 ) ;
#24922 = ORIENTED_EDGE ( 'NONE', *, *, #3126, .T. ) ;
#24923 = CARTESIAN_POINT ( 'NONE',  ( 15.00000000000000178, -3.464101615137757051, -3.956249998770955845 ) ) ;
#24924 = CARTESIAN_POINT ( 'NONE',  ( 18.12178482187499640, 4.985214923628404904, -0.2156249993854608693 ) ) ;
#24925 = CARTESIAN_POINT ( 'NONE',  ( 20.99999999999997868, 210.0000000000000000, -5.999999999999999112 ) ) ;
#24926 = CARTESIAN_POINT ( 'NONE',  ( 26.99999999999999645, 7.347880794884117764E-16, -4.725000000000006750 ) ) ;
#24927 = CARTESIAN_POINT ( 'NONE',  ( 23.87821517812499650, 4.985214923628404904, -8.840624999385482852 ) ) ;
#24928 = CARTESIAN_POINT ( 'NONE',  ( 6.932735513423970097, 73.94768628210145778, 10.69584247140445044 ) ) ;
#24929 = CARTESIAN_POINT ( 'NONE',  ( 14.25334919248795451, 10.51481371789855679, -6.092822981423661410 ) ) ;
#24930 = CARTESIAN_POINT ( 'NONE',  ( -63.85044563604516554, 205.1570982666397072, -4.673758765035155527 ) ) ;
#24931 = CARTESIAN_POINT ( 'NONE',  ( 14.89154389910932252, 216.1084561008947844, 0.4848545222723734671 ) ) ;
#24932 = CARTESIAN_POINT ( 'NONE',  ( -55.14211230271182984, 205.5309553116392465, 1.321298161741817356 ) ) ;
#24933 = CARTESIAN_POINT ( 'NONE',  ( 37.07307153918868181, 7.347880794884117764E-16, 164.8737688849411143 ) ) ;
#24934 = CARTESIAN_POINT ( 'NONE',  ( -12.46528703574811558, 116.6023137178985678, 2.660918448318003726 ) ) ;
#24935 = CARTESIAN_POINT ( 'NONE',  ( -44.85788769728821990, 216.4690446883607535, 1.857196546604031662 ) ) ;
#24936 = CARTESIAN_POINT ( 'NONE',  ( -63.65997103062157692, 217.3034525342668815, 4.350049139982096413 ) ) ;
#24937 = CARTESIAN_POINT ( 'NONE',  ( 18.12178482187499640, 4.985214923628404904, -1.678124999385494087 ) ) ;
#24938 = CARTESIAN_POINT ( 'NONE',  ( 27.24356964375000345, 195.5281250006145228, -3.336375036156643733E-15 ) ) ;
#24939 = CARTESIAN_POINT ( 'NONE',  ( 14.25334919248795451, 93.31481371789855928, -6.092822981423661410 ) ) ;
#24940 = CARTESIAN_POINT ( 'NONE',  ( -46.23586230271182984, 206.8500491399821328, 5.686928522499748340 ) ) ;
#24941 = ORIENTED_EDGE ( 'NONE', *, *, #14339, .T. ) ;
#24942 = CARTESIAN_POINT ( 'NONE',  ( -4.944772684328673229, 130.5851862821014606, 11.48171059495397728 ) ) ;
#24943 = CARTESIAN_POINT ( 'NONE',  ( 3.257655550457285720, 61.29768628210142367, -15.46528703574804986 ) ) ;
#24944 = CARTESIAN_POINT ( 'NONE',  ( 37.07633987954135080, 3.464101615137969770, 164.9111261861195885 ) ) ;
#24945 = CARTESIAN_POINT ( 'NONE',  ( 27.85444716323975101, 5.407089921784862696, 164.1651534432314747 ) ) ;
#24946 = CARTESIAN_POINT ( 'NONE',  ( 8.927990412390657937, 89.47268628210143504, -13.04141134922759804 ) ) ;
#24947 = CARTESIAN_POINT ( 'NONE',  ( -50.39955436395489841, 214.8429017333601792, -4.673758765035197271 ) ) ;
#24948 = CARTESIAN_POINT ( 'NONE',  ( 22.80587116629410716, 3.604726614523238837, -6.628124999385534899 ) ) ;
#24949 = CARTESIAN_POINT ( 'NONE',  ( -9.465287035748065847, 31.39768628210144286, -2.064181346179273735 ) ) ;
#24950 = FACE_OUTER_BOUND ( 'NONE', #14457, .T. ) ;
#24951 = CARTESIAN_POINT ( 'NONE',  ( -61.48288769728821990, 203.5309553116391612, -1.857196546604028775 ) ) ;
#24952 = CARTESIAN_POINT ( 'NONE',  ( 24.73633934067528983, 0.000000000000000000, 161.5488335588110544 ) ) ;
#24953 = CARTESIAN_POINT ( 'NONE',  ( 6.932735513423970097, 55.54768628210144499, 10.69584247140445044 ) ) ;
#24954 = CARTESIAN_POINT ( 'NONE',  ( 19.56230152254412502, -5.196152422706635576, -8.400000000000073186 ) ) ;
#24955 = CARTESIAN_POINT ( 'NONE',  ( 13.56230152254410548, 5.196152422706636465, -6.825000000000025935 ) ) ;
#24957 = CARTESIAN_POINT ( 'NONE',  ( 19.68408634441911431, 5.407089921784862696, -0.7968749993855217539 ) ) ;
#24956 = CARTESIAN_POINT ( 'NONE',  ( -1.715153634034234598, 23.92268628210143788, -9.534712964251941258 ) ) ;
#24958 = CARTESIAN_POINT ( 'NONE',  ( 7.234628195640309123, 198.6299038117966802, -27.00000000000000711 ) ) ;
#24959 = EDGE_LOOP ( 'NONE', ( #36042, #26035, #4826, #22489 ) ) ;
#24960 = CARTESIAN_POINT ( 'NONE',  ( 15.00000000000000178, -3.464101615137757051, -2.212500000000014122 ) ) ;
#24961 = CARTESIAN_POINT ( 'NONE',  ( 30.92186422678543423, 7.209453229046482114, 163.4074270530628894 ) ) ;
#24962 = CARTESIAN_POINT ( 'NONE',  ( 36.79199426872038714, 3.464101615137759271, 161.6610409823708778 ) ) ;
#24963 = CARTESIAN_POINT ( 'NONE',  ( 15.00000000000000000, 243.6625000000000227, -3.464101615137752166 ) ) ;
#24964 = DIRECTION ( 'NONE',  ( -1.000000000000000000, -4.130293990420971855E-17, 0.000000000000000000 ) ) ;
#24965 = CARTESIAN_POINT ( 'NONE',  ( -11.48171059495408208, 88.71481371789855075, 4.944772684328421875 ) ) ;
#24966 = CARTESIAN_POINT ( 'NONE',  ( 6.932735513423970097, 92.34768628210144925, 10.69584247140445044 ) ) ;
#24967 = ORIENTED_EDGE ( 'NONE', *, *, #17548, .F. ) ;
#24968 = ORIENTED_EDGE ( 'NONE', *, *, #10058, .F. ) ;
#24969 = CARTESIAN_POINT ( 'NONE',  ( 13.50000000000001421, 199.3625000012290513, 23.38268590217984055 ) ) ;
#24970 = CARTESIAN_POINT ( 'NONE',  ( 19.39230484541326760, 248.7986538117967541, 5.999999999999998224 ) ) ;
#24971 = CARTESIAN_POINT ( 'NONE',  ( 8.927990412390371944, 58.52731371789855785, 13.04141134922778811 ) ) ;
#24972 = CARTESIAN_POINT ( 'NONE',  ( 26.75643035624999655, -3.323476615752267715, -9.065624999385498484 ) ) ;
#24973 = CARTESIAN_POINT ( 'NONE',  ( 23.87821517812500005, 246.4093750006145171, 4.985214923628404016 ) ) ;
#24974 = CARTESIAN_POINT ( 'NONE',  ( -62.27455436395490551, 206.6211998817774997, 3.209657149897401585 ) ) ;
#24975 = CARTESIAN_POINT ( 'NONE',  ( 25.37693404997770230, -3.464101615137787693, 168.8708645910097346 ) ) ;
#24976 = CARTESIAN_POINT ( 'NONE',  ( -8.843639120294245259, 43.86481371789854933, -3.474262827703533230 ) ) ;
#24977 = CARTESIAN_POINT ( 'NONE',  ( 22.80587116629410716, 3.604726614523238837, -7.978124999385491023 ) ) ;
#24978 = VECTOR ( 'NONE', #14026, 1000.000000000000000 ) ;
#24979 = CARTESIAN_POINT ( 'NONE',  ( 3.474262827703532341, 92.16481371789855359, -8.843639120294245259 ) ) ;
#24980 = CARTESIAN_POINT ( 'NONE',  ( -1.926257025242585782E-15, 197.4968750006145513, -31.45816453501075927 ) ) ;
#24981 = CARTESIAN_POINT ( 'NONE',  ( -11.48171059495408208, 15.11481371789855110, 4.944772684328421875 ) ) ;
#24982 = EDGE_CURVE ( 'NONE', #25851, #33921, #10284, .T. ) ;
#24983 =( BOUNDED_CURVE ( )  B_SPLINE_CURVE ( 2, ( #27253, #12472, #32369, #32747, #24415, #901, #24227 ),
 .UNSPECIFIED., .F., .F. ) 
 B_SPLINE_CURVE_WITH_KNOTS ( ( 3, 2, 2, 3 ),
 ( 0.6304347826086960094, 0.6376811594202902445, 0.6449275362318847016, 0.6521739130434790477 ),
 .UNSPECIFIED. ) 
 CURVE ( )  GEOMETRIC_REPRESENTATION_ITEM ( )  RATIONAL_B_SPLINE_CURVE ( ( 0.9999999999999938938, 0.8660254037844448138, 1.000000000000000000, 0.8660254037844387076, 1.000000000000000000, 0.8660254037844243857, 1.000000000000014433 ) ) 
 REPRESENTATION_ITEM ( '' )  );
#24984 = CARTESIAN_POINT ( 'NONE',  ( -11.61527771782819940, 58.13518628210144357, 4.622313124798574258 ) ) ;
#24985 = CARTESIAN_POINT ( 'NONE',  ( 22.56230152254410370, 3.464101615137755275, -8.174999998770983822 ) ) ;
#24986 = EDGE_CURVE ( 'NONE', #10609, #9065, #8084, .T. ) ;
#24987 = DIRECTION ( 'NONE',  ( 0.000000000000000000, 0.000000000000000000, 1.000000000000000000 ) ) ;
#24988 = CARTESIAN_POINT ( 'NONE',  ( 30.73066631613276556, 7.209453229046475009, 161.2220249341241072 ) ) ;
#24989 = CARTESIAN_POINT ( 'NONE',  ( 26.99999999999999645, 7.347880794884117764E-16, -1.068749998770962550 ) ) ;
#24990 = AXIS2_PLACEMENT_3D ( 'NONE', #394, #23530, #8249 ) ;
#24991 = CARTESIAN_POINT ( 'NONE',  ( 10.31873187879411091, -3.604726614523244610, -7.359374999385524418 ) ) ;
#24992 =( NAMED_UNIT ( * ) PLANE_ANGLE_UNIT ( ) SI_UNIT ( $, .RADIAN. ) );
#24993 = DIRECTION ( 'NONE',  ( 0.000000000000000000, 0.000000000000000000, 1.000000000000000000 ) ) ;
#24994 = CARTESIAN_POINT ( 'NONE',  ( 9.500000000000005329, 100.1101862821014521, 0.1745138560725188748 ) ) ;
#24995 = CARTESIAN_POINT ( 'NONE',  ( 13.56230152254410726, 5.196152422706636465, -5.925000000000041567 ) ) ;
#24996 = EDGE_CURVE ( 'NONE', #33325, #14550, #22762, .T. ) ;
#24997 = CARTESIAN_POINT ( 'NONE',  ( 8.962234695871762469, 117.3601862821014521, -8.715434833791931624 ) ) ;
#24998 = CARTESIAN_POINT ( 'NONE',  ( 15.24356964374999990, 0.000000000000000000, -0.1406249993854691294 ) ) ;
#24999 = CYLINDRICAL_SURFACE ( 'NONE', #16200, 27.00000000000000355 ) ;
#25000 = ORIENTED_EDGE ( 'NONE', *, *, #14263, .T. ) ;
#25001 = CARTESIAN_POINT ( 'NONE',  ( 37.25116460488249004, -3.604726614523235284, 164.1147336928428899 ) ) ;
#25002 = CARTESIAN_POINT ( 'NONE',  ( 26.75643035624999655, 7.049594010296217766E-16, -5.765624999385460470 ) ) ;
#25003 = CARTESIAN_POINT ( 'NONE',  ( 27.24356964375000700, 198.6968750006145115, 15.72908226750537075 ) ) ;
#25004 = CARTESIAN_POINT ( 'NONE',  ( 19.32307722456181409, 5.539345343143609490, -8.000000000000000000 ) ) ;
#25005 = CARTESIAN_POINT ( 'NONE',  ( 25.40634911304786314, -3.464101615137761048, 169.2070803003913397 ) ) ;
#25006 = DIRECTION ( 'NONE',  ( 1.000000000000000000, 0.000000000000000000, 2.312964634635742957E-16 ) ) ;
#25007 = CARTESIAN_POINT ( 'NONE',  ( 26.75643035624999655, 242.8843750006145115, -7.049594010296217766E-16 ) ) ;
#25008 = FACE_OUTER_BOUND ( 'NONE', #3754, .T. ) ;
#25009 =( BOUNDED_CURVE ( )  B_SPLINE_CURVE ( 2, ( #6196, #11881, #29311, #14919, #26468, #501, #12449 ),
 .UNSPECIFIED., .F., .F. ) 
 B_SPLINE_CURVE_WITH_KNOTS ( ( 3, 2, 2, 3 ),
 ( 0.3913043478260868069, 0.3985507246376819857, 0.4057971014492771644, 0.4130434782608723432 ),
 .UNSPECIFIED. ) 
 CURVE ( )  GEOMETRIC_REPRESENTATION_ITEM ( )  RATIONAL_B_SPLINE_CURVE ( ( 1.000000000000003109, 0.8660254037844357100, 1.000000000000000000, 0.8660254037844387076, 1.000000000000000000, 0.8660254037843874153, 1.000000000000051292 ) ) 
 REPRESENTATION_ITEM ( '' )  );
#25010 = CARTESIAN_POINT ( 'NONE',  ( 4.944772684328420986, 141.6148137178985849, 11.48171059495408208 ) ) ;
#25011 = CARTESIAN_POINT ( 'NONE',  ( 27.24356964374999279, 195.1718750006145342, -15.72908226750539207 ) ) ;
#25013 = VERTEX_POINT ( 'NONE', #9734 ) ;
#25012 = ORIENTED_EDGE ( 'NONE', *, *, #23303, .F. ) ;
#25014 = AXIS2_PLACEMENT_3D ( 'NONE', #18857, #30405, #13154 ) ;
#25015 = CARTESIAN_POINT ( 'NONE',  ( 15.24356964374999990, 243.4093750006145171, -3.323476615752268604 ) ) ;
#25016 = CARTESIAN_POINT ( 'NONE',  ( -4.622313124798826500, 13.96481371789853831, 11.61527771782809637 ) ) ;
#25017 = CARTESIAN_POINT ( 'NONE',  ( 26.75643035624999655, 7.049594010296217766E-16, -3.515624999385458249 ) ) ;
#25018 = CARTESIAN_POINT ( 'NONE',  ( -8.927990412390371944, 118.3273137178985763, -13.04141134922778988 ) ) ;
#25019 = CARTESIAN_POINT ( 'NONE',  ( 16.56230152254411436, 6.928203230275514990, -2.362500000000002043 ) ) ;
#25020 = CARTESIAN_POINT ( 'NONE',  ( 18.00000000000000000, 5.196152422706630247, -8.568749998770941900 ) ) ;
#25021 = CARTESIAN_POINT ( 'NONE',  ( 10.31873187879410736, 3.604726614523240613, -8.334374999385541827 ) ) ;
#25022 = VERTEX_POINT ( 'NONE', #1562 ) ;
#25023 = CARTESIAN_POINT ( 'NONE',  ( 13.62178482187499640, 195.1531250006145513, -23.59362340125807123 ) ) ;
#25024 = CARTESIAN_POINT ( 'NONE',  ( 12.46528703574805874, 109.5976862821014493, 2.660918448318279950 ) ) ;
#25025 = CARTESIAN_POINT ( 'NONE',  ( 19.68408634441911076, -5.407089921784855591, -1.340624999385559013 ) ) ;
#25026 = CARTESIAN_POINT ( 'NONE',  ( -37.13169563604516554, 210.1155267958018271, 8.500000000000003553 ) ) ;
#25027 = CARTESIAN_POINT ( 'NONE',  ( 26.75643035624999655, 243.6343750006144830, 3.323476615752267271 ) ) ;
#25028 = CARTESIAN_POINT ( 'NONE',  ( 10.56230152254352461, -3.464101615137419543, -7.499999998771012422 ) ) ;
#25029 = CARTESIAN_POINT ( 'NONE',  ( -34.16294563604517265, 213.2096571498974527, -3.378800118222469617 ) ) ;
#25030 = CARTESIAN_POINT ( 'NONE',  ( -12.50000000000000355, 132.3101862821014549, -0.1745138560725492671 ) ) ;
#25031 = CARTESIAN_POINT ( 'NONE',  ( 19.56230152254411081, -5.196152422706629359, -0.6374999987710516791 ) ) ;
#25032 = ORIENTED_EDGE ( 'NONE', *, *, #11222, .F. ) ;
#25033 = AXIS2_PLACEMENT_3D ( 'NONE', #31336, #31519, #3079 ) ;
#25034 = APPLICATION_CONTEXT ( 'automotive_design' ) ;
#25035 = DIRECTION ( 'NONE',  ( 0.000000000000000000, 0.000000000000000000, 1.000000000000000000 ) ) ;
#25036 = CARTESIAN_POINT ( 'NONE',  ( 1.069080835302379631E-14, 199.6625000000000227, 27.00000000000000000 ) ) ;
#25037 = CARTESIAN_POINT ( 'NONE',  ( 13.23911966647218996, 126.8476862821014635, -8.632099005475504683 ) ) ;
#25038 = UNCERTAINTY_MEASURE_WITH_UNIT (LENGTH_MEASURE( 1.000000000000000082E-05 ), #33824, 'distance_accuracy_value', 'NONE');
#25039 = CARTESIAN_POINT ( 'NONE',  ( 27.00000000000001421, 199.2874999999999943, 15.58845726811988897 ) ) ;
#25040 = CARTESIAN_POINT ( 'NONE',  ( -11.48171059495397373, 4.085186282101443744, -4.944772684328680334 ) ) ;
#25041 = CARTESIAN_POINT ( 'NONE',  ( 10.56230152254410726, 3.464101615137757051, -9.937500000000000000 ) ) ;
#25042 = VERTEX_POINT ( 'NONE', #21858 ) ;
#25043 = CARTESIAN_POINT ( 'NONE',  ( 19.56230152254412502, -5.196152422706635576, -3.450000000000091660 ) ) ;
#25044 = MECHANICAL_DESIGN_GEOMETRIC_PRESENTATION_REPRESENTATION (  '', ( #34135 ), #3257 ) ;
#25045 = CARTESIAN_POINT ( 'NONE',  ( -5.529263428287477744, 84.87268628210145494, 7.954856959092191815 ) ) ;
#25046 =( BOUNDED_CURVE ( )  B_SPLINE_CURVE ( 2, ( #15302, #32729, #1074, #26855, #14740, #321, #693, #32915, #12073 ),
 .UNSPECIFIED., .F., .F. ) 
 B_SPLINE_CURVE_WITH_KNOTS ( ( 3, 2, 2, 2, 3 ),
 ( 0.4673913043478261087, 0.4710144927536231707, 0.4782608695652174058, 0.4855072463768115854, 0.4891304347826087029 ),
 .UNSPECIFIED. ) 
 CURVE ( )  GEOMETRIC_REPRESENTATION_ITEM ( )  RATIONAL_B_SPLINE_CURVE ( ( 0.9330127018922194093, 0.9330127018922198534, 1.000000000000000000, 0.8660254037844387076, 1.000000000000000000, 0.8660254037844387076, 1.000000000000000000, 0.9330127018922194093, 0.9330127018922194093 ) ) 
 REPRESENTATION_ITEM ( '' )  );
#25047 = DIRECTION ( 'NONE',  ( -0.000000000000000000, 0.000000000000000000, 1.000000000000000000 ) ) ;
#25048 = CARTESIAN_POINT ( 'NONE',  ( -8.710071997420207879, 134.7148137178985507, 3.796722387233182339 ) ) ;
#25049 = CARTESIAN_POINT ( 'NONE',  ( 13.62178482187501416, 195.9031250006145513, 23.59362340125806767 ) ) ;
#25050 = CARTESIAN_POINT ( 'NONE',  ( 20.99999999999999645, -6.928203230275506996, -5.737500000000017586 ) ) ;
#25051 = CARTESIAN_POINT ( 'NONE',  ( 13.62178482187501416, 198.2093750006145285, 23.59362340125806767 ) ) ;
#25052 = CARTESIAN_POINT ( 'NONE',  ( 28.00600070531170971, -5.196152422706638241, 164.5000942319139483 ) ) ;
#25053 = AXIS2_PLACEMENT_3D ( 'NONE', #16073, #35957, #32742 ) ;
#25054 = CARTESIAN_POINT ( 'NONE',  ( 0.000000000000000000, 202.0000000000000000, 0.000000000000000000 ) ) ;
#25055 = CARTESIAN_POINT ( 'NONE',  ( -5.233372021372612259, 60.25231371789854506, 8.152565276336593669 ) ) ;
#25056 = CARTESIAN_POINT ( 'NONE',  ( 23.99999999999999645, 5.196152422706631135, -8.699999999999985079 ) ) ;
#25057 = ORIENTED_EDGE ( 'NONE', *, *, #33040, .F. ) ;
#25058 = CARTESIAN_POINT ( 'NONE',  ( 26.99999999999999645, 241.7687500012290229, -3.464101615137755275 ) ) ;
#25059 = CARTESIAN_POINT ( 'NONE',  ( -12.46528703574811558, 61.40231371789855785, 2.660918448318004170 ) ) ;
#25060 = CARTESIAN_POINT ( 'NONE',  ( 10.31873187879410736, 0.000000000000000000, -7.396874999385516958 ) ) ;
#25061 = CARTESIAN_POINT ( 'NONE',  ( -27.24356964374999635, 198.0406250006145399, 15.72908226750539384 ) ) ;
#25062 = CARTESIAN_POINT ( 'NONE',  ( 23.87821517812500005, -4.985214923628404016, -6.853124999385479477 ) ) ;
#25063 = CARTESIAN_POINT ( 'NONE',  ( 8.715434833792128799, 37.53981371789855359, -8.962234695871567070 ) ) ;
#25064 = EDGE_LOOP ( 'NONE', ( #28503, #19786, #19987, #23181 ) ) ;
#25065 = CARTESIAN_POINT ( 'NONE',  ( 10.31873187879410736, 3.604726614523240613, -1.584374999385509630 ) ) ;
#25066 = CARTESIAN_POINT ( 'NONE',  ( -6.932735513423968321, 4.947686282101432909, -10.69584247140445221 ) ) ;
#25067 = CARTESIAN_POINT ( 'NONE',  ( -74.35000000000002274, 210.0000000000000000, -3.000000000000000000 ) ) ;
#25068 = CARTESIAN_POINT ( 'NONE',  ( -59.69419563604516554, 203.5000000000000000, 0.1155267958017914542 ) ) ;
#25069 = AXIS2_PLACEMENT_3D ( 'NONE', #2577, #34418, #25700 ) ;
#25070 =( NAMED_UNIT ( * ) PLANE_ANGLE_UNIT ( ) SI_UNIT ( $, .RADIAN. ) );
#25071 = PRODUCT_DEFINITION_FORMATION_WITH_SPECIFIED_SOURCE ( 'ANY', '', #17435, .NOT_KNOWN. ) ;
#25072 = CARTESIAN_POINT ( 'NONE',  ( 22.56230152254411792, 7.347880794884125653E-16, -9.675000000000045119 ) ) ;
#25073 = CARTESIAN_POINT ( 'NONE',  ( -8.715434833792127023, 60.53981371789856070, 8.962234695871568846 ) ) ;
#25074 = CARTESIAN_POINT ( 'NONE',  ( -37.93080436395490551, 205.4999999999999716, -0.1155267958017894420 ) ) ;
#25075 = CARTESIAN_POINT ( 'NONE',  ( -59.30580436395489841, 216.5000000000000000, 0.1155267958017343610 ) ) ;
#25076 = CARTESIAN_POINT ( 'NONE',  ( 22.56230152254410370, 7.347880794884117764E-16, -1.912499998771022280 ) ) ;
#25077 = CARTESIAN_POINT ( 'NONE',  ( 16.56230152254411081, -6.928203230275514990, -6.187500000000013323 ) ) ;
#25078 = CARTESIAN_POINT ( 'NONE',  ( 8.632099005475788900, 46.45231371789854791, -13.23911966647199812 ) ) ;
#25079 = CARTESIAN_POINT ( 'NONE',  ( -69.59747103062156270, 214.3500491399821044, -7.303452534266878793 ) ) ;
#25080 = CARTESIAN_POINT ( 'NONE',  ( 4.944772684328679446, 24.78518628210143859, -11.48171059495397373 ) ) ;
#25081 = CARTESIAN_POINT ( 'NONE',  ( 16.56230152254411436, 6.928203230275514990, -8.212500000000009237 ) ) ;
#25082 = CARTESIAN_POINT ( 'NONE',  ( -4.622313124798576922, 69.63518628210145778, -11.61527771782819762 ) ) ;
#25083 = CARTESIAN_POINT ( 'NONE',  ( 8.632099005475504683, 9.547686282101452093, 13.23911966647218996 ) ) ;
#25084 = CARTESIAN_POINT ( 'NONE',  ( 16.56230152254411436, 6.928203230275514990, -1.012500000000046585 ) ) ;
#25085 = CARTESIAN_POINT ( 'NONE',  ( -28.01712176579047764, 207.1685799127409382, -7.486769987355970102 ) ) ;
#25086 = EDGE_LOOP ( 'NONE', ( #4849, #7241, #29672, #17281 ) ) ;
#25087 = CARTESIAN_POINT ( 'NONE',  ( -15.46528703574804986, 31.39768628210144286, -3.257655550457287497 ) ) ;
#25088 = CARTESIAN_POINT ( 'NONE',  ( -27.24356964375000345, 196.1656250006145399, -15.72908226750537786 ) ) ;
#25089 = CARTESIAN_POINT ( 'NONE',  ( -27.24356964374999990, 198.0218750006145569, -15.72908226750537786 ) ) ;
#25090 = DIRECTION ( 'NONE',  ( 0.000000000000000000, 0.000000000000000000, -1.000000000000000000 ) ) ;
#25091 = CARTESIAN_POINT ( 'NONE',  ( 27.00000000000001421, 195.3500000012290343, 15.58845726811988897 ) ) ;
#25092 = DIRECTION ( 'NONE',  ( -0.9933043639548644332, 0.1155267958017622554, 0.000000000000000000 ) ) ;
#25093 = CARTESIAN_POINT ( 'NONE',  ( 31.08609832957909092, -6.928203230275506996, 165.2846314378917043 ) ) ;
#25094 = CARTESIAN_POINT ( 'NONE',  ( 21.00000000000000000, 248.1718750006145342, 6.646953231504538984 ) ) ;
#25095 = CARTESIAN_POINT ( 'NONE',  ( -3.474262827703527901, 105.9648137178985650, 8.843639120294245259 ) ) ;
#25096 = CARTESIAN_POINT ( 'NONE',  ( 18.12178482187499640, 245.2843750006145456, -4.985214923628404904 ) ) ;
#25097 = ORIENTED_EDGE ( 'NONE', *, *, #2962, .F. ) ;
#25098 = CARTESIAN_POINT ( 'NONE',  ( 6.000769315822030740E-16, 141.0000000000000000, -4.899999999999999467 ) ) ;
#25099 = CARTESIAN_POINT ( 'NONE',  ( 21.00000000000000000, 248.1437500012290513, -6.928203230275506996 ) ) ;
#25100 = CARTESIAN_POINT ( 'NONE',  ( 10.49813415416005213, 120.6273137178985593, -7.228626920338837358 ) ) ;
#25101 = CARTESIAN_POINT ( 'NONE',  ( 13.44051670066911264, 5.407089921784856479, -8.765624999385545735 ) ) ;
#25102 = CARTESIAN_POINT ( 'NONE',  ( 37.06160086440634416, 3.604726614523238837, 161.9480102244933732 ) ) ;
#25103 = CARTESIAN_POINT ( 'NONE',  ( 23.87821517812500005, -4.985214923628404016, -0.5531249993854792102 ) ) ;
#25104 = CARTESIAN_POINT ( 'NONE',  ( 27.00000000000000355, 196.6250000000000284, -3.306546357697854128E-15 ) ) ;
#25105 = ADVANCED_FACE ( 'NONE', ( #33411 ), #5404, .T. ) ;
#25106 = ORIENTED_EDGE ( 'NONE', *, *, #29738, .F. ) ;
#25107 = CARTESIAN_POINT ( 'NONE',  ( 11.61527771782819940, 25.93518628210143717, -4.622313124798573369 ) ) ;
#25108 = ORIENTED_EDGE ( 'NONE', *, *, #13141, .T. ) ;
#25109 = EDGE_LOOP ( 'NONE', ( #26362, #4074, #5134, #35595 ) ) ;
#25110 = CARTESIAN_POINT ( 'NONE',  ( 18.00000000000000355, -5.196152422706632912, -4.368749998770960374 ) ) ;
#25111 = CARTESIAN_POINT ( 'NONE',  ( 26.75643035624999655, -3.323476615752267271, -3.553124999385494753 ) ) ;
#25112 = CARTESIAN_POINT ( 'NONE',  ( -7.234628195640307347, 199.1200961906613713, -27.00000000000000711 ) ) ;
#25113 = CARTESIAN_POINT ( 'NONE',  ( 10.56230152254410903, 7.347880794884117764E-16, -10.00000000000000000 ) ) ;
#25114 = CARTESIAN_POINT ( 'NONE',  ( 26.75643035624999655, 248.5843750006145001, 3.323476615752267715 ) ) ;
#25115 = CARTESIAN_POINT ( 'NONE',  ( -12.46528703574805697, 58.99768628210144783, -2.660918448318280838 ) ) ;
#25116 = CARTESIAN_POINT ( 'NONE',  ( -5.770363421893818234, 134.0351862821014493, -14.38691631536207005 ) ) ;
#25117 = CARTESIAN_POINT ( 'NONE',  ( -68.00669563604516554, 209.8844732041982013, -6.500000000000000888 ) ) ;
#25118 = ADVANCED_FACE ( 'NONE', ( #14718 ), #14904, .T. ) ;
#25119 = CARTESIAN_POINT ( 'NONE',  ( 5.409584567222309737, 215.8464057872915305, 1.363118671454217390 ) ) ;
#25120 =( BOUNDED_CURVE ( )  B_SPLINE_CURVE ( 2, ( #2114, #10276, #36791, #28081, #13310, #30751, #13494 ),
 .UNSPECIFIED., .F., .F. ) 
 B_SPLINE_CURVE_WITH_KNOTS ( ( 3, 2, 2, 3 ),
 ( 0.1086956521739118053, 0.1159420289855061098, 0.1231884057971004143, 0.1304347826086947049 ),
 .UNSPECIFIED. ) 
 CURVE ( )  GEOMETRIC_REPRESENTATION_ITEM ( )  RATIONAL_B_SPLINE_CURVE ( ( 1.000000000000022871, 0.8660254037844159480, 1.000000000000000000, 0.8660254037844387076, 1.000000000000000000, 0.8660254037844561381, 0.9999999999999825695 ) ) 
 REPRESENTATION_ITEM ( '' )  );
#25121 = CARTESIAN_POINT ( 'NONE',  ( -52.76711230271184405, 214.4690446883608104, -1.321298161741814914 ) ) ;
#25122 = CARTESIAN_POINT ( 'NONE',  ( 28.04195244930222586, 5.196152422706630247, 164.9110245461011743 ) ) ;
#25123 = CARTESIAN_POINT ( 'NONE',  ( 2.311890736173452865, 119.4773137178985678, -12.53471296425189152 ) ) ;
#25124 = CARTESIAN_POINT ( 'NONE',  ( -38.92038769728823411, 208.1428034533959703, 6.469044688360770401 ) ) ;
#25125 = CARTESIAN_POINT ( 'NONE',  ( -57.72247103062156270, 205.6499508600178956, 7.303452534266880569 ) ) ;
#25126 = ADVANCED_FACE ( 'NONE', ( #26641 ), #29106, .F. ) ;
#25127 = CARTESIAN_POINT ( 'NONE',  ( 15.24356964375000167, -3.323476615752272600, -2.915624999385482141 ) ) ;
#25128 = CARTESIAN_POINT ( 'NONE',  ( 27.24356964375000700, 196.3906250006145058, 15.72908226750537075 ) ) ;
#25129 = CARTESIAN_POINT ( 'NONE',  ( -3.257655550456946880, 100.5023137178985451, -15.46528703574811736 ) ) ;
#25130 = CARTESIAN_POINT ( 'NONE',  ( -67.61086230271183695, 214.1499508600178387, -7.418979330068641964 ) ) ;
#25131 = ADVANCED_FACE ( 'NONE', ( #6182 ), #9778, .F. ) ;
#25132 = ORIENTED_EDGE ( 'NONE', *, *, #12154, .F. ) ;
#25133 = CARTESIAN_POINT ( 'NONE',  ( 36.82794601260381029, 7.347880794884125653E-16, 162.0719712953337250 ) ) ;
#25134 = CARTESIAN_POINT ( 'NONE',  ( 11.61527771782819940, 127.1351862821014578, -4.622313124798573369 ) ) ;
#25135 = CARTESIAN_POINT ( 'NONE',  ( -14.38691631536207183, 67.33518628210143220, 5.770363421893814682 ) ) ;
#25136 = AXIS2_PLACEMENT_3D ( 'NONE', #35999, #10036, #10595 ) ;
#25137 = CARTESIAN_POINT ( 'NONE',  ( -79.65000000000001990, 210.0000000000000000, -2.499999999999998668 ) ) ;
#25138 = CARTESIAN_POINT ( 'NONE',  ( 24.71185827157421855, 0.000000000000000000, 164.0636619062959483 ) ) ;
#25139 = CARTESIAN_POINT ( 'NONE',  ( 13.23911966647218996, 80.84768628210143504, -8.632099005475504683 ) ) ;
#25140 = CARTESIAN_POINT ( 'NONE',  ( -45.64955436395490551, 214.8429017333601792, -4.673758765035197271 ) ) ;
#25141 = CARTESIAN_POINT ( 'NONE',  ( 10.31873187879411091, 3.604726614523236616, -7.378124999385539340 ) ) ;
#25142 = CARTESIAN_POINT ( 'NONE',  ( -5.233372021372430183, 14.14768628210144286, -8.152565276336710909 ) ) ;
#25143 = CARTESIAN_POINT ( 'NONE',  ( 16.56230152254411436, -6.928203230275514990, -7.537500000000000533 ) ) ;
#25144 = CARTESIAN_POINT ( 'NONE',  ( -58.51413769728823411, 213.1499508600178672, 5.686928522499718142 ) ) ;
#25145 = CARTESIAN_POINT ( 'NONE',  ( -13.50000000000000533, 198.6875000012290400, -23.38268590217984411 ) ) ;
#25146 = CARTESIAN_POINT ( 'NONE',  ( 0.1745138560725515708, 61.01018628210145067, -12.50000000000000355 ) ) ;
#25147 = CARTESIAN_POINT ( 'NONE',  ( 5.727106289114498080E-15, 197.4124999999999943, 31.17691453623979214 ) ) ;
#25148 = FACE_OUTER_BOUND ( 'NONE', #35812, .T. ) ;
#25150 = CARTESIAN_POINT ( 'NONE',  ( 10.31873187879410736, -3.604726614523244610, -1.959374999385511407 ) ) ;
#25149 = CARTESIAN_POINT ( 'NONE',  ( -8.710071997420127943, 22.48518628210144499, -3.796722387233380402 ) ) ;
#25151 = CARTESIAN_POINT ( 'NONE',  ( 15.00000000000000000, 0.000000000000000000, -6.243749998770947940 ) ) ;
#25152 = ORIENTED_EDGE ( 'NONE', *, *, #13589, .F. ) ;
#25153 = CARTESIAN_POINT ( 'NONE',  ( 23.99999999999999645, 5.196152422706631135, -2.400000000000013234 ) ) ;
#25154 = CARTESIAN_POINT ( 'NONE',  ( 22.62369653919286350, -5.721836169135973371, -7.999999999999998224 ) ) ;
#25155 = CARTESIAN_POINT ( 'NONE',  ( 24.35887751344623098, 0.000000000000000000, 160.0290733790243962 ) ) ;
#25156 = CARTESIAN_POINT ( 'NONE',  ( 16.56230152254411436, -7.209453229046475009, -1.378124999385542226 ) ) ;
#25157 = CARTESIAN_POINT ( 'NONE',  ( 36.63511393177462594, 3.464101615137759271, 159.8678905258057341 ) ) ;
#25158 = CARTESIAN_POINT ( 'NONE',  ( 26.99999999999999645, 243.9250000000000114, -7.347880794884117764E-16 ) ) ;
#25159 = DIRECTION ( 'NONE',  ( -0.9925324990730154395, 0.1219804832088915297, 0.000000000000000000 ) ) ;
#25160 = CARTESIAN_POINT ( 'NONE',  ( 11.61527771782809637, 85.26481371789856212, 4.622313124798827388 ) ) ;
#25161 = CARTESIAN_POINT ( 'NONE',  ( 10.49813415415989581, 82.57268628210145778, 7.228626920339069173 ) ) ;
#25162 = VERTEX_POINT ( 'NONE', #21167 ) ;
#25163 = ORIENTED_EDGE ( 'NONE', *, *, #22903, .F. ) ;
#25164 = CARTESIAN_POINT ( 'NONE',  ( 27.00000000000001066, 197.1500000012290172, 15.58845726811988897 ) ) ;
#25165 = PLANE ( 'NONE',  #33193 ) ;
#25166 = EDGE_CURVE ( 'NONE', #13240, #30190, #23576, .T. ) ;
#25167 = CARTESIAN_POINT ( 'NONE',  ( -14.38691631536193860, 53.06481371789855928, -5.770363421894132649 ) ) ;
#25168 = CARTESIAN_POINT ( 'NONE',  ( 23.87821517812500005, -4.985214923628404016, -10.00312499938549315 ) ) ;
#25169 = CIRCLE ( 'NONE', #24571, 5.500000000000005329 ) ;
#25170 = EDGE_CURVE ( 'NONE', #4445, #12908, #12160, .T. ) ;
#25171 = CARTESIAN_POINT ( 'NONE',  ( 26.75643035624999655, 242.4343750006145513, -7.049594010296217766E-16 ) ) ;
#25172 = CARTESIAN_POINT ( 'NONE',  ( -54.55580436395489841, 214.5000000000000284, 0.1155267958017899832 ) ) ;
#25173 = CARTESIAN_POINT ( 'NONE',  ( 25.37366570962461054, 0.000000000000000000, 168.8335072898312887 ) ) ;
#25174 = CARTESIAN_POINT ( 'NONE',  ( -8.152565276336593669, 34.95231371789854080, -5.233372021372610483 ) ) ;
#25175 = EDGE_CURVE ( 'NONE', #33950, #31726, #25169, .T. ) ;
#25176 = CARTESIAN_POINT ( 'NONE',  ( 34.08121910445329661, 5.196152422706637353, 165.0978788107812818 ) ) ;
#25177 = CARTESIAN_POINT ( 'NONE',  ( -9.500000000000005329, 89.28981371789856780, 0.1745138560723101806 ) ) ;
#25178 = CARTESIAN_POINT ( 'NONE',  ( 27.24356964375000345, 198.2843750006145456, -3.336375036156643733E-15 ) ) ;
#25179 = CARTESIAN_POINT ( 'NONE',  ( -7.228626920338836470, 7.927313717898537782, -10.49813415416005213 ) ) ;
#25180 = CARTESIAN_POINT ( 'NONE',  ( 10.49813415415989581, 73.37268628210144072, 7.228626920339068285 ) ) ;
#25181 = CARTESIAN_POINT ( 'NONE',  ( 22.56230152254411436, -3.464101615137751278, -9.599999998771028942 ) ) ;
#25182 = CARTESIAN_POINT ( 'NONE',  ( 25.08932009880328096, 0.000000000000000000, 165.5834220860826349 ) ) ;
#25183 = CARTESIAN_POINT ( 'NONE',  ( 24.59910052939444824, 0.000000000000000000, 162.7748350156397521 ) ) ;
#25184 = CARTESIAN_POINT ( 'NONE',  ( 10.31873187879410558, -3.604726614523244610, -10.05937499938549884 ) ) ;
#25185 = CARTESIAN_POINT ( 'NONE',  ( 10.31873187879410558, 3.604726614523240613, -5.634374999385534544 ) ) ;
#25186 = CARTESIAN_POINT ( 'NONE',  ( 33.59750473220383071, -5.196152422706635576, 159.5689982363720674 ) ) ;
#25187 = CARTESIAN_POINT ( 'NONE',  ( 30.71350752933288675, 6.928203230275506996, 161.0258991035495058 ) ) ;
#25188 = CARTESIAN_POINT ( 'NONE',  ( -5.233372021372430183, 96.94768628210147199, -8.152565276336710909 ) ) ;
#25189 = CARTESIAN_POINT ( 'NONE',  ( 25.20698035151260896, 0.000000000000000000, 166.9282849285064856 ) ) ;
#25190 = AXIS2_PLACEMENT_3D ( 'NONE', #8136, #36916, #28213 ) ;
#25191 = CARTESIAN_POINT ( 'NONE',  ( 4.944772684328679446, 107.5851862821014464, -11.48171059495397373 ) ) ;
#25192 = CARTESIAN_POINT ( 'NONE',  ( -7.234628195640263826, 197.2075961894323370, -27.00000000000003553 ) ) ;
#25193 = CARTESIAN_POINT ( 'NONE',  ( 26.99999999999999645, 240.3437500012290116, 3.464101615137751278 ) ) ;
#25194 = ORIENTED_EDGE ( 'NONE', *, *, #29038, .F. ) ;
#25195 = CARTESIAN_POINT ( 'NONE',  ( 27.91164311941789933, -5.407089921784859143, 164.8189062138541772 ) ) ;
#25196 = CARTESIAN_POINT ( 'NONE',  ( 15.24356964374999990, 3.323476615752268604, -5.578124999385491556 ) ) ;
#25197 = CARTESIAN_POINT ( 'NONE',  ( 27.24356964375000700, 197.7968750006145342, 15.72908226750537075 ) ) ;
#25198 = CARTESIAN_POINT ( 'NONE',  ( 15.26092559546365734, -1.672032278976862685, -8.000000000000001776 ) ) ;
#25199 = CARTESIAN_POINT ( 'NONE',  ( 34.39497977834484743, 5.196152422706637353, 168.6841797239115976 ) ) ;
#25200 = CARTESIAN_POINT ( 'NONE',  ( 2.999999999999997335, 244.5000000000000000, -2.500000000000000000 ) ) ;
#25201 = CARTESIAN_POINT ( 'NONE',  ( 15.00000000000000178, 249.5875000000000341, 3.464101615137757051 ) ) ;
#25202 = CARTESIAN_POINT ( 'NONE',  ( 10.56230152254379817, -3.464101615137573198, -7.049999998771014909 ) ) ;
#25203 = CARTESIAN_POINT ( 'NONE',  ( -2.660918448318004614, 137.3023137178985564, -12.46528703574811558 ) ) ;
#25204 = CARTESIAN_POINT ( 'NONE',  ( -27.24356964375000345, 195.8093750006145513, 0.000000000000000000 ) ) ;
#25206 = ORIENTED_EDGE ( 'NONE', *, *, #17513, .T. ) ;
#25205 = ORIENTED_EDGE ( 'NONE', *, *, #33134, .T. ) ;
#25207 = CARTESIAN_POINT ( 'NONE',  ( 26.75643035624999655, 244.0843750006145285, 3.323476615752267715 ) ) ;
#25208 = AXIS2_PLACEMENT_3D ( 'NONE', #36073, #10300, #4236 ) ;
#25209 = DIRECTION ( 'NONE',  ( 0.000000000000000000, 0.000000000000000000, 1.000000000000000000 ) ) ;
#25210 = EDGE_CURVE ( 'NONE', #21, #113, #301, .T. ) ;
#25211 = CARTESIAN_POINT ( 'NONE',  ( 26.75643035624999655, -3.323476615752267715, -4.003124999385458516 ) ) ;
#25212 = CARTESIAN_POINT ( 'NONE',  ( 15.50000000000000533, 121.4898137178985564, -0.1745138560722452326 ) ) ;
#25213 = PLANE ( 'NONE',  #18623 ) ;
#25214 = CARTESIAN_POINT ( 'NONE',  ( 26.75643035624999655, 7.049594010296217766E-16, -1.378124999385471616 ) ) ;
#25215 = CARTESIAN_POINT ( 'NONE',  ( 22.80587116629411426, 7.646167579472024665E-16, -8.071874999385524774 ) ) ;
#25216 = CARTESIAN_POINT ( 'NONE',  ( -26.99999999999998934, 199.2500000012290116, 15.58845726811991561 ) ) ;
#25217 = CARTESIAN_POINT ( 'NONE',  ( 4.944772684328679446, 107.5851862821014464, -11.48171059495397373 ) ) ;
#25218 = DIRECTION ( 'NONE',  ( -0.000000000000000000, 0.000000000000000000, 1.000000000000000000 ) ) ;
#25219 =( BOUNDED_CURVE ( )  B_SPLINE_CURVE ( 2, ( #27002, #4250, #18300, #27565, #9571, #21885, #21703 ),
 .UNSPECIFIED., .F., .F. ) 
 B_SPLINE_CURVE_WITH_KNOTS ( ( 3, 2, 2, 3 ),
 ( 0.02173913043478281626, 0.02898550724637714154, 0.03623188405797146683, 0.04347826086956579211 ),
 .UNSPECIFIED. ) 
 CURVE ( )  GEOMETRIC_REPRESENTATION_ITEM ( )  RATIONAL_B_SPLINE_CURVE ( ( 0.9999999999999961142, 0.8660254037844425934, 1.000000000000000000, 0.8660254037844387076, 1.000000000000000000, 0.8660254037844280495, 1.000000000000010658 ) ) 
 REPRESENTATION_ITEM ( '' )  );
#25220 = CARTESIAN_POINT ( 'NONE',  ( -39.30877896937850124, 212.1620413398627534, -8.530955311639255356 ) ) ;
#25221 = CARTESIAN_POINT ( 'NONE',  ( 26.75643035624999655, 245.5093750006145115, -3.323476615752271268 ) ) ;
#25222 = CARTESIAN_POINT ( 'NONE',  ( 10.56230152254548926, 3.464101615138548862, -2.624999998770999543 ) ) ;
#25223 = CARTESIAN_POINT ( 'NONE',  ( -35.35044563604517265, 206.6211998817775566, -3.209657149897419348 ) ) ;
#25224 = CARTESIAN_POINT ( 'NONE',  ( -8.715434833791929847, 115.0601862821014549, -8.962234695871762469 ) ) ;
#25225 = CARTESIAN_POINT ( 'NONE',  ( 22.56230152254410370, 7.347880794884117764E-16, -0.5624999987710044280 ) ) ;
#25226 = CARTESIAN_POINT ( 'NONE',  ( -45.84747103062156981, 213.3500491399821328, -5.571401726697985168 ) ) ;
#25227 = CARTESIAN_POINT ( 'NONE',  ( 15.00000000000053468, -3.464101615138063472, -5.362499999999978506 ) ) ;
#25228 = CARTESIAN_POINT ( 'NONE',  ( 18.00000000000000355, 244.6750000000000114, 5.196152422706632912 ) ) ;
#25229 = CARTESIAN_POINT ( 'NONE',  ( -5.770363421893818234, 115.6351862821014436, -14.38691631536207005 ) ) ;
#25230 = CIRCLE ( 'NONE', #8888, 28.99999999999999645 ) ;
#25231 = CARTESIAN_POINT ( 'NONE',  ( 25.36386068845838082, 0.000000000000000000, 168.7214353850716293 ) ) ;
#25232 = CARTESIAN_POINT ( 'NONE',  ( -4.944772684328673229, 20.18518628210144783, 11.48171059495397728 ) ) ;
#25233 = CARTESIAN_POINT ( 'NONE',  ( 16.56230152254411081, 6.928203230275514990, -8.662500000000004974 ) ) ;
#25234 = ORIENTED_EDGE ( 'NONE', *, *, #1109, .T. ) ;
#25235 = CARTESIAN_POINT ( 'NONE',  ( 13.56230152254411969, -5.196152422706638241, -3.525000000000083844 ) ) ;
#25236 = CARTESIAN_POINT ( 'NONE',  ( 2.064181346179272847, 88.89768628210146062, -9.465287035748065847 ) ) ;
#25237 = CARTESIAN_POINT ( 'NONE',  ( 5.778771075727756162E-15, 194.9656250006145228, 31.45816453501075927 ) ) ;
#25238 = CARTESIAN_POINT ( 'NONE',  ( 26.99999999999999645, 7.347880794884117764E-16, -2.925000000000010925 ) ) ;
#25239 = CARTESIAN_POINT ( 'NONE',  ( -27.24356964374999990, 198.9218750006145626, -15.72908226750537786 ) ) ;
#25240 = ADVANCED_FACE ( 'NONE', ( #32142 ), #29296, .F. ) ;
#25241 = CARTESIAN_POINT ( 'NONE',  ( 26.60793733450167053, 1.299049382686714882, -8.000000000000000000 ) ) ;
#25242 = CARTESIAN_POINT ( 'NONE',  ( 24.66770419336863185, 0.000000000000000000, 160.7643302352881278 ) ) ;
#25243 = CARTESIAN_POINT ( 'NONE',  ( -6.594114490232462877, 51.33981371789855785, 6.840914352311949109 ) ) ;
#25244 = CARTESIAN_POINT ( 'NONE',  ( 15.00000000000000000, 3.464101615137752166, -9.487500000000004263 ) ) ;
#25245 = ORIENTED_EDGE ( 'NONE', *, *, #534, .T. ) ;
#25246 = AXIS2_PLACEMENT_3D ( 'NONE', #19420, #16197, #33063 ) ;
#25247 = CARTESIAN_POINT ( 'NONE',  ( 26.99999999999999645, 240.8687500012290457, -3.464101615137755275 ) ) ;
#25248 = CARTESIAN_POINT ( 'NONE',  ( -4.622313124798826500, 69.16481371789855359, 11.61527771782809637 ) ) ;
#25249 = CARTESIAN_POINT ( 'NONE',  ( 22.80587116629412847, -3.604726614523238837, -5.409374999385520688 ) ) ;
#25250 = CARTESIAN_POINT ( 'NONE',  ( 13.62178482187501416, 198.6031250006145399, 23.59362340125806767 ) ) ;
#25251 = CARTESIAN_POINT ( 'NONE',  ( 15.24356964374999990, 3.323476615752268604, -6.590624999385473970 ) ) ;
#25252 = CARTESIAN_POINT ( 'NONE',  ( -4.944772684328424539, 26.61481371789854578, -11.48171059495408031 ) ) ;
#25253 = EDGE_CURVE ( 'NONE', #23933, #26829, #23796, .T. ) ;
#25254 = EDGE_LOOP ( 'NONE', ( #29031, #22600, #23481, #6547 ) ) ;
#25255 = UNCERTAINTY_MEASURE_WITH_UNIT (LENGTH_MEASURE( 1.000000000000000082E-05 ), #1171, 'distance_accuracy_value', 'NONE');
#25256 = CARTESIAN_POINT ( 'NONE',  ( 19.68408634441911431, 5.407089921784862696, -0.3468749993855158031 ) ) ;
#25257 = AXIS2_PLACEMENT_3D ( 'NONE', #30063, #4098, #15669 ) ;
#25258 = DIRECTION ( 'NONE',  ( 0.000000000000000000, 1.000000000000000000, 0.000000000000000000 ) ) ;
#25259 = CARTESIAN_POINT ( 'NONE',  ( 37.64173127707041289, 7.646167579472024665E-16, 168.5789311836665831 ) ) ;
#25260 = CARTESIAN_POINT ( 'NONE',  ( -41.48586230271182984, 206.8500491399821328, 5.686928522499748340 ) ) ;
#25261 = CYLINDRICAL_SURFACE ( 'NONE', #12543, 5.999999999999999112 ) ;
#25262 = CARTESIAN_POINT ( 'NONE',  ( -7.228626920338836470, 72.32731371789854791, -10.49813415416005213 ) ) ;
#25263 = CARTESIAN_POINT ( 'NONE',  ( -37.73288769728823411, 205.5309553116392465, -1.321298161741839117 ) ) ;
#25264 = CARTESIAN_POINT ( 'NONE',  ( -40.50372103062156981, 216.5309553116391612, -1.626142955000564383 ) ) ;
#25265 = CARTESIAN_POINT ( 'NONE',  ( 15.00000000000000000, 0.000000000000000000, -3.543749998770939769 ) ) ;
#25266 = DIRECTION ( 'NONE',  ( 6.123233995736766036E-17, -1.000000000000000000, 0.000000000000000000 ) ) ;
#25267 = CARTESIAN_POINT ( 'NONE',  ( 15.50000000000000533, 38.68981371789855217, -0.1745138560722452326 ) ) ;
#25268 = CARTESIAN_POINT ( 'NONE',  ( -67.81622103062157692, 212.1620413398628671, 8.530955311639223382 ) ) ;
#25269 = PRODUCT_DEFINITION_SHAPE ( 'NONE', 'NONE',  #33139 ) ;
#25270 = CARTESIAN_POINT ( 'NONE',  ( -2.660918448318275509, 19.89768628210143575, 12.46528703574805874 ) ) ;
#25271 = CARTESIAN_POINT ( 'NONE',  ( -2.311890736173176641, 60.72268628210144925, -12.53471296425194836 ) ) ;
#25272 = CARTESIAN_POINT ( 'NONE',  ( 11.08355503943142750, 6.960186282101432198, -10.83675517735155225 ) ) ;
#25273 = CARTESIAN_POINT ( 'NONE',  ( 13.56230152254410726, 5.196152422706636465, -1.425000000000037348 ) ) ;
#25274 = CARTESIAN_POINT ( 'NONE',  ( 13.50000000000001421, 198.9125000012290343, 23.38268590217984055 ) ) ;
#25275 = EDGE_LOOP ( 'NONE', ( #20512, #5851, #27445, #10038 ) ) ;
#25276 = CARTESIAN_POINT ( 'NONE',  ( 14.25334919248782661, 36.28518628210144215, 6.092822981423971385 ) ) ;
#25277 = CARTESIAN_POINT ( 'NONE',  ( 15.00000000000000355, 7.347880794884112834E-16, -8.000000000000000000 ) ) ;
#25278 = CARTESIAN_POINT ( 'NONE',  ( -13.62178482187498396, 199.0343750006145456, 23.59362340125808188 ) ) ;
#25279 = FACE_OUTER_BOUND ( 'NONE', #21894, .T. ) ;
#25280 =( LENGTH_UNIT ( ) NAMED_UNIT ( * ) SI_UNIT ( .MILLI., .METRE. ) );
#25281 = FACE_OUTER_BOUND ( 'NONE', #1150, .T. ) ;
#25282 = CARTESIAN_POINT ( 'NONE',  ( -10.69584247140444866, 11.84768628210144925, 6.932735513423972762 ) ) ;
#25283 = CARTESIAN_POINT ( 'NONE',  ( 21.00000000000000000, 247.2718750006145569, 6.646953231504538984 ) ) ;
#25284 = CARTESIAN_POINT ( 'NONE',  ( 6.594114490232462877, 111.1398137178985621, -6.840914352311949109 ) ) ;
#25285 = CARTESIAN_POINT ( 'NONE',  ( 23.87821517812500005, 242.3593750006145342, 4.985214923628404016 ) ) ;
#25286 = VERTEX_POINT ( 'NONE', #23812 ) ;
#25287 = CARTESIAN_POINT ( 'NONE',  ( -68.40997103062156270, 215.5714017266979852, 3.350049139982118618 ) ) ;
#25288 = CARTESIAN_POINT ( 'NONE',  ( 15.00000000000000000, 247.7687500012291082, -3.464101615137752166 ) ) ;
#25289 = CARTESIAN_POINT ( 'NONE',  ( 11.61527771782809637, 112.8648137178985564, 4.622313124798827388 ) ) ;
#25290 = CARTESIAN_POINT ( 'NONE',  ( 10.31873187879410914, 0.000000000000000000, -9.590624999385537919 ) ) ;
#25291 = CARTESIAN_POINT ( 'NONE',  ( 30.73066631613276556, 7.209453229046475009, 161.2220249341241072 ) ) ;
#25292 = DIRECTION ( 'NONE',  ( -1.045431693899523221E-14, -0.1163425707149444432, 0.9932091452657080266 ) ) ;
#25293 = CARTESIAN_POINT ( 'NONE',  ( -27.24356964374999635, 198.9968750006145228, 15.72908226750539384 ) ) ;
#25294 = ORIENTED_EDGE ( 'NONE', *, *, #20289, .T. ) ;
#25295 = VERTEX_POINT ( 'NONE', #12623 ) ;
#25296 = VERTEX_POINT ( 'NONE', #3710 ) ;
#25297 = CARTESIAN_POINT ( 'NONE',  ( 15.00000000000000000, 3.464101615137752166, -4.481249998770945098 ) ) ;
#25298 = CARTESIAN_POINT ( 'NONE',  ( 20.99999999999999645, 6.646953231504538984, -2.503124999385450966 ) ) ;
#25299 = DIRECTION ( 'NONE',  ( 0.000000000000000000, 0.000000000000000000, 1.000000000000000000 ) ) ;
#25300 = CARTESIAN_POINT ( 'NONE',  ( 26.97716818855048260, 0.000000000000000000, 49.47706554351410801 ) ) ;
#25301 = CARTESIAN_POINT ( 'NONE',  ( 26.75643035624999655, 249.5218750006145001, -7.049594010296217766E-16 ) ) ;
#25302 = CARTESIAN_POINT ( 'NONE',  ( -10.69584247140444866, 67.04768628210145209, 6.932735513423972762 ) ) ;
#25303 = CARTESIAN_POINT ( 'NONE',  ( -66.42336230271182274, 215.6869285224997270, 3.149950860017831200 ) ) ;
#25304 = CARTESIAN_POINT ( 'NONE',  ( 14.99999999999999822, 225.9999999999999716, 0.1963495407219037481 ) ) ;
#25305 = CARTESIAN_POINT ( 'NONE',  ( -43.86086230271183695, 212.1499508600178387, -3.954877714930852495 ) ) ;
#25306 = FACE_OUTER_BOUND ( 'NONE', #14848, .T. ) ;
#25307 = CARTESIAN_POINT ( 'NONE',  ( 28.12039261777511356, 5.196152422706630247, 165.8075997743837604 ) ) ;
#25308 = CARTESIAN_POINT ( 'NONE',  ( -12.50000000000000355, 116.8898137178985621, 0.1745138560722786503 ) ) ;
#25309 = CARTESIAN_POINT ( 'NONE',  ( -67.42038769728826253, 208.6787018382581778, 4.469044688360752637 ) ) ;
#25310 = CARTESIAN_POINT ( 'NONE',  ( -54.35788769728822700, 218.4690446883607535, 2.393094931466250408 ) ) ;
#25311 = CARTESIAN_POINT ( 'NONE',  ( 18.12178482187500350, -4.985214923628407568, -1.078124999385476901 ) ) ;
#25312 = CARTESIAN_POINT ( 'NONE',  ( 27.24356964374999635, 195.5656250006145171, -15.72908226750539029 ) ) ;
#25313 = AXIS2_PLACEMENT_3D ( 'NONE', #12475, #4446, #36278 ) ;
#25314 = CARTESIAN_POINT ( 'NONE',  ( 6.092822981423662299, 86.41481371789855359, 14.25334919248795096 ) ) ;
#25315 = CARTESIAN_POINT ( 'NONE',  ( -33.76711230271183695, 216.4690446883607535, -1.857196546604089393 ) ) ;
#25316 = ORIENTED_EDGE ( 'NONE', *, *, #17995, .T. ) ;
#25317 =( BOUNDED_CURVE ( )  B_SPLINE_CURVE ( 2, ( #19890, #34459, #23281, #8500, #20068, #17410, #25929, #31613, #37473 ),
 .UNSPECIFIED., .F., .F. ) 
 B_SPLINE_CURVE_WITH_KNOTS ( ( 3, 2, 2, 2, 3 ),
 ( 0.4791666666666666852, 0.4861111111111111049, 0.5000000000000000000, 0.5138888888888888395, 0.5208333333333333703 ),
 .UNSPECIFIED. ) 
 CURVE ( )  GEOMETRIC_REPRESENTATION_ITEM ( )  RATIONAL_B_SPLINE_CURVE ( ( 0.9330127018922194093, 0.9330127018922196314, 1.000000000000000000, 0.8660254037844387076, 1.000000000000000000, 0.8660254037844387076, 1.000000000000000000, 0.9330127018922187432, 0.9330127018922192983 ) ) 
 REPRESENTATION_ITEM ( '' )  );
#25318 = CARTESIAN_POINT ( 'NONE',  ( 20.99999999999999645, -6.928203230275506996, -6.637499999999977085 ) ) ;
#25319 = CARTESIAN_POINT ( 'NONE',  ( -2.660918448318275509, 121.0976862821014635, 12.46528703574805874 ) ) ;
#25320 = EDGE_CURVE ( 'NONE', #21615, #33833, #15280, .T. ) ;
#25321 = CARTESIAN_POINT ( 'NONE',  ( 8.927990412390657937, 71.07268628210144357, -13.04141134922759804 ) ) ;
#25322 = PLANE ( 'NONE',  #26511 ) ;
#25323 = CARTESIAN_POINT ( 'NONE',  ( 31.01991443737654564, -7.209453229046482114, 164.5281460884161220 ) ) ;
#25324 = CARTESIAN_POINT ( 'NONE',  ( 8.632099005475504683, 83.14768628210143220, 13.23911966647218996 ) ) ;
#25325 = CARTESIAN_POINT ( 'NONE',  ( -41.09747103062156981, 213.3500491399821328, -5.571401726697985168 ) ) ;
#25326 = CARTESIAN_POINT ( 'NONE',  ( 10.31873187879410914, 0.000000000000000000, -5.990624999385518734 ) ) ;
#25327 = CARTESIAN_POINT ( 'NONE',  ( -9.500000000000005329, 21.91018628210143859, -0.1745138560725176813 ) ) ;
#25328 = CARTESIAN_POINT ( 'NONE',  ( 36.68087069682425039, 7.347880794884117764E-16, 160.3908927435282692 ) ) ;
#25329 = CARTESIAN_POINT ( 'NONE',  ( -67.81622103062156270, 211.6261429550005744, 6.530955311639227823 ) ) ;
#25330 = DIRECTION ( 'NONE',  ( -0.9925324990730152175, 0.1219804832088933616, 0.000000000000000000 ) ) ;
#25331 = CARTESIAN_POINT ( 'NONE',  ( -8.715434833791929847, 59.86018628210145209, -8.962234695871762469 ) ) ;
#25332 = CARTESIAN_POINT ( 'NONE',  ( 13.50000000000001421, 197.4500000000000171, 23.38268590217984055 ) ) ;
#25333 = AXIS2_PLACEMENT_3D ( 'NONE', #20495, #5881, #32034 ) ;
#25334 = LINE ( 'NONE', #22315, #23846 ) ;
#25336 = CARTESIAN_POINT ( 'NONE',  ( 19.56230152254411792, 5.196152422706637353, -1.950000000000035039 ) ) ;
#25335 = CARTESIAN_POINT ( 'NONE',  ( -3.474262827703337830, 32.83518628210143930, -8.843639120294326972 ) ) ;
#25337 = CARTESIAN_POINT ( 'NONE',  ( 15.24356964374999990, 249.8218750006145399, -3.323476615752268604 ) ) ;
#25338 = VERTEX_POINT ( 'NONE', #18321 ) ;
#25339 = CARTESIAN_POINT ( 'NONE',  ( 24.00000000000000000, -5.196152422706629359, -3.450000000000008615 ) ) ;
#25340 = CARTESIAN_POINT ( 'NONE',  ( 26.77152063323770292, 0.3446893914122488023, -7.999999999999996447 ) ) ;
#25341 = CARTESIAN_POINT ( 'NONE',  ( 24.51248951003896437, 3.604726614523240613, 161.7848665344110657 ) ) ;
#25342 = CARTESIAN_POINT ( 'NONE',  ( 22.80587116629410716, -3.604726614523235284, -2.203124999385539962 ) ) ;
#25343 = CARTESIAN_POINT ( 'NONE',  ( 24.65789917220240213, 0.000000000000000000, 160.6522583305284968 ) ) ;
#25344 = CARTESIAN_POINT ( 'NONE',  ( 26.99999999999999645, 244.4124999999999943, -3.464101615137755275 ) ) ;
#25345 = CARTESIAN_POINT ( 'NONE',  ( 13.56230152254410548, 5.196152422706630247, -4.012499998771012599 ) ) ;
#25346 = EDGE_CURVE ( 'NONE', #7130, #30424, #11940, .T. ) ;
#25347 =( BOUNDED_CURVE ( )  B_SPLINE_CURVE ( 2, ( #8047, #28313, #19623, #5192, #10506 ),
 .UNSPECIFIED., .F., .F. ) 
 B_SPLINE_CURVE_WITH_KNOTS ( ( 3, 2, 3 ),
 ( 0.000000000000000000, 0.01388888888888888985, 0.02083333333333333565 ),
 .UNSPECIFIED. ) 
 CURVE ( )  GEOMETRIC_REPRESENTATION_ITEM ( )  RATIONAL_B_SPLINE_CURVE ( ( 1.000000000000000000, 0.8660254037844387076, 1.000000000000000000, 0.9330127018922192983, 0.9330127018922194093 ) ) 
 REPRESENTATION_ITEM ( '' )  );
#25348 = CARTESIAN_POINT ( 'NONE',  ( 2.660918448318279950, 79.69768628210144357, -12.46528703574805874 ) ) ;
#25349 = VERTEX_POINT ( 'NONE', #24187 ) ;
#25350 = ORIENTED_EDGE ( 'NONE', *, *, #29030, .F. ) ;
#25351 = CARTESIAN_POINT ( 'NONE',  ( 27.00000000000000355, 195.3875000012290286, -3.306546357697854128E-15 ) ) ;
#25352 = CARTESIAN_POINT ( 'NONE',  ( -10.83675517735179028, 51.33981371789855785, 11.08355503943118947 ) ) ;
#25353 = CARTESIAN_POINT ( 'NONE',  ( 26.75643035624999655, -3.323476615752267715, -9.965624999385457983 ) ) ;
#25354 = EDGE_CURVE ( 'NONE', #29149, #31332, #15830, .T. ) ;
#25355 = CARTESIAN_POINT ( 'NONE',  ( 15.24356964375000167, 243.5968750006144887, 3.323476615752272600 ) ) ;
#25356 = CARTESIAN_POINT ( 'NONE',  ( -41.09747103062157692, 212.3500491399821613, -3.839350919129076445 ) ) ;
#25357 = CARTESIAN_POINT ( 'NONE',  ( 20.00041209925370467, 239.8223985277589918, -5.668978256696592055 ) ) ;
#25358 = CARTESIAN_POINT ( 'NONE',  ( 5.233372021372610483, 46.45231371789854791, -8.152565276336593669 ) ) ;
#25359 = CARTESIAN_POINT ( 'NONE',  ( 22.80587116629410716, 7.646167579472015790E-16, -9.815624999385569538 ) ) ;
#25360 = CARTESIAN_POINT ( 'NONE',  ( -1.715153634034442431, 96.47731371789852517, 9.534712964251900402 ) ) ;
#25361 = CARTESIAN_POINT ( 'NONE',  ( 27.24356964374999635, 198.3218750006145399, -15.72908226750539029 ) ) ;
#25362 = CARTESIAN_POINT ( 'NONE',  ( -12.50000000000000355, 6.489813717898557321, 0.1745138560722786503 ) ) ;
#25363 = CARTESIAN_POINT ( 'NONE',  ( -8.962234695871760692, 66.76018628210145778, 8.715434833791933400 ) ) ;
#25364 = DIRECTION ( 'NONE',  ( -0.000000000000000000, -1.000000000000000000, -0.000000000000000000 ) ) ;
#25365 = CARTESIAN_POINT ( 'NONE',  ( -47.00000000000000711, 244.5000000000000000, 5.000000000000000000 ) ) ;
#25366 = CARTESIAN_POINT ( 'NONE',  ( 24.51739202056851852, 3.604726614523236616, 161.8409024861786918 ) ) ;
#25367 = CARTESIAN_POINT ( 'NONE',  ( 10.31873187879410381, 0.000000000000000000, -9.646874999385518734 ) ) ;
#25368 = CARTESIAN_POINT ( 'NONE',  ( 22.80587116629412847, 3.604726614523243278, -6.234374999385518201 ) ) ;
#25369 = PLANE ( 'NONE',  #10066 ) ;
#25370 = CARTESIAN_POINT ( 'NONE',  ( 33.69882328325508070, 5.196152422706631135, 160.7270745741280962 ) ) ;
#25371 = CARTESIAN_POINT ( 'NONE',  ( -1.715153634034234598, 69.92268628210143788, -9.534712964251941258 ) ) ;
#25372 = CARTESIAN_POINT ( 'NONE',  ( 2.999999999999997335, 244.5000000000000000, -5.000000000000001776 ) ) ;
#25373 = CARTESIAN_POINT ( 'NONE',  ( -2.311890736173176641, 106.7226862821014635, -12.53471296425194836 ) ) ;
#25374 = CARTESIAN_POINT ( 'NONE',  ( 1.069080835302379631E-14, 199.6625000000000227, 27.00000000000000000 ) ) ;
#25375 = LINE ( 'NONE', #16860, #9538 ) ;
#25376 = VERTEX_POINT ( 'NONE', #7133 ) ;
#25377 = CARTESIAN_POINT ( 'NONE',  ( 27.75476278247212747, -5.407089921784859143, 163.0257557572890335 ) ) ;
#25378 = CARTESIAN_POINT ( 'NONE',  ( 26.75643035624999655, 7.049594010296217766E-16, -4.865624999385476102 ) ) ;
#25380 = EDGE_CURVE ( 'NONE', #11014, #28686, #8818, .T. ) ;
#25379 = CARTESIAN_POINT ( 'NONE',  ( 5.778771075727756162E-15, 196.8218750006145683, 31.45816453501076637 ) ) ;
#25381 = CARTESIAN_POINT ( 'NONE',  ( 28.08976766865841057, 5.407089921784862696, 166.8548791280792045 ) ) ;
#25382 = CARTESIAN_POINT ( 'NONE',  ( 37.22014685496823461, 7.347880794884125653E-16, 166.5548474367465985 ) ) ;
#25383 = LINE ( 'NONE', #10603, #20482 ) ;
#25384 = CARTESIAN_POINT ( 'NONE',  ( 15.24356964374999990, 240.3718750006145228, -3.323476615752268604 ) ) ;
#25385 = DIRECTION ( 'NONE',  ( 0.000000000000000000, -1.000000000000000000, 0.000000000000000000 ) ) ;
#25386 = CARTESIAN_POINT ( 'NONE',  ( 12.50000000000000355, 139.8898137178985621, -0.1745138560722771515 ) ) ;
#25387 = CARTESIAN_POINT ( 'NONE',  ( -4.622313124798576922, 134.0351862821014493, -11.61527771782819762 ) ) ;
#25389 = ORIENTED_EDGE ( 'NONE', *, *, #4615, .F. ) ;
#25388 = ORIENTED_EDGE ( 'NONE', *, *, #20852, .T. ) ;
#25390 = CARTESIAN_POINT ( 'NONE',  ( 15.24356964375000167, 245.7343750006145058, 3.323476615752272600 ) ) ;
#25391 = EDGE_CURVE ( 'NONE', #9546, #24650, #2974, .T. ) ;
#25392 = CARTESIAN_POINT ( 'NONE',  ( 12.46528703574811558, 10.80231371789855466, -2.660918448318005947 ) ) ;
#25393 = CARTESIAN_POINT ( 'NONE',  ( 26.75643035624999655, 3.323476615752271712, -4.828124999385488003 ) ) ;
#25394 = CARTESIAN_POINT ( 'NONE',  ( 2.908627838312458636, 119.4773137178985678, -15.53471296425188442 ) ) ;
#25395 = CARTESIAN_POINT ( 'NONE',  ( 16.56230152254411436, -6.928203230275514990, -9.787500000000042277 ) ) ;
#25396 = CARTESIAN_POINT ( 'NONE',  ( 26.75643035624999655, 3.323476615752271712, -0.8906249993854854496 ) ) ;
#25397 = CARTESIAN_POINT ( 'NONE',  ( 10.31873187879410203, -3.604726614523244610, -7.809374999385487293 ) ) ;
#25398 = CARTESIAN_POINT ( 'NONE',  ( -27.00000000000000355, 197.8250000012290286, -15.58845726811989429 ) ) ;
#25399 = CARTESIAN_POINT ( 'NONE',  ( -8.715434833791929847, 105.8601862821014521, -8.962234695871762469 ) ) ;
#25400 = CARTESIAN_POINT ( 'NONE',  ( 10.31873187879411269, 3.604726614523236616, -3.778124999385508609 ) ) ;
#25401 = EDGE_CURVE ( 'NONE', #1340, #25502, #26436, .T. ) ;
#25402 = CARTESIAN_POINT ( 'NONE',  ( -43.66294563604516554, 216.1378603801729241, -6.307003348498026796 ) ) ;
#25403 = CARTESIAN_POINT ( 'NONE',  ( 26.75643035624999655, 244.6093750006145342, -3.323476615752271268 ) ) ;
#25404 = CARTESIAN_POINT ( 'NONE',  ( 22.60769515458672885, 240.4174038105676630, -5.999999999999998224 ) ) ;
#25405 = CARTESIAN_POINT ( 'NONE',  ( -31.59002896937850124, 206.1606490808709111, 2.350049139982143931 ) ) ;
#25406 = CARTESIAN_POINT ( 'NONE',  ( 11.48171059495397728, 128.2851862821014493, 4.944772684328674117 ) ) ;
#25407 = CARTESIAN_POINT ( 'NONE',  ( 22.56230152254410370, 3.464101615137755275, -0.9749999987710199489 ) ) ;
#25408 = CARTESIAN_POINT ( 'NONE',  ( -40.70163769728823411, 215.6869285224996986, -3.149950860017881382 ) ) ;
#25409 = FACE_OUTER_BOUND ( 'NONE', #6744, .T. ) ;
#25410 = CARTESIAN_POINT ( 'NONE',  ( -7.234628195640307347, 199.4575961894323370, -27.00000000000000711 ) ) ;
#25411 = CARTESIAN_POINT ( 'NONE',  ( 6.092822981423978490, 116.7851862821014635, -14.25334919248782306 ) ) ;
#25412 = CARTESIAN_POINT ( 'NONE',  ( 10.69584247140445221, 7.247686282101428290, -6.932735513423970097 ) ) ;
#25413 = EDGE_CURVE ( 'NONE', #14298, #30074, #30007, .T. ) ;
#25414 = DIRECTION ( 'NONE',  ( 0.08715574274765150453, 0.000000000000000000, 0.9961946980917461003 ) ) ;
#25415 = CARTESIAN_POINT ( 'NONE',  ( 9.534712964251941258, 136.6226862821014549, -1.715153634034235708 ) ) ;
#25416 = CARTESIAN_POINT ( 'NONE',  ( 22.80587116629410716, 7.646167579472015790E-16, -0.3656249993855553715 ) ) ;
#25417 = CARTESIAN_POINT ( 'NONE',  ( 16.56230152254410726, 0.000000000000000000, -10.00000000000000000 ) ) ;
#25419 = ORIENTED_EDGE ( 'NONE', *, *, #2636, .T. ) ;
#25418 = VECTOR ( 'NONE', #29990, 1000.000000000000114 ) ;
#25420 = DIRECTION ( 'NONE',  ( 0.000000000000000000, 0.000000000000000000, 1.000000000000000000 ) ) ;
#25421 = CARTESIAN_POINT ( 'NONE',  ( 9.500000000000005329, 72.51018628210145778, 0.1745138560725188748 ) ) ;
#25422 = CARTESIAN_POINT ( 'NONE',  ( 10.56230152254411081, 0.000000000000000000, -2.137499998771025034 ) ) ;
#25423 = CARTESIAN_POINT ( 'NONE',  ( -27.24356964374999635, 197.1406250006145058, 15.72908226750539384 ) ) ;
#25424 = CARTESIAN_POINT ( 'NONE',  ( 20.99999999999999289, 242.2937500012290570, -5.999999999999997335 ) ) ;
#25425 = CARTESIAN_POINT ( 'NONE',  ( -13.62178482187500528, 195.7343750006145626, -23.59362340125807123 ) ) ;
#25426 = DIRECTION ( 'NONE',  ( 1.000000000000000000, 0.000000000000000000, 0.000000000000000000 ) ) ;
#25427 = CARTESIAN_POINT ( 'NONE',  ( 22.56230152254421739, 3.464101615137694878, -6.824999998770996612 ) ) ;
#25428 = CARTESIAN_POINT ( 'NONE',  ( 5.529263428287300108, 49.32731371789854791, 7.954856959092309943 ) ) ;
#25429 = CARTESIAN_POINT ( 'NONE',  ( 26.99999999999999645, -3.464101615137751278, -8.362499999999997158 ) ) ;
#25430 = ORIENTED_EDGE ( 'NONE', *, *, #10791, .F. ) ;
#25431 = CARTESIAN_POINT ( 'NONE',  ( 15.00000000000000178, 240.6437500012290513, 3.464101615137757051 ) ) ;
#25432 = AXIS2_PLACEMENT_3D ( 'NONE', #5330, #14245, #11207 ) ;
#25433 = CARTESIAN_POINT ( 'NONE',  ( 8.962234695871567070, 67.43981371789855928, 8.715434833792127023 ) ) ;
#25434 = CARTESIAN_POINT ( 'NONE',  ( 22.80587116629411426, 7.646167579472024665E-16, -6.271874999385529392 ) ) ;
#25435 = CARTESIAN_POINT ( 'NONE',  ( 23.87821517812499650, 4.985214923628404904, -6.253124999385489602 ) ) ;
#25436 = CARTESIAN_POINT ( 'NONE',  ( 4.622313124798831829, 27.76481371789854435, -11.61527771782809282 ) ) ;
#25437 = ORIENTED_EDGE ( 'NONE', *, *, #1321, .T. ) ;
#25438 = CARTESIAN_POINT ( 'NONE',  ( 10.31873187879411091, 3.604726614523240613, -0.6843749993854860714 ) ) ;
#25439 = CARTESIAN_POINT ( 'NONE',  ( 37.52733936471412335, 3.604726614523243278, 167.2714256424211499 ) ) ;
#25440 = AXIS2_PLACEMENT_3D ( 'NONE', #28026, #22170, #27469 ) ;
#25441 = CARTESIAN_POINT ( 'NONE',  ( -44.45461230271182274, 208.1428034533959135, -6.469044688360754414 ) ) ;
#25442 = CARTESIAN_POINT ( 'NONE',  ( 36.64165061258780298, 7.347880794884117764E-16, 159.9426051293869477 ) ) ;
#25443 = DIRECTION ( 'NONE',  ( -0.000000000000000000, 0.000000000000000000, 1.000000000000000000 ) ) ;
#25444 = EDGE_CURVE ( 'NONE', #23659, #8033, #21150, .T. ) ;
#25445 = CARTESIAN_POINT ( 'NONE',  ( -37.13913769728823411, 207.8500491399821613, -3.954877714930864485 ) ) ;
#25446 = CARTESIAN_POINT ( 'NONE',  ( -41.69122103062155560, 208.3738570449993404, -6.530955311639226935 ) ) ;
#25447 = ORIENTED_EDGE ( 'NONE', *, *, #22948, .T. ) ;
#25448 = FACE_OUTER_BOUND ( 'NONE', #813, .T. ) ;
#25449 = CARTESIAN_POINT ( 'NONE',  ( 26.99999999999999645, 7.347880794884117764E-16, -0.6187499987709565996 ) ) ;
#25450 = CARTESIAN_POINT ( 'NONE',  ( -0.1745138560722442889, 36.38981371789855501, -15.50000000000000533 ) ) ;
#25451 = CARTESIAN_POINT ( 'NONE',  ( -38.71502896937850124, 217.3034525342667962, -4.350049139982195001 ) ) ;
#25452 = CARTESIAN_POINT ( 'NONE',  ( 11.61527771782819940, 16.73518628210143788, -4.622313124798573369 ) ) ;
#25453 = EDGE_CURVE ( 'NONE', #4785, #26761, #27395, .T. ) ;
#25454 = CARTESIAN_POINT ( 'NONE',  ( 10.49813415415989581, 73.37268628210144072, 7.228626920339068285 ) ) ;
#25455 = ADVANCED_FACE ( 'NONE', ( #1425 ), #1987, .F. ) ;
#25456 = CARTESIAN_POINT ( 'NONE',  ( -2.908627838312119351, 14.72268628210143859, -15.53471296425195369 ) ) ;
#25457 = CARTESIAN_POINT ( 'NONE',  ( 22.56230152254411436, 3.464101615137759271, -1.987500000000063993 ) ) ;
#25458 = CARTESIAN_POINT ( 'NONE',  ( 20.99999999999998579, 247.9187500012290002, 5.999999999999998224 ) ) ;
#25459 = ORIENTED_EDGE ( 'NONE', *, *, #25453, .F. ) ;
#25460 = CARTESIAN_POINT ( 'NONE',  ( 11.08355503943142750, 6.960186282101432198, -10.83675517735155225 ) ) ;
#25461 = PRODUCT_RELATED_PRODUCT_CATEGORY ( 'part', '', ( #2880 ) ) ;
#25462 = CARTESIAN_POINT ( 'NONE',  ( -20.86978604919638869, 194.8026013911397456, -17.51182792271053046 ) ) ;
#25463 = CARTESIAN_POINT ( 'NONE',  ( -13.62178482187500528, 198.8843750006145399, -23.59362340125807123 ) ) ;
#25464 = CARTESIAN_POINT ( 'NONE',  ( 24.92917142150405496, 3.464101615137512358, 163.7529143283390454 ) ) ;
#25465 = DIRECTION ( 'NONE',  ( -0.000000000000000000, -1.000000000000000000, -0.000000000000000000 ) ) ;
#25466 = CARTESIAN_POINT ( 'NONE',  ( 13.50000000000001421, 195.6500000000000057, 23.38268590217984055 ) ) ;
#25467 = CARTESIAN_POINT ( 'NONE',  ( 6.932735513423970097, 9.547686282101453870, 10.69584247140445044 ) ) ;
#25468 = CARTESIAN_POINT ( 'NONE',  ( 18.12178482187499640, 246.6343750006145115, -4.985214923628404904 ) ) ;
#25469 = CARTESIAN_POINT ( 'NONE',  ( 0.1745138560723095977, 105.3898137178985479, 9.500000000000005329 ) ) ;
#25470 = CARTESIAN_POINT ( 'NONE',  ( 15.24356964374999990, 242.6593750006145171, 0.000000000000000000 ) ) ;
#25471 = VERTEX_POINT ( 'NONE', #30627 ) ;
#25472 = DIRECTION ( 'NONE',  ( 0.9925324990730152175, -0.1219804832088933616, 0.000000000000000000 ) ) ;
#25473 = CARTESIAN_POINT ( 'NONE',  ( 15.00000000000000000, 249.5687500012290343, -3.464101615137752166 ) ) ;
#25474 = CARTESIAN_POINT ( 'NONE',  ( 6.932735513424201024, 110.8523137178985536, -10.69584247140429412 ) ) ;
#25475 = CARTESIAN_POINT ( 'NONE',  ( 13.44051670066911619, -5.407089921784859143, -9.965624999385552130 ) ) ;
#25476 = CARTESIAN_POINT ( 'NONE',  ( 24.63832061363088854, 0.000000000000000000, 163.2231226297810451 ) ) ;
#25477 = CARTESIAN_POINT ( 'NONE',  ( -12.50000000000000355, 143.0000000000000284, -1.353084311261909534E-13 ) ) ;
#25478 = CARTESIAN_POINT ( 'NONE',  ( -27.24356964374999635, 199.4468750006145399, 15.72908226750539384 ) ) ;
#25479 = EDGE_LOOP ( 'NONE', ( #35824, #5500, #4433, #27562 ) ) ;
#25480 = VERTEX_POINT ( 'NONE', #21909 ) ;
#25481 = ORIENTED_EDGE ( 'NONE', *, *, #5298, .T. ) ;
#25482 = CARTESIAN_POINT ( 'NONE',  ( 21.00000000000000000, 6.928203230275506996, -5.906249998770959131 ) ) ;
#25483 = CARTESIAN_POINT ( 'NONE',  ( 15.24356964375000167, -3.323476615752272600, -3.253124999385454519 ) ) ;
#25484 = CARTESIAN_POINT ( 'NONE',  ( 15.00000000000000000, 241.9562500012290513, 0.000000000000000000 ) ) ;
#25485 = DIRECTION ( 'NONE',  ( -1.000000000000000000, -4.130293990420971855E-17, 0.000000000000000000 ) ) ;
#25486 = CARTESIAN_POINT ( 'NONE',  ( 15.24356964374999990, 249.7093750006145285, -3.323476615752268604 ) ) ;
#25487 = CARTESIAN_POINT ( 'NONE',  ( -7.228626920339069173, 66.47268628210144925, 10.49813415415989581 ) ) ;
#25488 = CARTESIAN_POINT ( 'NONE',  ( -62.66294563604517975, 214.6737587650350747, -4.842901733360248429 ) ) ;
#25489 = CARTESIAN_POINT ( 'NONE',  ( 6.418300056333629655, 215.4681374788749793, -2.477503916095892489 ) ) ;
#25490 = CARTESIAN_POINT ( 'NONE',  ( -38.31919563604515844, 214.5000000000000284, -0.1155267958017627827 ) ) ;
#25491 =( NAMED_UNIT ( * ) SI_UNIT ( $, .STERADIAN. ) SOLID_ANGLE_UNIT ( ) );
#25492 =( BOUNDED_CURVE ( )  B_SPLINE_CURVE ( 2, ( #31789, #5825, #8862, #23275, #14368, #34819, #10959 ),
 .UNSPECIFIED., .F., .F. ) 
 B_SPLINE_CURVE_WITH_KNOTS ( ( 3, 2, 2, 3 ),
 ( 0.7608695652173934620, 0.7681159420289876971, 0.7753623188405820432, 0.7826086956521763893 ),
 .UNSPECIFIED. ) 
 CURVE ( )  GEOMETRIC_REPRESENTATION_ITEM ( )  RATIONAL_B_SPLINE_CURVE ( ( 0.9999999999999610312, 0.8660254037844776764, 1.000000000000000000, 0.8660254037844387076, 1.000000000000000000, 0.8660254037843935215, 1.000000000000045075 ) ) 
 REPRESENTATION_ITEM ( '' )  );
#25493 = CARTESIAN_POINT ( 'NONE',  ( 31.06648828746087077, 6.928203230275506996, 165.0604876308210862 ) ) ;
#25494 = CARTESIAN_POINT ( 'NONE',  ( -6.932735513424201912, 115.4523137178985621, 10.69584247140429412 ) ) ;
#25495 = CARTESIAN_POINT ( 'NONE',  ( -34.36830436395490551, 209.8844732041982581, 6.500000000000000888 ) ) ;
#25496 = CARTESIAN_POINT ( 'NONE',  ( -38.52455436395490551, 203.6929966515020283, 6.137860380172978303 ) ) ;
#25497 = CARTESIAN_POINT ( 'NONE',  ( 15.24356964374999990, 0.000000000000000000, -3.853124999385476812 ) ) ;
#25498 = VECTOR ( 'NONE', #9099, 1000.000000000000227 ) ;
#25499 = CARTESIAN_POINT ( 'NONE',  ( -1.926257025242585782E-15, 195.1906250006145456, -31.45816453501075927 ) ) ;
#25500 = CARTESIAN_POINT ( 'NONE',  ( 11.08355503943118769, 85.83981371789856496, 10.83675517735179028 ) ) ;
#25501 = CARTESIAN_POINT ( 'NONE',  ( -37.32961230271182274, 211.8571965466040297, 6.469044688360755302 ) ) ;
#25502 = VERTEX_POINT ( 'NONE', #33458 ) ;
#25503 = CARTESIAN_POINT ( 'NONE',  ( 26.99999999999999645, 7.347880794884117764E-16, -6.525000000000003020 ) ) ;
#25504 = CARTESIAN_POINT ( 'NONE',  ( -0.1745138560725500443, 120.8101862821014691, 12.50000000000000355 ) ) ;
#25505 = CARTESIAN_POINT ( 'NONE',  ( -0.1745138560725817967, 56.41018628210145636, 15.50000000000000533 ) ) ;
#25506 = CARTESIAN_POINT ( 'NONE',  ( 31.10570837169731107, 6.928203230275506996, 165.5087752449623224 ) ) ;
#25507 = CARTESIAN_POINT ( 'NONE',  ( 24.67590652769081316, -3.604726614523244610, 163.6527315933331295 ) ) ;
#25508 = CARTESIAN_POINT ( 'NONE',  ( 3.257655550457285720, 79.69768628210141515, -15.46528703574804986 ) ) ;
#25509 = CARTESIAN_POINT ( 'NONE',  ( 16.56230152254411081, 7.209453229046475009, -5.653124999385517491 ) ) ;
#25510 = CARTESIAN_POINT ( 'NONE',  ( -8.843639120294326972, 21.33518628210144641, 3.474262827703335166 ) ) ;
#25511 = DIRECTION ( 'NONE',  ( 0.000000000000000000, 0.000000000000000000, 1.000000000000000000 ) ) ;
#25512 = CARTESIAN_POINT ( 'NONE',  ( -59.89955436395490551, 214.8429017333601792, -4.673758765035196383 ) ) ;
#25513 = LINE ( 'NONE', #37066, #24489 ) ;
#25514 = CARTESIAN_POINT ( 'NONE',  ( 12.53471296425194836, 63.02268628210145351, -2.311890736173178418 ) ) ;
#25515 = CARTESIAN_POINT ( 'NONE',  ( 27.00000000000001066, 197.0374999999999943, 15.58845726811988897 ) ) ;
#25516 = CARTESIAN_POINT ( 'NONE',  ( -60.72871937935236986, 215.3268752544371978, -7.500000000000000888 ) ) ;
#25518 = CARTESIAN_POINT ( 'NONE',  ( 10.31873187879410914, 0.000000000000000000, -2.446874999385534544 ) ) ;
#25517 = CARTESIAN_POINT ( 'NONE',  ( -3.474262827703337830, 23.63518628210144357, -8.843639120294326972 ) ) ;
#25519 = CARTESIAN_POINT ( 'NONE',  ( 15.24356964374999990, 249.4093750006145171, 0.000000000000000000 ) ) ;
#25520 = ORIENTED_EDGE ( 'NONE', *, *, #8449, .F. ) ;
#25521 = CARTESIAN_POINT ( 'NONE',  ( 18.00000000000000355, -5.196152422706632912, -4.874999999999990230 ) ) ;
#25522 = CARTESIAN_POINT ( 'NONE',  ( 28.03214742813599969, 5.196152422706636465, 164.7989526413415149 ) ) ;
#25523 = CIRCLE ( 'NONE', #12809, 7.500000000000000000 ) ;
#25524 = CARTESIAN_POINT ( 'NONE',  ( 30.74537384772143866, -7.209453229046482114, 161.3901327894271276 ) ) ;
#25525 = CARTESIAN_POINT ( 'NONE',  ( 22.80587116629411071, -3.604726614523235284, -2.653124999385503724 ) ) ;
#25526 = CARTESIAN_POINT ( 'NONE',  ( 31.39740774815230751, 7.209453229046475009, 168.8429143745260035 ) ) ;
#25527 = CARTESIAN_POINT ( 'NONE',  ( 21.00000000000000000, 243.1374999999999886, -6.928203230275506996 ) ) ;
#25528 = LINE ( 'NONE', #34248, #28162 ) ;
#25529 = CARTESIAN_POINT ( 'NONE',  ( 7.228626920339069173, 71.07268628210144357, -10.49813415415989404 ) ) ;
#25530 = VERTEX_POINT ( 'NONE', #7499 ) ;
#25531 = VERTEX_POINT ( 'NONE', #19075 ) ;
#25532 = AXIS2_PLACEMENT_3D ( 'NONE', #24403, #9990, #4301 ) ;
#25533 = CARTESIAN_POINT ( 'NONE',  ( -27.00000000000000355, 195.1250000012290400, -15.58845726811989429 ) ) ;
#25534 = CYLINDRICAL_SURFACE ( 'NONE', #5341, 6.000000000000001776 ) ;
#25535 = CARTESIAN_POINT ( 'NONE',  ( 5.770363421894130873, 36.96481371789853654, -14.38691631536193860 ) ) ;
#25536 = CARTESIAN_POINT ( 'NONE',  ( 18.12178482187499640, 4.985214923628404904, -8.428124999385472549 ) ) ;
#25537 = CARTESIAN_POINT ( 'NONE',  ( 21.00000000000000000, 241.8718750006145228, 6.646953231504538984 ) ) ;
#25538 = CARTESIAN_POINT ( 'NONE',  ( -48.81622103062156981, 211.0902445701382533, 4.530955311639240257 ) ) ;
#25539 = CARTESIAN_POINT ( 'NONE',  ( -26.99999999999999645, 199.5875000000000341, 15.58845726811991561 ) ) ;
#25540 = CARTESIAN_POINT ( 'NONE',  ( 33.89776776044609363, -5.407089921784861808, 161.6036962298979915 ) ) ;
#25541 = CARTESIAN_POINT ( 'NONE',  ( 2.064181346179061460, 40.70231371789854791, 9.465287035748106703 ) ) ;
#25542 = CARTESIAN_POINT ( 'NONE',  ( 16.56230152254411081, -7.209453229046475009, -9.028124999385502392 ) ) ;
#25543 =( BOUNDED_CURVE ( )  B_SPLINE_CURVE ( 2, ( #7571, #2059, #33529, #19146, #4713, #33347, #16107 ),
 .UNSPECIFIED., .F., .F. ) 
 B_SPLINE_CURVE_WITH_KNOTS ( ( 3, 2, 2, 3 ),
 ( 0.6304347826086944551, 0.6376811594202886901, 0.6449275362318830362, 0.6521739130434773823 ),
 .UNSPECIFIED. ) 
 CURVE ( )  GEOMETRIC_REPRESENTATION_ITEM ( )  RATIONAL_B_SPLINE_CURVE ( ( 1.000000000000022649, 0.8660254037844161701, 1.000000000000000000, 0.8660254037844387076, 1.000000000000000000, 0.8660254037844551389, 0.9999999999999835687 ) ) 
 REPRESENTATION_ITEM ( '' )  );
#25544 = CARTESIAN_POINT ( 'NONE',  ( -5.529263428287297444, 90.72731371789855359, -7.954856959092311719 ) ) ;
#25545 = CARTESIAN_POINT ( 'NONE',  ( -27.24356964374999635, 198.5468750006145626, 15.72908226750539384 ) ) ;
#25546 = CARTESIAN_POINT ( 'NONE',  ( 2.311890736173452865, 18.27731371789853299, -12.53471296425189152 ) ) ;
#25547 = AXIS2_PLACEMENT_3D ( 'NONE', #10224, #33351, #18780 ) ;
#25548 = CARTESIAN_POINT ( 'NONE',  ( -12.46528703574805697, 68.19768628210144357, -2.660918448318280838 ) ) ;
#25549 = CARTESIAN_POINT ( 'NONE',  ( 1.069080835302379631E-14, 198.7624999999999886, 27.00000000000000000 ) ) ;
#25550 = DIRECTION ( 'NONE',  ( -1.045431693899523221E-14, -0.1163425707149444432, 0.9932091452657080266 ) ) ;
#25551 = CARTESIAN_POINT ( 'NONE',  ( 25.21845102629493951, 3.604726614523240613, 169.8540435889542550 ) ) ;
#25552 = CARTESIAN_POINT ( 'NONE',  ( 13.44051670066911441, -5.407089921784865361, -9.571874999385554972 ) ) ;
#25553 = CARTESIAN_POINT ( 'NONE',  ( 19.68408634441911786, -5.407089921784861808, -9.046874999385529748 ) ) ;
#25554 = CARTESIAN_POINT ( 'NONE',  ( 13.49999999999999645, 197.2625000012290286, -23.38268590217984766 ) ) ;
#25555 = CARTESIAN_POINT ( 'NONE',  ( 6.594114490232313663, 73.66018628210144925, 6.840914352312096547 ) ) ;
#25556 = CARTESIAN_POINT ( 'NONE',  ( 0.000000000000000000, 141.0000000000000000, 0.000000000000000000 ) ) ;
#25557 =( BOUNDED_CURVE ( )  B_SPLINE_CURVE ( 2, ( #19411, #16189, #19043, #25077, #7464, #27740, #24894 ),
 .UNSPECIFIED., .F., .F. ) 
 B_SPLINE_CURVE_WITH_KNOTS ( ( 3, 2, 2, 3 ),
 ( 0.5869565217391301548, 0.5942028985507243899, 0.6014492753623188470, 0.6086956521739131931 ),
 .UNSPECIFIED. ) 
 CURVE ( )  GEOMETRIC_REPRESENTATION_ITEM ( )  RATIONAL_B_SPLINE_CURVE ( ( 1.000000000000006217, 0.8660254037844326014, 1.000000000000000000, 0.8660254037844387076, 1.000000000000000000, 0.8660254037844367092, 1.000000000000001998 ) ) 
 REPRESENTATION_ITEM ( '' )  );
#25558 = CARTESIAN_POINT ( 'NONE',  ( 11.48171059495397728, 109.8851862821014436, 4.944772684328674117 ) ) ;
#25559 = CARTESIAN_POINT ( 'NONE',  ( 22.60769515458673240, 248.7825961894322973, 6.000000000000000000 ) ) ;
#25560 = LINE ( 'NONE', #22733, #30730 ) ;
#25561 = ORIENTED_EDGE ( 'NONE', *, *, #20025, .T. ) ;
#25562 = CARTESIAN_POINT ( 'NONE',  ( 24.68080903822037442, -3.604726614523240613, 163.7087675451007556 ) ) ;
#25563 = CARTESIAN_POINT ( 'NONE',  ( 23.87821517812499650, 4.985214923628404904, -6.590624999385480187 ) ) ;
#25564 = DIRECTION ( 'NONE',  ( 0.000000000000000000, 0.000000000000000000, 1.000000000000000000 ) ) ;
#25565 = CARTESIAN_POINT ( 'NONE',  ( 34.30304196422265761, 5.407089921784862696, 166.2360015760246199 ) ) ;
#25566 = CARTESIAN_POINT ( 'NONE',  ( 25.24620043574905282, 0.000000000000000000, 167.3765725426477502 ) ) ;
#25567 = CARTESIAN_POINT ( 'NONE',  ( 22.56230152254221011, 3.464101615138862389, -9.187500000000003553 ) ) ;
#25568 = CARTESIAN_POINT ( 'NONE',  ( 21.00000000000000000, 240.2968750006145342, -6.646953231504538984 ) ) ;
#25569 = CARTESIAN_POINT ( 'NONE',  ( 27.24356964374999279, 198.7156250006145513, -15.72908226750539207 ) ) ;
#25570 = CARTESIAN_POINT ( 'NONE',  ( -8.715434833792127023, 124.9398137178985593, 8.962234695871568846 ) ) ;
#25571 = CARTESIAN_POINT ( 'NONE',  ( -11.48171059495397373, 132.8851862821014720, -4.944772684328680334 ) ) ;
#25573 = ORIENTED_EDGE ( 'NONE', *, *, #26449, .F. ) ;
#25572 = ORIENTED_EDGE ( 'NONE', *, *, #33252, .T. ) ;
#25574 = CARTESIAN_POINT ( 'NONE',  ( 15.24356964374999990, 241.1968750006145115, 0.000000000000000000 ) ) ;
#25575 = CARTESIAN_POINT ( 'NONE',  ( -6.932735513424201912, 14.25231371789853441, 10.69584247140429412 ) ) ;
#25576 = CARTESIAN_POINT ( 'NONE',  ( -15.50000000000000533, 98.48981371789855643, 0.1745138560722471477 ) ) ;
#25577 = VECTOR ( 'NONE', #1234, 1000.000000000000000 ) ;
#25578 = CARTESIAN_POINT ( 'NONE',  ( 23.99999999999999645, 244.4499999999999886, -5.196152422706631135 ) ) ;
#25579 = EDGE_CURVE ( 'NONE', #2118, #36527, #6633, .T. ) ;
#25580 = CARTESIAN_POINT ( 'NONE',  ( 21.00000000000000000, -6.646953231504538984, -1.490624999385501193 ) ) ;
#25581 = CARTESIAN_POINT ( 'NONE',  ( 19.68408634441911076, 5.407089921784862696, -7.996874999385533478 ) ) ;
#25582 = CARTESIAN_POINT ( 'NONE',  ( 5.727106289114498080E-15, 198.8750000012290400, 31.17691453623979214 ) ) ;
#25583 = CARTESIAN_POINT ( 'NONE',  ( -2.660918448318275509, 121.0976862821014635, 12.46528703574805874 ) ) ;
#25584 = CARTESIAN_POINT ( 'NONE',  ( 22.80587116629410360, 7.646167579472015790E-16, -2.165624999385551419 ) ) ;
#25585 = CARTESIAN_POINT ( 'NONE',  ( -38.71502896937850124, 217.3034525342667962, -4.350049139982195001 ) ) ;
#25586 = CARTESIAN_POINT ( 'NONE',  ( 15.24356964375000167, 243.9343750006145228, 3.323476615752272600 ) ) ;
#25587 = CARTESIAN_POINT ( 'NONE',  ( 16.56230152254411081, -6.928203230275506996, -1.574999998771003495 ) ) ;
#25588 = CARTESIAN_POINT ( 'NONE',  ( -67.21502896937850835, 215.5714017266979567, -3.350049139982168800 ) ) ;
#25589 = CARTESIAN_POINT ( 'NONE',  ( -4.622313124798576922, 115.6351862821014578, -11.61527771782819762 ) ) ;
#25590 = CARTESIAN_POINT ( 'NONE',  ( 10.56230152254411436, -3.464101615137757051, -4.349999998771036047 ) ) ;
#25591 = CARTESIAN_POINT ( 'NONE',  ( -44.06622103062156981, 211.6261429550005744, 6.530955311639227823 ) ) ;
#25592 = DIRECTION ( 'NONE',  ( 0.000000000000000000, 0.000000000000000000, 1.000000000000000000 ) ) ;
#25593 = CARTESIAN_POINT ( 'NONE',  ( 26.99999999999999645, 7.347880794884117764E-16, -5.568749998770966769 ) ) ;
#25594 = CARTESIAN_POINT ( 'NONE',  ( 13.23911966647218996, 99.24768628210145494, -8.632099005475504683 ) ) ;
#25595 = EDGE_CURVE ( 'NONE', #15548, #19287, #26972, .T. ) ;
#25596 = CARTESIAN_POINT ( 'NONE',  ( 0.1745138560725515708, 24.21018628210144641, -12.50000000000000355 ) ) ;
#25597 = CARTESIAN_POINT ( 'NONE',  ( 26.99999999999999645, 244.3937500012290513, 3.464101615137751278 ) ) ;
#25598 = CARTESIAN_POINT ( 'NONE',  ( 5.529263428287477744, 135.4726862821014777, -7.954856959092191815 ) ) ;
#25599 = AXIS2_PLACEMENT_3D ( 'NONE', #27861, #28049, #1893 ) ;
#25600 = CARTESIAN_POINT ( 'NONE',  ( 19.68408634441910721, 5.407089921784857367, -1.640624999385525973 ) ) ;
#25601 = CARTESIAN_POINT ( 'NONE',  ( 24.89975635843378399, 3.464101615137476831, 163.4166986189574970 ) ) ;
#25602 = ORIENTED_EDGE ( 'NONE', *, *, #7834, .F. ) ;
#25603 = CARTESIAN_POINT ( 'NONE',  ( 11.28998163430637725, -3.344369132205555317, -9.999999999999998224 ) ) ;
#25604 = CARTESIAN_POINT ( 'NONE',  ( 6.594114490232313663, 64.46018628210146062, 6.840914352312096547 ) ) ;
#25605 = CARTESIAN_POINT ( 'NONE',  ( 22.56230152254410370, 7.347880794884117764E-16, -2.362499998771028231 ) ) ;
#25606 = DIRECTION ( 'NONE',  ( 0.000000000000000000, 1.000000000000000000, 0.000000000000000000 ) ) ;
#25607 = CARTESIAN_POINT ( 'NONE',  ( 21.00000000000000355, 0.000000000000000000, 50.00000000000001421 ) ) ;
#25608 = CARTESIAN_POINT ( 'NONE',  ( -1.926257025242585782E-15, 195.6968750006145683, -31.45816453501075927 ) ) ;
#25609 = CARTESIAN_POINT ( 'NONE',  ( 22.56230152254410370, 7.347880794884117764E-16, -8.662499998771028942 ) ) ;
#25610 = FACE_OUTER_BOUND ( 'NONE', #23040, .T. ) ;
#25611 = CARTESIAN_POINT ( 'NONE',  ( -7.954856959092309943, 33.22731371789855359, 5.529263428287300108 ) ) ;
#25612 = CARTESIAN_POINT ( 'NONE',  ( 2.999999999999997335, 244.5000000000000000, 5.000000000000000000 ) ) ;
#25613 = EDGE_LOOP ( 'NONE', ( #16057, #3476, #1547, #12734 ) ) ;
#25614 = CARTESIAN_POINT ( 'NONE',  ( 15.00000000000000000, 241.0562500012290457, 0.000000000000000000 ) ) ;
#25615 = CARTESIAN_POINT ( 'NONE',  ( 12.46528703574811558, 56.80231371789857064, -2.660918448318005947 ) ) ;
#25616 = CARTESIAN_POINT ( 'NONE',  ( 13.44051670066910908, 5.407089921784862696, -9.271874999385531169 ) ) ;
#25617 = CARTESIAN_POINT ( 'NONE',  ( 26.75643035624999655, 3.323476615752271712, -9.440624999385470062 ) ) ;
#25618 = CARTESIAN_POINT ( 'NONE',  ( 2.311890736173452865, 36.67731371789854933, -12.53471296425189152 ) ) ;
#25619 = VERTEX_POINT ( 'NONE', #16779 ) ;
#25620 = CARTESIAN_POINT ( 'NONE',  ( 16.56230152254411436, 7.209453229046482114, -1.209374999385475657 ) ) ;
#25621 = CARTESIAN_POINT ( 'NONE',  ( 7.228626920339068285, 6.672686282101436106, -10.49813415415989581 ) ) ;
#25622 = EDGE_CURVE ( 'NONE', #4681, #21, #14879, .T. ) ;
#25623 = CARTESIAN_POINT ( 'NONE',  ( 24.98639886122932197, 0.000000000000000000, 167.2016752052849426 ) ) ;
#25624 = AXIS2_PLACEMENT_3D ( 'NONE', #22036, #12939, #30375 ) ;
#25625 = CARTESIAN_POINT ( 'NONE',  ( -43.46502896937849414, 215.5714017266979567, -3.350049139982168800 ) ) ;
#25626 = SURFACE_STYLE_FILL_AREA ( #8206 ) ;
#25627 = CARTESIAN_POINT ( 'NONE',  ( 2.999999999999997335, 244.5000000000000000, 2.500000000000000000 ) ) ;
#25628 = CARTESIAN_POINT ( 'NONE',  ( -67.61086230271183695, 212.1499508600178387, -3.954877714930852495 ) ) ;
#25629 = CARTESIAN_POINT ( 'NONE',  ( -39.11830436395489841, 209.8844732041982581, 6.500000000000000888 ) ) ;
#25630 = DIRECTION ( 'NONE',  ( 1.000000000000000000, 0.000000000000000000, 0.000000000000000000 ) ) ;
#25631 = ORIENTED_EDGE ( 'NONE', *, *, #594, .F. ) ;
#25632 = CARTESIAN_POINT ( 'NONE',  ( 0.000000000000000000, 141.0000000000000000, 4.899999999999999467 ) ) ;
#25633 = CARTESIAN_POINT ( 'NONE',  ( 2.999999999999997335, 252.0000000000000000, 2.500000000000000000 ) ) ;
#25634 = CARTESIAN_POINT ( 'NONE',  ( -6.092822981423666739, 17.41481371789854649, -14.25334919248795096 ) ) ;
#25635 = CARTESIAN_POINT ( 'NONE',  ( -30.79836230271183339, 202.5810206699313767, -4.149950860017804111 ) ) ;
#25636 = COLOUR_RGB ( '',0.8941176470588234615, 0.8941176470588234615, 0.8941176470588234615 ) ;
#25637 = CARTESIAN_POINT ( 'NONE',  ( 5.233372021372432847, 138.3476862821014208, 8.152565276336710909 ) ) ;
#25638 = CARTESIAN_POINT ( 'NONE',  ( -8.715434833791929847, 41.46018628210144641, -8.962234695871762469 ) ) ;
#25639 = VECTOR ( 'NONE', #16956, 1000.000000000000000 ) ;
#25640 = CARTESIAN_POINT ( 'NONE',  ( 19.56230152254411792, 5.196152422706637353, -3.750000000000031086 ) ) ;
#25641 = DIRECTION ( 'NONE',  ( 1.000000000000000000, 0.000000000000000000, 0.000000000000000000 ) ) ;
#25642 = ORIENTED_EDGE ( 'NONE', *, *, #36458, .F. ) ;
#25643 = CARTESIAN_POINT ( 'NONE',  ( 14.25334919248782661, 17.88518628210143646, 6.092822981423971385 ) ) ;
#25644 = CARTESIAN_POINT ( 'NONE',  ( -7.234628195640354420, 196.1549038117966859, 26.99999999999996803 ) ) ;
#25645 = CARTESIAN_POINT ( 'NONE',  ( 13.62178482187501416, 198.2093750006145285, 23.59362340125806767 ) ) ;
#25646 = CARTESIAN_POINT ( 'NONE',  ( 31.45868912971818432, 0.000000000000000000, 169.5433637710095809 ) ) ;
#25647 = FACE_OUTER_BOUND ( 'NONE', #37084, .T. ) ;
#25648 = CARTESIAN_POINT ( 'NONE',  ( 26.99999999999999645, 246.2687500012290513, -3.464101615137755275 ) ) ;
#25649 = EDGE_CURVE ( 'NONE', #27232, #5916, #17268, .T. ) ;
#25650 = CARTESIAN_POINT ( 'NONE',  ( 18.12178482187499640, 244.3843750006145115, -4.985214923628404904 ) ) ;
#25651 = CARTESIAN_POINT ( 'NONE',  ( 9.534712964251900402, 112.5773137178985479, 1.715153634034445540 ) ) ;
#25652 = CARTESIAN_POINT ( 'NONE',  ( 20.99999999999999645, 241.4218750006145626, 6.646953231504538984 ) ) ;
#25653 = EDGE_LOOP ( 'NONE', ( #5708, #15569 ) ) ;
#25654 = CARTESIAN_POINT ( 'NONE',  ( -64.05580436395490551, 216.5000000000000000, 0.1155267958017343610 ) ) ;
#25655 = CARTESIAN_POINT ( 'NONE',  ( -27.00000000000000355, 195.9125000000000796, -15.58845726811989429 ) ) ;
#25656 = CARTESIAN_POINT ( 'NONE',  ( 26.99999999999999645, 248.0687500012290343, -3.464101615137755275 ) ) ;
#25657 = EDGE_LOOP ( 'NONE', ( #19355, #34955, #13049, #4987, #14903 ) ) ;
#25658 = CARTESIAN_POINT ( 'NONE',  ( 4.944772684328420986, 123.2148137178985650, 11.48171059495408208 ) ) ;
#25659 = CARTESIAN_POINT ( 'NONE',  ( 13.44051670066911441, -5.407089921784859143, -8.165624999385528326 ) ) ;
#25660 = CARTESIAN_POINT ( 'NONE',  ( 30.86793661096031727, -7.209453229046475009, 162.7910315836186328 ) ) ;
#25661 = CARTESIAN_POINT ( 'NONE',  ( 21.00000000000000000, 6.646953231504538984, -0.3656249993854637226 ) ) ;
#25662 = CARTESIAN_POINT ( 'NONE',  ( -27.00000000000000355, 195.4625000000000057, -15.58845726811989429 ) ) ;
#25663 = ORIENTED_EDGE ( 'NONE', *, *, #18461, .T. ) ;
#25664 = ORIENTED_EDGE ( 'NONE', *, *, #27143, .F. ) ;
#25665 = ORIENTED_EDGE ( 'NONE', *, *, #13511, .T. ) ;
#25666 = CARTESIAN_POINT ( 'NONE',  ( 15.00000000000000000, 3.464101615137752166, -7.631249998770947229 ) ) ;
#25668 = AXIS2_PLACEMENT_3D ( 'NONE', #15269, #4076, #32320 ) ;
#25667 = CARTESIAN_POINT ( 'NONE',  ( 18.12178482187499640, 4.985214923628404904, -1.565624999385478722 ) ) ;
#25669 = DIRECTION ( 'NONE',  ( 1.000000000000000000, 0.000000000000000000, 0.000000000000000000 ) ) ;
#25671 = LINE ( 'NONE', #32237, #13590 ) ;
#25670 = PRODUCT_DEFINITION_FORMATION_WITH_SPECIFIED_SOURCE ( 'ANY', '', #28915, .NOT_KNOWN. ) ;
#25672 = CARTESIAN_POINT ( 'NONE',  ( 21.00000000000000000, 249.4093750006145171, 6.646953231504538984 ) ) ;
#25673 = CARTESIAN_POINT ( 'NONE',  ( -2.311890736173176641, 60.72268628210144925, -12.53471296425194836 ) ) ;
#25674 = EDGE_CURVE ( 'NONE', #26056, #12051, #36061, .T. ) ;
#25675 = AXIS2_PLACEMENT_3D ( 'NONE', #12338, #9503, #15188 ) ;
#25676 = AXIS2_PLACEMENT_3D ( 'NONE', #33378, #13668, #4750 ) ;
#25677 = CARTESIAN_POINT ( 'NONE',  ( -66.22544563604516554, 214.8429017333602360, 4.673758765035156415 ) ) ;
#25678 = CARTESIAN_POINT ( 'NONE',  ( 5.409584567223228113, 215.8464057872915589, -1.363118671453956265 ) ) ;
#25679 = CARTESIAN_POINT ( 'NONE',  ( -47.81919563604517265, 214.5000000000000284, -0.1155267958017627827 ) ) ;
#25680 = SURFACE_SIDE_STYLE ('',( #17159 ) ) ;
#25681 = CARTESIAN_POINT ( 'NONE',  ( 31.04687824534265417, -6.928203230275506996, 164.8363438237504397 ) ) ;
#25682 = CARTESIAN_POINT ( 'NONE',  ( 11.61527771782809637, 103.6648137178985678, 4.622313124798827388 ) ) ;
#25683 = CARTESIAN_POINT ( 'NONE',  ( -40.10788769728823411, 216.4690446883607535, 1.857196546604031662 ) ) ;
#25684 = CARTESIAN_POINT ( 'NONE',  ( -47.43080436395489841, 201.5000000000000000, -0.1155267958017054536 ) ) ;
#25685 = EDGE_CURVE ( 'NONE', #28635, #9537, #31181, .T. ) ;
#25686 = CARTESIAN_POINT ( 'NONE',  ( 18.12178482187500350, -4.985214923628407568, -3.328124999385479121 ) ) ;
#25687 = FACE_OUTER_BOUND ( 'NONE', #28829, .T. ) ;
#25688 = CARTESIAN_POINT ( 'NONE',  ( -13.04141134922778456, 97.62731371789854506, 8.927990412390377273 ) ) ;
#25689 = CARTESIAN_POINT ( 'NONE',  ( -32.18377896937850835, 208.3738570449995109, 6.530955311639247363 ) ) ;
#25690 = ORIENTED_EDGE ( 'NONE', *, *, #7768, .F. ) ;
#25691 = CARTESIAN_POINT ( 'NONE',  ( 18.00000000000000355, -5.196152422706632912, -6.674999999999986500 ) ) ;
#25692 = CARTESIAN_POINT ( 'NONE',  ( 10.69584247140445221, 99.24768628210146915, -6.932735513423970097 ) ) ;
#25693 = CARTESIAN_POINT ( 'NONE',  ( 3.257655550457285720, 70.49768628210145494, -15.46528703574804986 ) ) ;
#25694 = CARTESIAN_POINT ( 'NONE',  ( 27.65834674205753529, 5.407089921784862696, 161.9237153725250664 ) ) ;
#25695 = CARTESIAN_POINT ( 'NONE',  ( -8.632099005475501130, 60.14768628210144641, -13.23911966647218996 ) ) ;
#25696 = CARTESIAN_POINT ( 'NONE',  ( 16.56230152254411436, -7.209453229046475009, -7.228124999385518556 ) ) ;
#25697 = CARTESIAN_POINT ( 'NONE',  ( 5.233372021372432847, 18.74768628210143362, 8.152565276336710909 ) ) ;
#25698 = LINE ( 'NONE', #14695, #18290 ) ;
#25699 = CARTESIAN_POINT ( 'NONE',  ( -62.67038769728823411, 208.1428034533959703, 6.469044688360770401 ) ) ;
#25700 = DIRECTION ( 'NONE',  ( 1.000000000000000000, 0.000000000000000000, 0.000000000000000000 ) ) ;
#25701 = CARTESIAN_POINT ( 'NONE',  ( 8.962234695871762469, 52.96018628210144641, -8.715434833791931624 ) ) ;
#25702 = CARTESIAN_POINT ( 'NONE',  ( -26.99999999999998934, 198.2374999999999829, 15.58845726811991561 ) ) ;
#25703 = DIRECTION ( 'NONE',  ( -0.000000000000000000, 1.000000000000000000, -0.000000000000000000 ) ) ;
#25704 = CARTESIAN_POINT ( 'NONE',  ( 9.500000000000005329, 17.31018628210144428, 0.1745138560725188748 ) ) ;
#25705 = DIRECTION ( 'NONE',  ( 0.000000000000000000, 0.000000000000000000, 1.000000000000000000 ) ) ;
#25706 = ORIENTED_EDGE ( 'NONE', *, *, #17252, .F. ) ;
#25707 = CARTESIAN_POINT ( 'NONE',  ( 21.00000000000000000, -6.928203230275506996, -4.837499999999994138 ) ) ;
#25708 = CYLINDRICAL_SURFACE ( 'NONE', #33624, 3.500000000000002220 ) ;
#25709 = CARTESIAN_POINT ( 'NONE',  ( 36.89328133622495898, -3.604726614523238837, 160.0241092138036834 ) ) ;
#25710 = CARTESIAN_POINT ( 'NONE',  ( 10.31873187879411091, -3.604726614523240613, -1.453124999385536187 ) ) ;
#25711 = CARTESIAN_POINT ( 'NONE',  ( 25.11222996482124259, -3.604726614523240613, 168.6399313006548653 ) ) ;
#25712 = CARTESIAN_POINT ( 'NONE',  ( 21.00000000000000000, 244.7125000000000057, 6.928203230275506996 ) ) ;
#25713 = EDGE_CURVE ( 'NONE', #15610, #37311, #20932, .T. ) ;
#25714 = CARTESIAN_POINT ( 'NONE',  ( 20.99999999999999645, 0.000000000000000000, -8.000000000000000000 ) ) ;
#25715 = CARTESIAN_POINT ( 'NONE',  ( 0.1745138560725515708, 70.21018628210144641, -12.50000000000000355 ) ) ;
#25716 = ORIENTED_EDGE ( 'NONE', *, *, #4108, .T. ) ;
#25717 = ORIENTED_EDGE ( 'NONE', *, *, #34391, .T. ) ;
#25718 = CARTESIAN_POINT ( 'NONE',  ( 5.727106289114498080E-15, 196.1750000012290513, 31.17691453623979214 ) ) ;
#25719 = CARTESIAN_POINT ( 'NONE',  ( 20.99999999999999645, 6.928203230275506996, -5.006249998770934795 ) ) ;
#25720 = CARTESIAN_POINT ( 'NONE',  ( -15.46528703574811736, 33.80231371789854222, 3.257655550456946436 ) ) ;
#25721 = EDGE_CURVE ( 'NONE', #36284, #1170, #26040, .T. ) ;
#25722 = CARTESIAN_POINT ( 'NONE',  ( 23.87821517812499650, 4.985214923628404904, -8.503124999385491378 ) ) ;
#25723 = CARTESIAN_POINT ( 'NONE',  ( 26.75643035624999655, 243.3343750006145285, -7.049594010296217766E-16 ) ) ;
#25724 = CARTESIAN_POINT ( 'NONE',  ( -46.83705436395489130, 206.7903428501026042, -3.378800118222489157 ) ) ;
#25725 = CYLINDRICAL_SURFACE ( 'NONE', #26429, 2.649999999999991029 ) ;
#25726 = CARTESIAN_POINT ( 'NONE',  ( 37.01094158893428698, -3.604726614523238837, 161.3689720562275340 ) ) ;
#25727 = CARTESIAN_POINT ( 'NONE',  ( -8.710071997420207879, 24.31481371789855217, 3.796722387233182339 ) ) ;
#25728 = CARTESIAN_POINT ( 'NONE',  ( 19.68408634441910365, 5.407089921784857367, -9.290624999385570959 ) ) ;
#25729 = CIRCLE ( 'NONE', #17349, 2.649999999999991029 ) ;
#25730 = FILL_AREA_STYLE_COLOUR ( '', #18412 ) ;
#25731 = CARTESIAN_POINT ( 'NONE',  ( 23.27690126865536158, 194.9999999999999716, -13.80801991767920534 ) ) ;
#25732 = CARTESIAN_POINT ( 'NONE',  ( 13.62178482187501416, 195.9593750006145569, 23.59362340125806767 ) ) ;
#25733 = CARTESIAN_POINT ( 'NONE',  ( 0.1745138560722779009, 13.38981371789854613, 12.50000000000000355 ) ) ;
#25734 = ORIENTED_EDGE ( 'NONE', *, *, #15285, .F. ) ;
#25735 = CARTESIAN_POINT ( 'NONE',  ( 12.53471296425194836, 63.02268628210145351, -2.311890736173178418 ) ) ;
#25736 = CARTESIAN_POINT ( 'NONE',  ( 15.00000000000000000, 240.5124999999999602, -3.464101615137752610 ) ) ;
#25737 = LINE ( 'NONE', #22534, #24737 ) ;
#25738 = CARTESIAN_POINT ( 'NONE',  ( 36.85896376251805151, -3.604726614523235284, 159.6318575514300449 ) ) ;
#25739 = CARTESIAN_POINT ( 'NONE',  ( 15.00000000000000178, -3.464101615137757051, -2.156249998770940923 ) ) ;
#25740 = CARTESIAN_POINT ( 'NONE',  ( 19.68408634441910721, 5.407089921784862696, -9.796874999385529748 ) ) ;
#25741 = CARTESIAN_POINT ( 'NONE',  ( 36.94560626531313829, 7.347880794884125653E-16, 163.4168341377576041 ) ) ;
#25742 = CARTESIAN_POINT ( 'NONE',  ( -8.152565276336710909, 85.44768628210142936, 5.233372021372435512 ) ) ;
#25743 = CARTESIAN_POINT ( 'NONE',  ( 15.00000000000000000, 249.5124999999999602, -3.464101615137752610 ) ) ;
#25744 = CARTESIAN_POINT ( 'NONE',  ( 12.50000000000000355, 109.3101862821014549, 0.1745138560725507937 ) ) ;
#25745 = CARTESIAN_POINT ( 'NONE',  ( 22.60769515458672885, 240.4736538117967086, -5.999999999999998224 ) ) ;
#25746 = ORIENTED_EDGE ( 'NONE', *, *, #23719, .T. ) ;
#25747 = CARTESIAN_POINT ( 'NONE',  ( 30.82871652672388052, -7.209453229046475009, 162.3427439694773398 ) ) ;
#25748 = CARTESIAN_POINT ( 'NONE',  ( 18.12178482187499640, 4.985214923628404904, -7.865624999385478766 ) ) ;
#25749 = CARTESIAN_POINT ( 'NONE',  ( 20.99999999999999645, 185.0294372515228645, -5.999999999999999112 ) ) ;
#25750 = CARTESIAN_POINT ( 'NONE',  ( 37.56002276824448671, -3.604726614523238837, 167.6449986542055797 ) ) ;
#25751 = CARTESIAN_POINT ( 'NONE',  ( 28.16288104225748512, -5.196152422706638241, 166.2932446884790920 ) ) ;
#25752 = DIRECTION ( 'NONE',  ( 0.000000000000000000, 1.000000000000000000, 0.000000000000000000 ) ) ;
#25753 = CARTESIAN_POINT ( 'NONE',  ( 18.00000000000000355, 249.6250000000000000, 5.196152422706632912 ) ) ;
#25754 = CARTESIAN_POINT ( 'NONE',  ( 13.62178482187499640, 197.8531250006145399, -23.59362340125807123 ) ) ;
#25755 = VECTOR ( 'NONE', #24689, 1000.000000000000000 ) ;
#25756 = CARTESIAN_POINT ( 'NONE',  ( 12.53471296425189330, 121.7773137178985792, 2.311890736173451977 ) ) ;
#25757 = CARTESIAN_POINT ( 'NONE',  ( -7.228626920339070061, 121.6726862821014521, 10.49813415415989404 ) ) ;
#25759 = VERTEX_POINT ( 'NONE', #2171 ) ;
#25758 = ORIENTED_EDGE ( 'NONE', *, *, #15239, .F. ) ;
#25760 = CARTESIAN_POINT ( 'NONE',  ( 21.00000000000000000, 242.4343750006145228, -6.646953231504538984 ) ) ;
#25761 = CARTESIAN_POINT ( 'NONE',  ( 10.56230152254411081, 0.000000000000000000, -2.137499998771025034 ) ) ;
#25762 = CARTESIAN_POINT ( 'NONE',  ( 15.50000000000000533, 103.0898137178985792, -0.1745138560722452326 ) ) ;
#25763 =( BOUNDED_CURVE ( )  B_SPLINE_CURVE ( 2, ( #11499, #14530, #11681, #26086, #8657, #31771, #9216 ),
 .UNSPECIFIED., .F., .T. ) 
 B_SPLINE_CURVE_WITH_KNOTS ( ( 3, 2, 2, 3 ),
 ( 0.8913043478260880281, 0.8985507246376823742, 0.9057971014492767203, 0.9130434782608709554 ),
 .UNSPECIFIED. ) 
 CURVE ( )  GEOMETRIC_REPRESENTATION_ITEM ( )  RATIONAL_B_SPLINE_CURVE ( ( 0.9999999999999794609, 0.8660254037844592467, 1.000000000000000000, 0.8660254037844387076, 1.000000000000000000, 0.8660254037844120623, 1.000000000000026645 ) ) 
 REPRESENTATION_ITEM ( '' )  );
#25764 = CARTESIAN_POINT ( 'NONE',  ( 10.49813415415989581, 91.77268628210144641, 7.228626920339068285 ) ) ;
#25765 = CARTESIAN_POINT ( 'NONE',  ( 15.24356964374999990, 3.323476615752268604, -2.090624999385484628 ) ) ;
#25766 = CARTESIAN_POINT ( 'NONE',  ( -27.00000000000000355, 196.9250000012290229, -15.58845726811989429 ) ) ;
#25767 = CARTESIAN_POINT ( 'NONE',  ( 11.61527771782819940, 117.9351862821014549, -4.622313124798573369 ) ) ;
#25768 = CARTESIAN_POINT ( 'NONE',  ( 13.44051670066911797, -5.407089921784859143, -4.115624999385558702 ) ) ;
#25769 = CARTESIAN_POINT ( 'NONE',  ( 23.87821517812500005, 243.5968750006145171, 4.985214923628404016 ) ) ;
#25770 = CARTESIAN_POINT ( 'NONE',  ( 33.88185034302515675, -5.196152422706629359, 162.8190834401207496 ) ) ;
#25771 = CARTESIAN_POINT ( 'NONE',  ( -53.75669563604516554, 209.8844732041982013, -6.500000000000000888 ) ) ;
#25772 = CARTESIAN_POINT ( 'NONE',  ( -12.53471296425194836, 113.6226862821014407, 2.311890736173176641 ) ) ;
#25773 = CARTESIAN_POINT ( 'NONE',  ( 10.56230152254411436, -3.464101615137757051, -2.999999998771016418 ) ) ;
#25774 = AXIS2_PLACEMENT_3D ( 'NONE', #2295, #13687, #16340 ) ;
#25775 =( BOUNDED_CURVE ( )  B_SPLINE_CURVE ( 2, ( #22854, #11467, #2561, #14131, #26053, #26419, #81 ),
 .UNSPECIFIED., .F., .F. ) 
 B_SPLINE_CURVE_WITH_KNOTS ( ( 3, 2, 2, 3 ),
 ( 0.3695652173913038241, 0.3768115942028981702, 0.3840579710144924608, 0.3913043478260868069 ),
 .UNSPECIFIED. ) 
 CURVE ( )  GEOMETRIC_REPRESENTATION_ITEM ( )  RATIONAL_B_SPLINE_CURVE ( ( 1.000000000000009104, 0.8660254037844293817, 1.000000000000000000, 0.8660254037844387076, 1.000000000000000000, 0.8660254037844418162, 0.9999999999999968914 ) ) 
 REPRESENTATION_ITEM ( '' )  );
#25776 = CARTESIAN_POINT ( 'NONE',  ( -40.10788769728823411, 216.4690446883607535, 1.857196546604031662 ) ) ;
#25777 = DIRECTION ( 'NONE',  ( 1.000000000000000000, 0.000000000000000000, 0.000000000000000000 ) ) ;
#25778 = CYLINDRICAL_SURFACE ( 'NONE', #226, 5.000000000000000000 ) ;
#25779 = CARTESIAN_POINT ( 'NONE',  ( -8.632099005475501130, 106.1476862821014322, -13.23911966647218996 ) ) ;
#25780 = CARTESIAN_POINT ( 'NONE',  ( -11.61527771782819940, 21.33518628210144641, 4.622313124798574258 ) ) ;
#25781 = CARTESIAN_POINT ( 'NONE',  ( 26.99999999999985789, -3.464101615137830770, -0.2625000000000126121 ) ) ;
#25782 = CARTESIAN_POINT ( 'NONE',  ( 7.234628195640363302, 196.8299038117967257, -26.99999999999996803 ) ) ;
#25783 = CARTESIAN_POINT ( 'NONE',  ( 5.233372021372432847, 138.3476862821014208, 8.152565276336710909 ) ) ;
#25784 = ADVANCED_FACE ( 'NONE', ( #5203 ), #13753, .F. ) ;
#25785 = CARTESIAN_POINT ( 'NONE',  ( 24.65789917220240213, 0.000000000000000000, 160.6522583305284968 ) ) ;
#25786 = ORIENTED_EDGE ( 'NONE', *, *, #29045, .T. ) ;
#25787 = CARTESIAN_POINT ( 'NONE',  ( 34.50404489593442747, 5.407089921784857367, 168.5334755984986828 ) ) ;
#25788 = CARTESIAN_POINT ( 'NONE',  ( -9.465287035748065847, 68.19768628210142936, -2.064181346179273735 ) ) ;
#25789 = AXIS2_PLACEMENT_3D ( 'NONE', #31146, #8397, #28472 ) ;
#25790 = CARTESIAN_POINT ( 'NONE',  ( 22.56230152254410370, 7.347880794884117764E-16, -5.962499998771020771 ) ) ;
#25791 = CYLINDRICAL_SURFACE ( 'NONE', #20803, 5.999999999999999112 ) ;
#25792 = CARTESIAN_POINT ( 'NONE',  ( -27.24356964374999990, 195.7718750006145569, -15.72908226750537786 ) ) ;
#25793 = CARTESIAN_POINT ( 'NONE',  ( 8.433054386417008885, 195.0000000000000284, 25.92026892250748205 ) ) ;
#25794 = CARTESIAN_POINT ( 'NONE',  ( 37.41624727615045742, 7.347880794884125653E-16, 168.7962855074530069 ) ) ;
#25795 = CARTESIAN_POINT ( 'NONE',  ( -7.954856959092309943, 42.42731371789855643, 5.529263428287300108 ) ) ;
#25796 = CARTESIAN_POINT ( 'NONE',  ( -13.62178482187498396, 198.5843750006145569, 23.59362340125808188 ) ) ;
#25797 = ORIENTED_EDGE ( 'NONE', *, *, #1154, .F. ) ;
#25798 = ORIENTED_EDGE ( 'NONE', *, *, #10991, .F. ) ;
#25799 = CARTESIAN_POINT ( 'NONE',  ( 15.24356964374999990, 248.8468750006145171, 0.000000000000000000 ) ) ;
#25800 = CARTESIAN_POINT ( 'NONE',  ( 10.49813415416005213, 37.82731371789854791, -7.228626920338837358 ) ) ;
#25801 = CARTESIAN_POINT ( 'NONE',  ( 13.44051670066910731, 5.407089921784862696, -7.921874999385513760 ) ) ;
#25802 = CARTESIAN_POINT ( 'NONE',  ( 15.24356964375000167, -3.323476615752272600, -9.665624999385482141 ) ) ;
#25803 = CARTESIAN_POINT ( 'NONE',  ( -2.908627838312453306, 142.4773137178985678, 15.53471296425188797 ) ) ;
#25804 = EDGE_CURVE ( 'NONE', #28136, #4445, #24795, .T. ) ;
#25805 = VECTOR ( 'NONE', #2613, 1000.000000000000000 ) ;
#25806 = ORIENTED_EDGE ( 'NONE', *, *, #12248, .F. ) ;
#25807 = CARTESIAN_POINT ( 'NONE',  ( 16.56230152254411792, -7.209453229046482114, -0.5343749993854981506 ) ) ;
#25808 = CARTESIAN_POINT ( 'NONE',  ( -27.00000000000000355, 200.0000000000000000, 0.000000000000000000 ) ) ;
#25809 = CARTESIAN_POINT ( 'NONE',  ( 34.21152843433763024, -5.407089921784861808, 165.1899971430282505 ) ) ;
#25810 = ADVANCED_FACE ( 'NONE', ( #5568 ), #11454, .T. ) ;
#25811 = CARTESIAN_POINT ( 'NONE',  ( -37.52752896937850124, 213.3500491399821613, 5.571401726697954970 ) ) ;
#25812 = DIRECTION ( 'NONE',  ( -0.000000000000000000, 1.000000000000000000, -0.000000000000000000 ) ) ;
#25813 =( NAMED_UNIT ( * ) SI_UNIT ( $, .STERADIAN. ) SOLID_ANGLE_UNIT ( ) );
#25814 = VECTOR ( 'NONE', #26650, 1000.000000000000000 ) ;
#25815 = CARTESIAN_POINT ( 'NONE',  ( -22.11840882573491740, 195.0000000000000284, 15.80876310588338463 ) ) ;
#25816 = CARTESIAN_POINT ( 'NONE',  ( -62.46502896937850124, 213.8393509191290889, -2.350049139982142155 ) ) ;
#25817 = CARTESIAN_POINT ( 'NONE',  ( -40.89955436395488420, 214.8429017333601792, -4.673758765035196383 ) ) ;
#25818 = CARTESIAN_POINT ( 'NONE',  ( 25.15145004905768644, -3.604726614523240613, 169.0882189147961583 ) ) ;
#25819 = ORIENTED_EDGE ( 'NONE', *, *, #3801, .F. ) ;
#25820 = CARTESIAN_POINT ( 'NONE',  ( -27.00000000000000355, 196.8500000000000227, 0.000000000000000000 ) ) ;
#25821 = CARTESIAN_POINT ( 'NONE',  ( 11.62741699796951345, 213.5147186257614180, -6.000000000000000000 ) ) ;
#25822 = CARTESIAN_POINT ( 'NONE',  ( 2.908627838312458636, 27.47731371789854649, -15.53471296425188442 ) ) ;
#25823 = CARTESIAN_POINT ( 'NONE',  ( -38.31919563604515844, 218.5000000000000000, -0.1155267958018185298 ) ) ;
#25824 = CARTESIAN_POINT ( 'NONE',  ( 7.228626920339068285, 15.87268628210144961, -10.49813415415989581 ) ) ;
#25825 = CARTESIAN_POINT ( 'NONE',  ( 4.944772684328679446, 43.18518628210144072, -11.48171059495397373 ) ) ;
#25826 = CARTESIAN_POINT ( 'NONE',  ( 19.56230152254412502, -5.196152422706635576, -3.450000000000091660 ) ) ;
#25827 = VERTEX_POINT ( 'NONE', #34571 ) ;
#25828 = CARTESIAN_POINT ( 'NONE',  ( -47.00000000000000711, 244.5000000000000000, -5.000000000000000000 ) ) ;
#25829 = EDGE_CURVE ( 'NONE', #26637, #3147, #8611, .T. ) ;
#25830 = CARTESIAN_POINT ( 'NONE',  ( -27.24356964374999635, 196.7468750006145797, 15.72908226750539384 ) ) ;
#25831 = CARTESIAN_POINT ( 'NONE',  ( 13.56230152254411614, -5.196152422706632912, -6.562499998771037291 ) ) ;
#25832 = DIRECTION ( 'NONE',  ( 0.08715574274765143514, 0.000000000000000000, 0.9961946980917462113 ) ) ;
#25833 = DIRECTION ( 'NONE',  ( 1.000000000000000000, 0.000000000000000000, 0.000000000000000000 ) ) ;
#25834 = DIRECTION ( 'NONE',  ( 0.000000000000000000, 0.000000000000000000, -1.000000000000000000 ) ) ;
#25835 = CARTESIAN_POINT ( 'NONE',  ( 26.75643035624999655, 246.4468750006144830, 3.323476615752267715 ) ) ;
#25836 = CARTESIAN_POINT ( 'NONE',  ( 9.534712964251900402, 94.17731371789857064, 1.715153634034445540 ) ) ;
#25837 = CARTESIAN_POINT ( 'NONE',  ( 26.75643035624999655, 241.9843750006145342, -7.049594010296217766E-16 ) ) ;
#25838 = ORIENTED_EDGE ( 'NONE', *, *, #23360, .T. ) ;
#25839 = CARTESIAN_POINT ( 'NONE',  ( -50.39955436395490551, 214.8429017333601792, -4.673758765035196383 ) ) ;
#25840 = CARTESIAN_POINT ( 'NONE',  ( 1.069080835302379631E-14, 198.3124999999999716, 27.00000000000000000 ) ) ;
#25841 = CIRCLE ( 'NONE', #32524, 5.500000000000005329 ) ;
#25842 = CARTESIAN_POINT ( 'NONE',  ( 26.99999999999999645, 245.3687500012290457, -3.464101615137755275 ) ) ;
#25843 = VERTEX_POINT ( 'NONE', #17336 ) ;
#25844 = CARTESIAN_POINT ( 'NONE',  ( -11.61527771782809282, 117.4648137178985650, -4.622313124798832717 ) ) ;
#25845 = EDGE_CURVE ( 'NONE', #19865, #11078, #34199, .T. ) ;
#25846 = CARTESIAN_POINT ( 'NONE',  ( 16.56230152254412147, -7.209453229046482114, -0.9843749993855260838 ) ) ;
#25847 = CARTESIAN_POINT ( 'NONE',  ( 33.98111043944852128, -5.407089921784855591, 162.5563074099482037 ) ) ;
#25848 = CARTESIAN_POINT ( 'NONE',  ( 23.87821517812499650, 4.985214923628404904, -2.653124999385497951 ) ) ;
#25849 = CARTESIAN_POINT ( 'NONE',  ( 7.228626920338837358, 58.52731371789855785, 10.49813415416005036 ) ) ;
#25850 = CARTESIAN_POINT ( 'NONE',  ( 27.24356964375000345, 199.1843750006145228, -3.336375036156643733E-15 ) ) ;
#25851 = VERTEX_POINT ( 'NONE', #17707 ) ;
#25852 = VERTEX_POINT ( 'NONE', #23579 ) ;
#25853 = ORIENTED_EDGE ( 'NONE', *, *, #11660, .F. ) ;
#25854 = CARTESIAN_POINT ( 'NONE',  ( 26.99999999999999645, 7.347880794884117764E-16, -6.918749998770956644 ) ) ;
#25855 = CARTESIAN_POINT ( 'NONE',  ( 15.24356964375000167, -3.323476615752272600, -2.803124999385491201 ) ) ;
#25856 = CARTESIAN_POINT ( 'NONE',  ( 26.75643035624999655, 245.9593750006145001, -3.323476615752271712 ) ) ;
#25857 = EDGE_CURVE ( 'NONE', #19019, #12668, #3289, .T. ) ;
#25858 = CARTESIAN_POINT ( 'NONE',  ( 8.962234695871762469, 62.16018628210144215, -8.715434833791931624 ) ) ;
#25859 = CARTESIAN_POINT ( 'NONE',  ( -54.35044563604515844, 205.1570982666397072, -4.673758765035155527 ) ) ;
#25860 = SURFACE_SIDE_STYLE ('',( #2919 ) ) ;
#25861 = CARTESIAN_POINT ( 'NONE',  ( -39.50669563604516554, 209.8844732041982297, -4.499999999999996447 ) ) ;
#25862 = CARTESIAN_POINT ( 'NONE',  ( 0.000000000000000000, 0.000000000000000000, 0.000000000000000000 ) ) ;
#25863 = CARTESIAN_POINT ( 'NONE',  ( 33.85570362020085611, 5.196152422706631135, 162.5202250306932399 ) ) ;
#25864 = CARTESIAN_POINT ( 'NONE',  ( -6.932735513424201912, 97.05231371789857064, 10.69584247140429412 ) ) ;
#25865 = CARTESIAN_POINT ( 'NONE',  ( -69.79538769728823411, 211.3212981617418222, -4.469044688360751749 ) ) ;
#25866 = CARTESIAN_POINT ( 'NONE',  ( -44.85788769728823411, 218.4690446883607535, 2.393094931466250408 ) ) ;
#25867 = EDGE_CURVE ( 'NONE', #26175, #4359, #17052, .T. ) ;
#25868 = CARTESIAN_POINT ( 'NONE',  ( 15.24356964374999990, 0.000000000000000000, -4.753124999385488714 ) ) ;
#25869 = DIRECTION ( 'NONE',  ( -1.000000000000000000, 0.000000000000000000, 0.000000000000000000 ) ) ;
#25870 = CARTESIAN_POINT ( 'NONE',  ( -2.908627838312453306, 68.87731371789855928, 15.53471296425188797 ) ) ;
#25871 = CARTESIAN_POINT ( 'NONE',  ( -68.00669563604516554, 209.8844732041981729, -8.500000000000003553 ) ) ;
#25872 = AXIS2_PLACEMENT_3D ( 'NONE', #19343, #1877, #22919 ) ;
#25873 = ORIENTED_EDGE ( 'NONE', *, *, #33185, .T. ) ;
#25874 = CARTESIAN_POINT ( 'NONE',  ( -49.64999999999999858, 244.5000000000000000, 2.500000000000000000 ) ) ;
#25875 = CARTESIAN_POINT ( 'NONE',  ( 4.944772684328679446, 107.5851862821014464, -11.48171059495397373 ) ) ;
#25876 = CARTESIAN_POINT ( 'NONE',  ( -10.83675517735155047, 50.66018628210144925, -11.08355503943142750 ) ) ;
#25877 = DIRECTION ( 'NONE',  ( -0.000000000000000000, -1.000000000000000000, -0.000000000000000000 ) ) ;
#25878 = CARTESIAN_POINT ( 'NONE',  ( 33.87162103762178589, 5.407089921784862696, 161.3048378204704534 ) ) ;
#25879 = CARTESIAN_POINT ( 'NONE',  ( -13.23911966647218463, 57.84768628210144925, 8.632099005475506459 ) ) ;
#25880 = EDGE_CURVE ( 'NONE', #5473, #25013, #18089, .T. ) ;
#25881 = CARTESIAN_POINT ( 'NONE',  ( 19.68408634441910365, 5.407089921784857367, -9.740624999385548932 ) ) ;
#25882 = CARTESIAN_POINT ( 'NONE',  ( 23.99999999999999645, 5.196152422706631135, -4.200000000000009059 ) ) ;
#25883 = CARTESIAN_POINT ( 'NONE',  ( -51.19122103062155560, 208.3738570449993404, -6.530955311639226935 ) ) ;
#25884 = DIRECTION ( 'NONE',  ( 1.000000000000000000, 0.000000000000000000, 0.000000000000000000 ) ) ;
#25885 = CARTESIAN_POINT ( 'NONE',  ( 4.622313124798573369, 46.63518628210145067, 11.61527771782819940 ) ) ;
#25886 = CARTESIAN_POINT ( 'NONE',  ( -27.00000000000000355, 197.7125000000000057, -15.58845726811989429 ) ) ;
#25887 = CARTESIAN_POINT ( 'NONE',  ( 23.99999999999999645, 5.196152422706631135, -3.693749998770950782 ) ) ;
#25888 = CARTESIAN_POINT ( 'NONE',  ( -3.796722387233375073, 10.98518628210143433, 8.710071997420127943 ) ) ;
#25889 = CARTESIAN_POINT ( 'NONE',  ( 22.56230152254410370, 0.000000000000000000, -10.00000000000000000 ) ) ;
#25890 = VERTEX_POINT ( 'NONE', #8983 ) ;
#25891 = CARTESIAN_POINT ( 'NONE',  ( 15.00000000000000000, 0.000000000000000000, -4.500000000000003553 ) ) ;
#25893 = LINE ( 'NONE', #37441, #13672 ) ;
#25892 = PRODUCT_DEFINITION_SHAPE ( 'NONE', 'NONE',  #10201 ) ;
#25894 = CARTESIAN_POINT ( 'NONE',  ( 24.43404934156608022, 3.604726614523240613, 160.8882913061285080 ) ) ;
#25895 = CARTESIAN_POINT ( 'NONE',  ( 22.80587116629410716, 7.646167579472015790E-16, -4.865624999385531169 ) ) ;
#25896 = CARTESIAN_POINT ( 'NONE',  ( 27.61379986294728184, -5.196152422706638241, 160.0172180905011032 ) ) ;
#25897 = CARTESIAN_POINT ( 'NONE',  ( 24.00000000000000000, 240.6999999999999886, 5.196152422706629359 ) ) ;
#25898 = CARTESIAN_POINT ( 'NONE',  ( -7.234628195640302017, 196.6049038117967029, 27.00000000000000711 ) ) ;
#25899 = CARTESIAN_POINT ( 'NONE',  ( 8.715434833791931624, 64.46018628210146062, 8.962234695871760692 ) ) ;
#25900 = ORIENTED_EDGE ( 'NONE', *, *, #6322, .T. ) ;
#25901 = EDGE_LOOP ( 'NONE', ( #30994, #28549, #14064, #27584 ) ) ;
#25902 = CARTESIAN_POINT ( 'NONE',  ( 23.34314575050770202, -3.999999999999897859, 49.79500130984166617 ) ) ;
#25903 = ADVANCED_FACE ( 'NONE', ( #8800 ), #29248, .F. ) ;
#25904 = CARTESIAN_POINT ( 'NONE',  ( -1.909035429704832693E-15, 196.8500000012290343, -31.17691453623979214 ) ) ;
#25905 = DIRECTION ( 'NONE',  ( -0.9925324990730154395, 0.1219804832088915297, 0.000000000000000000 ) ) ;
#25906 = VECTOR ( 'NONE', #18105, 1000.000000000000000 ) ;
#25907 = CARTESIAN_POINT ( 'NONE',  ( -10.83675517735179028, 32.93981371789854506, 11.08355503943118947 ) ) ;
#25908 = CARTESIAN_POINT ( 'NONE',  ( 31.45868912971819142, 0.000000000000000000, 169.5433637710095809 ) ) ;
#25909 = CARTESIAN_POINT ( 'NONE',  ( 23.87821517812499650, 241.1593750006145171, -4.985214923628404904 ) ) ;
#25910 = VECTOR ( 'NONE', #567, 1000.000000000000000 ) ;
#25911 = CARTESIAN_POINT ( 'NONE',  ( -48.61830436395490551, 209.8844732041982297, 4.499999999999996447 ) ) ;
#25912 = CARTESIAN_POINT ( 'NONE',  ( 19.39230484541326760, 242.9486538117967029, 5.999999999999999112 ) ) ;
#25913 = CARTESIAN_POINT ( 'NONE',  ( 36.93903810116746911, 3.604726614523243278, 160.5471114303018680 ) ) ;
#25914 = CARTESIAN_POINT ( 'NONE',  ( 9.500000000000005329, 20.28981371789855004, -0.1745138560723090149 ) ) ;
#25915 = CARTESIAN_POINT ( 'NONE',  ( 0.000000000000000000, 200.0000000000000000, -27.00000000000000355 ) ) ;
#25916 = DIRECTION ( 'NONE',  ( 0.000000000000000000, 0.000000000000000000, 1.000000000000000000 ) ) ;
#25917 = CARTESIAN_POINT ( 'NONE',  ( 26.58413874528002907, 195.0000000000000000, -5.631313390073841241 ) ) ;
#25918 = CARTESIAN_POINT ( 'NONE',  ( 5.778771075727756162E-15, 196.3718750006145513, 31.45816453501075927 ) ) ;
#25919 = CARTESIAN_POINT ( 'NONE',  ( -2.908627838312453306, 133.2773137178985507, 15.53471296425188797 ) ) ;
#25920 = ORIENTED_EDGE ( 'NONE', *, *, #1357, .F. ) ;
#25921 = ADVANCED_FACE ( 'NONE', ( #6327 ), #12194, .F. ) ;
#25922 = CARTESIAN_POINT ( 'NONE',  ( 4.622313124798573369, 37.43518628210144783, 11.61527771782819940 ) ) ;
#25923 = CARTESIAN_POINT ( 'NONE',  ( 13.56230152254410370, 5.196152422706630247, -10.31249999877101331 ) ) ;
#25924 = CARTESIAN_POINT ( 'NONE',  ( 15.00000000000000000, 247.2624999999999886, -3.464101615137752610 ) ) ;
#25925 = AXIS2_PLACEMENT_3D ( 'NONE', #23045, #25877, #2751 ) ;
#25926 = CARTESIAN_POINT ( 'NONE',  ( 25.22171936664797798, 0.000000000000000000, 169.8914008901326724 ) ) ;
#25927 = CARTESIAN_POINT ( 'NONE',  ( 24.00000000000000000, -5.196152422706629359, -2.943749998770950338 ) ) ;
#25928 = CARTESIAN_POINT ( 'NONE',  ( 19.68408634441911076, 5.407089921784862696, -7.996874999385533478 ) ) ;
#25929 = CARTESIAN_POINT ( 'NONE',  ( -13.50000000000000533, 196.8875000012290286, -23.38268590217984411 ) ) ;
#25930 = CARTESIAN_POINT ( 'NONE',  ( 5.233372021372432847, 73.94768628210142936, 8.152565276336710909 ) ) ;
#25931 = DIRECTION ( 'NONE',  ( 1.000000000000000000, 0.000000000000000000, -0.000000000000000000 ) ) ;
#25932 = EDGE_CURVE ( 'NONE', #11530, #32439, #29058, .T. ) ;
#25933 = CARTESIAN_POINT ( 'NONE',  ( 12.46528703574805874, 100.3976862821014464, 2.660918448318279950 ) ) ;
#25934 = CARTESIAN_POINT ( 'NONE',  ( 16.56230152254410726, 0.000000000000000000, -10.00000000000000000 ) ) ;
#25935 = CARTESIAN_POINT ( 'NONE',  ( -3.253724281355068545E-15, 198.6500000012290172, -27.00000000000000000 ) ) ;
#25936 = ORIENTED_EDGE ( 'NONE', *, *, #10728, .F. ) ;
#25937 = CARTESIAN_POINT ( 'NONE',  ( 33.98111043944852128, -5.407089921784855591, 162.5563074099482037 ) ) ;
#25938 = CARTESIAN_POINT ( 'NONE',  ( 18.12178482187499640, 4.985214923628404904, -7.415624999385473259 ) ) ;
#25939 = CARTESIAN_POINT ( 'NONE',  ( 13.62178482187501416, 195.0593750006145513, 23.59362340125806767 ) ) ;
#25940 = CARTESIAN_POINT ( 'NONE',  ( 37.60577953318700395, 3.604726614523243278, 168.1680008707037075 ) ) ;
#25941 = CARTESIAN_POINT ( 'NONE',  ( 34.23809944139907202, 5.196152422706637353, 166.8910292673464539 ) ) ;
#25942 = CARTESIAN_POINT ( 'NONE',  ( -26.99999999999999645, 198.2375000000000114, 15.58845726811991561 ) ) ;
#25943 = CARTESIAN_POINT ( 'NONE',  ( 15.24356964374999990, 240.8593750006145342, 0.000000000000000000 ) ) ;
#25944 = CARTESIAN_POINT ( 'NONE',  ( 13.62178482187501416, 199.5031250006145456, 23.59362340125806767 ) ) ;
#25945 = CARTESIAN_POINT ( 'NONE',  ( 6.932735513424201024, 120.0523137178985564, -10.69584247140429412 ) ) ;
#25946 = CARTESIAN_POINT ( 'NONE',  ( 10.49813415415989581, 119.3726862821014549, 7.228626920339069173 ) ) ;
#25948 = ORIENTED_EDGE ( 'NONE', *, *, #34391, .F. ) ;
#25947 = EDGE_LOOP ( 'NONE', ( #9028, #23991, #25573, #35678 ) ) ;
#25949 = CARTESIAN_POINT ( 'NONE',  ( 13.62178482187499640, 199.2031250006145342, -23.59362340125807123 ) ) ;
#25950 = CARTESIAN_POINT ( 'NONE',  ( 21.00000000000000000, 243.1093750006145058, 6.646953231504538984 ) ) ;
#25951 = CARTESIAN_POINT ( 'NONE',  ( 24.00000000000000000, -5.196152422706629359, -2.549999999999996714 ) ) ;
#25952 = CARTESIAN_POINT ( 'NONE',  ( 2.908627838312458636, 101.0773137178985479, -15.53471296425188442 ) ) ;
#25953 = CARTESIAN_POINT ( 'NONE',  ( 18.12178482187499640, 4.985214923628404904, -2.578124999385478233 ) ) ;
#25954 = CIRCLE ( 'NONE', #23524, 2.649999999999992806 ) ;
#25955 = CARTESIAN_POINT ( 'NONE',  ( -26.99999999999998934, 196.1000000012290627, 15.58845726811991561 ) ) ;
#25956 = CARTESIAN_POINT ( 'NONE',  ( 8.843639120294245259, 76.06481371789855928, 3.474262827703527901 ) ) ;
#25957 = CARTESIAN_POINT ( 'NONE',  ( 22.80587116629410716, 3.604726614523238837, -3.028124999385537031 ) ) ;
#25958 = CARTESIAN_POINT ( 'NONE',  ( 23.87821517812499650, 241.0468750006145058, -4.985214923628404904 ) ) ;
#25959 = CARTESIAN_POINT ( 'NONE',  ( -7.228626920338836470, 53.92731371789854933, -10.49813415416005213 ) ) ;
#25960 = CARTESIAN_POINT ( 'NONE',  ( -29.50000000000000711, 237.0000000000000000, -2.499999999999994671 ) ) ;
#25961 = CARTESIAN_POINT ( 'NONE',  ( 4.622313124798573369, 111.0351862821014635, 11.61527771782819940 ) ) ;
#25962 = CARTESIAN_POINT ( 'NONE',  ( 10.56230152254411436, -3.464101615137757051, -2.549999998770989151 ) ) ;
#25963 = CARTESIAN_POINT ( 'NONE',  ( -38.72247103062156981, 206.6499508600178672, 5.571401726697986057 ) ) ;
#25964 = PLANE ( 'NONE',  #15551 ) ;
#25965 = CARTESIAN_POINT ( 'NONE',  ( 20.99999999999999645, 240.2125000000000057, 5.999999999999998224 ) ) ;
#25966 = CARTESIAN_POINT ( 'NONE',  ( -13.23911966647218463, 94.64768628210147483, 8.632099005475506459 ) ) ;
#25967 = CARTESIAN_POINT ( 'NONE',  ( -11.48171059495397373, 22.48518628210144499, -4.944772684328680334 ) ) ;
#25968 = DIRECTION ( 'NONE',  ( 0.000000000000000000, 1.000000000000000000, -2.710505431213758620E-16 ) ) ;
#25969 = CARTESIAN_POINT ( 'NONE',  ( 15.00000000000000178, 241.5437500012290570, 3.464101615137757051 ) ) ;
#25970 = CARTESIAN_POINT ( 'NONE',  ( -3.796722387233375073, 130.5851862821014606, 8.710071997420127943 ) ) ;
#25971 = EDGE_LOOP ( 'NONE', ( #4224, #10890, #7311, #25758 ) ) ;
#25972 = CARTESIAN_POINT ( 'NONE',  ( 37.56819361912707222, 7.646167579472015790E-16, 167.7383919071516516 ) ) ;
#25973 = CARTESIAN_POINT ( 'NONE',  ( 8.843639120294328748, 71.93518628210142651, -3.474262827703334722 ) ) ;
#25974 = DIRECTION ( 'NONE',  ( -0.000000000000000000, -0.000000000000000000, 1.000000000000000000 ) ) ;
#25975 = CARTESIAN_POINT ( 'NONE',  ( -27.24356964375001056, 194.8294844423495533, -9.915847621322177119 ) ) ;
#25977 = DIRECTION ( 'NONE',  ( 0.000000000000000000, 0.000000000000000000, -1.000000000000000000 ) ) ;
#25976 =( BOUNDED_CURVE ( )  B_SPLINE_CURVE ( 2, ( #21665, #16535, #33777, #21852, #18832, #10648, #1745, #33404, #36607 ),
 .UNSPECIFIED., .F., .F. ) 
 B_SPLINE_CURVE_WITH_KNOTS ( ( 3, 2, 2, 2, 3 ),
 ( 0.5760869565217391353, 0.5797101449275362528, 0.5869565217391304879, 0.5942028985507246119, 0.5978260869565217295 ),
 .UNSPECIFIED. ) 
 CURVE ( )  GEOMETRIC_REPRESENTATION_ITEM ( )  RATIONAL_B_SPLINE_CURVE ( ( 0.9330127018922194093, 0.9330127018922194093, 1.000000000000000000, 0.8660254037844387076, 1.000000000000000000, 0.8660254037844387076, 1.000000000000000000, 0.9330127018922194093, 0.9330127018922194093 ) ) 
 REPRESENTATION_ITEM ( '' )  );
#25978 = CARTESIAN_POINT ( 'NONE',  ( -1.926257025242585782E-15, 196.5968750006145456, -31.45816453501075927 ) ) ;
#25979 = CARTESIAN_POINT ( 'NONE',  ( -79.65000000000001990, 210.0000000000000000, 2.500000000000001332 ) ) ;
#25980 = DIRECTION ( 'NONE',  ( 0.000000000000000000, 0.000000000000000000, 1.000000000000000000 ) ) ;
#25981 = EDGE_CURVE ( 'NONE', #11631, #11055, #537, .T. ) ;
#25982 = CARTESIAN_POINT ( 'NONE',  ( -6.840914352311947333, 35.23981371789855643, -6.594114490232462877 ) ) ;
#25983 = CARTESIAN_POINT ( 'NONE',  ( 27.24356964375000700, 199.5968750006145740, 15.72908226750537075 ) ) ;
#25984 = ORIENTED_EDGE ( 'NONE', *, *, #24228, .F. ) ;
#25985 = ORIENTED_EDGE ( 'NONE', *, *, #37470, .T. ) ;
#25986 = CARTESIAN_POINT ( 'NONE',  ( 26.99999999999999645, 240.3437500012290400, 3.464101615137751278 ) ) ;
#25987 = CARTESIAN_POINT ( 'NONE',  ( 11.61527771782809637, 39.26481371789855501, 4.622313124798827388 ) ) ;
#25988 = CARTESIAN_POINT ( 'NONE',  ( 16.56230152254411436, -7.209453229046482114, -9.534374999385541116 ) ) ;
#25989 = CARTESIAN_POINT ( 'NONE',  ( 18.12178482187500350, -4.985214923628407568, -8.728124999385494576 ) ) ;
#25990 = CARTESIAN_POINT ( 'NONE',  ( 11.08355503943118769, 141.0398137178985678, 10.83675517735179028 ) ) ;
#25991 = VERTEX_POINT ( 'NONE', #34938 ) ;
#25992 = CARTESIAN_POINT ( 'NONE',  ( 22.80587116629411781, -3.604726614523238837, -3.609374999385538185 ) ) ;
#25993 = CARTESIAN_POINT ( 'NONE',  ( 27.24356964375000700, 199.0906250006145228, 15.72908226750537075 ) ) ;
#25994 = EDGE_CURVE ( 'NONE', #36517, #36421, #4416, .T. ) ;
#25995 = CARTESIAN_POINT ( 'NONE',  ( 31.17679477432231394, -7.209453229046482114, 166.3212965449812657 ) ) ;
#25996 =( BOUNDED_CURVE ( )  B_SPLINE_CURVE ( 2, ( #18243, #29787, #26563, #35845, #3818, #9141, #15011, #29214, #17677 ),
 .UNSPECIFIED., .F., .F. ) 
 B_SPLINE_CURVE_WITH_KNOTS ( ( 3, 2, 2, 2, 3 ),
 ( 0.7500000000000000000, 0.7536231884057971175, 0.7608695652173913526, 0.7681159420289854767, 0.7717391304347825942 ),
 .UNSPECIFIED. ) 
 CURVE ( )  GEOMETRIC_REPRESENTATION_ITEM ( )  RATIONAL_B_SPLINE_CURVE ( ( 0.9330127018922194093, 0.9330127018922194093, 1.000000000000000000, 0.8660254037844387076, 1.000000000000000000, 0.8660254037844387076, 1.000000000000000000, 0.9330127018922194093, 0.9330127018922194093 ) ) 
 REPRESENTATION_ITEM ( '' )  );
#25997 = CARTESIAN_POINT ( 'NONE',  ( -62.06919563604516554, 218.5000000000000000, -0.1155267958018185298 ) ) ;
#25998 = CARTESIAN_POINT ( 'NONE',  ( 26.75643035624999655, 248.2093750006145285, -3.323476615752271268 ) ) ;
#25999 = PRESENTATION_STYLE_ASSIGNMENT (( #31685 ) ) ;
#26000 = CARTESIAN_POINT ( 'NONE',  ( -18.43413144353408484, 194.9999999999999432, 19.99507324645828277 ) ) ;
#26001 = CARTESIAN_POINT ( 'NONE',  ( -51.97544563604517265, 213.3788001182224718, 3.209657149897419348 ) ) ;
#26002 = CARTESIAN_POINT ( 'NONE',  ( -44.65997103062156981, 215.5714017266979852, 3.350049139982118618 ) ) ;
#26003 = DIRECTION ( 'NONE',  ( 0.000000000000000000, 0.000000000000000000, 1.000000000000000000 ) ) ;
#26004 = EDGE_LOOP ( 'NONE', ( #9350, #37030, #7411, #32096 ) ) ;
#26005 = PLANE ( 'NONE',  #22192 ) ;
#26006 = CARTESIAN_POINT ( 'NONE',  ( 26.99999999999999645, 7.347880794884117764E-16, -6.975000000000008527 ) ) ;
#26007 = CARTESIAN_POINT ( 'NONE',  ( 8.632099005475788900, 18.85231371789855359, -13.23911966647199812 ) ) ;
#26008 = CARTESIAN_POINT ( 'NONE',  ( -59.89955436395489841, 216.3070033484980002, -6.137860380172975638 ) ) ;
#26009 = CARTESIAN_POINT ( 'NONE',  ( -12.46528703574805697, 3.797686282101447652, -2.660918448318280838 ) ) ;
#26010 = CARTESIAN_POINT ( 'NONE',  ( 11.48171059495397728, 54.68518628210144783, 4.944772684328674117 ) ) ;
#26011 = CARTESIAN_POINT ( 'NONE',  ( 10.56230152254410903, 3.464101615137757051, -4.087500000000054534 ) ) ;
#26012 = ORIENTED_EDGE ( 'NONE', *, *, #21001, .T. ) ;
#26013 = CARTESIAN_POINT ( 'NONE',  ( -42.28497103062156270, 204.4285982733020148, -3.350049139982115509 ) ) ;
#26014 = DIRECTION ( 'NONE',  ( 1.000000000000000000, 0.000000000000000000, 0.000000000000000000 ) ) ;
#26015 = VECTOR ( 'NONE', #4004, 1000.000000000000000 ) ;
#26016 = CARTESIAN_POINT ( 'NONE',  ( 27.24356964374999635, 196.0718750006145683, -15.72908226750539029 ) ) ;
#26017 = CARTESIAN_POINT ( 'NONE',  ( 28.29034631613303929, -5.196152422706632912, 167.7501794356626306 ) ) ;
#26018 = CARTESIAN_POINT ( 'NONE',  ( 13.49999999999999645, 197.5999999999999943, -23.38268590217984766 ) ) ;
#26019 = DIRECTION ( 'NONE',  ( 0.08715574274765150453, 0.000000000000000000, 0.9961946980917461003 ) ) ;
#26020 = CARTESIAN_POINT ( 'NONE',  ( 23.87821517812500005, 245.5093750006145399, 4.985214923628404016 ) ) ;
#26021 = CARTESIAN_POINT ( 'NONE',  ( 8.152565276336593669, 94.75231371789854506, 5.233372021372610483 ) ) ;
#26022 = CARTESIAN_POINT ( 'NONE',  ( 33.79360515338605353, -5.196152422706635576, 161.8104363070785041 ) ) ;
#26023 = EDGE_LOOP ( 'NONE', ( #37376, #25437, #34177, #32469 ) ) ;
#26024 = CARTESIAN_POINT ( 'NONE',  ( -57.72247103062156270, 206.6499508600178672, 5.571401726697986057 ) ) ;
#26025 = DIRECTION ( 'NONE',  ( 0.000000000000000000, 1.000000000000000000, 0.000000000000000000 ) ) ;
#26026 = CARTESIAN_POINT ( 'NONE',  ( 24.00000000000000000, 246.1562500012290400, 5.196152422706629359 ) ) ;
#26027 = VERTEX_POINT ( 'NONE', #5322 ) ;
#26028 = CARTESIAN_POINT ( 'NONE',  ( 4.622313124798831829, 101.3648137178985564, -11.61527771782809282 ) ) ;
#26029 = CARTESIAN_POINT ( 'NONE',  ( 22.80587116629412492, -3.604726614523238837, -0.4593749993855362757 ) ) ;
#26030 = CARTESIAN_POINT ( 'NONE',  ( 27.51944227705346790, -5.407089921784859143, 160.3360300724413321 ) ) ;
#26031 = CARTESIAN_POINT ( 'NONE',  ( 23.87821517812499650, 4.985214923628404904, -3.103124999385475924 ) ) ;
#26032 = CARTESIAN_POINT ( 'NONE',  ( 2.311890736173452865, 64.27731371789855075, -12.53471296425189152 ) ) ;
#26033 = CARTESIAN_POINT ( 'NONE',  ( 27.24356964374999635, 199.6718750006145058, -15.72908226750539029 ) ) ;
#26034 = VERTEX_POINT ( 'NONE', #5499 ) ;
#26035 = ORIENTED_EDGE ( 'NONE', *, *, #36935, .T. ) ;
#26036 = CIRCLE ( 'NONE', #11511, 7.500000000000000000 ) ;
#26037 = ORIENTED_EDGE ( 'NONE', *, *, #4718, .T. ) ;
#26038 = CARTESIAN_POINT ( 'NONE',  ( 26.99999999999999645, 7.347880794884117764E-16, -7.368749998770962151 ) ) ;
#26039 = CARTESIAN_POINT ( 'NONE',  ( 20.99999999999999645, 6.646953231504538984, -6.103124999385481253 ) ) ;
#26040 = LINE ( 'NONE', #31730, #23347 ) ;
#26041 =( BOUNDED_CURVE ( )  B_SPLINE_CURVE ( 3, ( #20481, #6051, #14227, #182 ),
 .UNSPECIFIED., .F., .F. ) 
 B_SPLINE_CURVE_WITH_KNOTS ( ( 4, 4 ),
 ( 3.141592653589793116, 4.712388980384648818 ),
 .UNSPECIFIED. ) 
 CURVE ( )  GEOMETRIC_REPRESENTATION_ITEM ( )  RATIONAL_B_SPLINE_CURVE ( ( 1.000000000000000000, 0.8047378541243747074, 0.8047378541243747074, 1.000000000000000000 ) ) 
 REPRESENTATION_ITEM ( '' )  );
#26042 = CARTESIAN_POINT ( 'NONE',  ( 21.00000000000000000, 247.8343750006144717, -6.646953231504538984 ) ) ;
#26043 = CARTESIAN_POINT ( 'NONE',  ( 6.932735513423970097, 37.14768628210143930, 10.69584247140445044 ) ) ;
#26044 = EDGE_CURVE ( 'NONE', #20032, #18087, #5133, .T. ) ;
#26045 = CARTESIAN_POINT ( 'NONE',  ( -51.57961230271182984, 211.8571965466040581, 6.469044688360755302 ) ) ;
#26046 = CARTESIAN_POINT ( 'NONE',  ( 16.34449471653107011, 214.6555052834990818, -4.429144169343526727 ) ) ;
#26047 = CARTESIAN_POINT ( 'NONE',  ( -44.65252896937850835, 207.6499508600178387, -3.839350919129087547 ) ) ;
#26048 = CARTESIAN_POINT ( 'NONE',  ( 33.76419009031582874, -5.196152422706629359, 161.4742205976968989 ) ) ;
#26049 = CARTESIAN_POINT ( 'NONE',  ( -2.311890736173448424, 96.47731371789855359, 12.53471296425189330 ) ) ;
#26050 = CARTESIAN_POINT ( 'NONE',  ( -54.15997103062156981, 213.8393509191290889, 2.350049139982164359 ) ) ;
#26051 = CARTESIAN_POINT ( 'NONE',  ( -40.10788769728823411, 218.4690446883607535, 2.393094931466250408 ) ) ;
#26052 = CARTESIAN_POINT ( 'NONE',  ( 20.99999999999999645, 6.646953231504538984, -5.315624999385481608 ) ) ;
#26053 = CARTESIAN_POINT ( 'NONE',  ( 13.56230152254411614, -5.196152422706632912, -4.312499998771063048 ) ) ;
#26054 = CARTESIAN_POINT ( 'NONE',  ( 14.25334919248795451, 84.11481371789855643, -6.092822981423661410 ) ) ;
#26055 = CARTESIAN_POINT ( 'NONE',  ( -54.15252896937849414, 205.6499508600178103, -7.303452534266820173 ) ) ;
#26056 = VERTEX_POINT ( 'NONE', #11384 ) ;
#26057 = CARTESIAN_POINT ( 'NONE',  ( 15.00000000000000000, 0.000000000000000000, -6.750000000000006217 ) ) ;
#26058 = CARTESIAN_POINT ( 'NONE',  ( -6.932735513423968321, 106.1476862821014606, -10.69584247140445221 ) ) ;
#26059 = CARTESIAN_POINT ( 'NONE',  ( -15.50000000000000533, 49.51018628210145067, -0.1745138560725808530 ) ) ;
#26060 = CARTESIAN_POINT ( 'NONE',  ( 19.39230484541323918, 243.1575961894323541, -5.999999999999987566 ) ) ;
#26061 = CARTESIAN_POINT ( 'NONE',  ( 33.83240095338533848, 5.407089921784862696, 160.8565502063291603 ) ) ;
#26062 =( GEOMETRIC_REPRESENTATION_CONTEXT ( 3 ) GLOBAL_UNCERTAINTY_ASSIGNED_CONTEXT ( ( #2126 ) ) GLOBAL_UNIT_ASSIGNED_CONTEXT ( ( #20862, #9662, #20668 ) ) REPRESENTATION_CONTEXT ( 'NONE', 'WORKASPACE' ) );
#26063 = CARTESIAN_POINT ( 'NONE',  ( 8.927990412390657937, 71.07268628210144357, -13.04141134922759804 ) ) ;
#26064 = CARTESIAN_POINT ( 'NONE',  ( 27.24356964375000345, 199.1281250006145171, -3.336375036156643733E-15 ) ) ;
#26065 = EDGE_CURVE ( 'NONE', #6301, #12071, #35183, .T. ) ;
#26066 = CARTESIAN_POINT ( 'NONE',  ( 22.80587116629410716, 7.646167579472015790E-16, -9.815624999385569538 ) ) ;
#26067 = LINE ( 'NONE', #20397, #13440 ) ;
#26068 = CARTESIAN_POINT ( 'NONE',  ( -54.95163769728823411, 215.6869285224996986, -3.149950860017881382 ) ) ;
#26069 = CARTESIAN_POINT ( 'NONE',  ( 13.62844269029146638, 5.304656780843813202, -10.00000000000000000 ) ) ;
#26070 = CARTESIAN_POINT ( 'NONE',  ( -11.61527771782819940, 39.73518628210144499, 4.622313124798574258 ) ) ;
#26071 = CARTESIAN_POINT ( 'NONE',  ( 27.24356964375000700, 199.5968750006145456, 15.72908226750537075 ) ) ;
#26072 = DIRECTION ( 'NONE',  ( -5.782411586589356653E-16, 0.000000000000000000, -1.000000000000000000 ) ) ;
#26073 = CARTESIAN_POINT ( 'NONE',  ( 7.954856959092191815, 8.972686282101431487, 5.529263428287477744 ) ) ;
#26074 = CARTESIAN_POINT ( 'NONE',  ( 23.87821517812499650, 247.9093750006145171, -4.985214923628404904 ) ) ;
#26075 = VERTEX_POINT ( 'NONE', #13868 ) ;
#26076 = CARTESIAN_POINT ( 'NONE',  ( 15.00000000000000000, 3.464101615137752166, -4.087499999999990585 ) ) ;
#26077 = CARTESIAN_POINT ( 'NONE',  ( -47.00000000000000711, 244.5000000000000000, -5.000000000000001776 ) ) ;
#26078 = DIRECTION ( 'NONE',  ( 1.000000000000000000, 0.000000000000000000, 0.000000000000000000 ) ) ;
#26079 = CARTESIAN_POINT ( 'NONE',  ( 19.68408634441910365, -5.407089921784855591, -5.390624999385557281 ) ) ;
#26080 = CARTESIAN_POINT ( 'NONE',  ( 37.45380170677077558, 3.604726614523238837, 166.4308863659062183 ) ) ;
#26081 = CARTESIAN_POINT ( 'NONE',  ( 15.00000000000000178, 241.4874999999999829, 3.464101615137757051 ) ) ;
#26082 = CARTESIAN_POINT ( 'NONE',  ( 15.00000000000027711, 3.464101615137910706, -0.8812499987709506710 ) ) ;
#26083 = CARTESIAN_POINT ( 'NONE',  ( 4.944772684328679446, 70.78518628210144925, -11.48171059495397373 ) ) ;
#26084 = ORIENTED_EDGE ( 'NONE', *, *, #8485, .T. ) ;
#26085 = VERTEX_POINT ( 'NONE', #8728 ) ;
#26086 = CARTESIAN_POINT ( 'NONE',  ( 30.61545731874177534, -6.928203230275506996, 159.9051800681962732 ) ) ;
#26087 = CARTESIAN_POINT ( 'NONE',  ( -1.909035429704832693E-15, 195.0500000012290229, -31.17691453623979214 ) ) ;
#26088 = DIRECTION ( 'NONE',  ( 0.08715574274765150453, 0.000000000000000000, 0.9961946980917461003 ) ) ;
#26089 = CARTESIAN_POINT ( 'NONE',  ( 26.75643035624999655, -3.323476615752267715, -6.703124999385464911 ) ) ;
#26090 = CARTESIAN_POINT ( 'NONE',  ( -14.25334919248795096, 33.51481371789854791, 6.092822981423662299 ) ) ;
#26091 = CARTESIAN_POINT ( 'NONE',  ( 24.00000000000000000, -5.196152422706629359, -5.193749998770952558 ) ) ;
#26092 = CARTESIAN_POINT ( 'NONE',  ( 15.24356964374999990, 240.4093750006145456, 0.000000000000000000 ) ) ;
#26093 = AXIS2_PLACEMENT_3D ( 'NONE', #14591, #28794, #37142 ) ;
#26094 = CARTESIAN_POINT ( 'NONE',  ( -45.05580436395490551, 214.5000000000000284, 0.1155267958017899832 ) ) ;
#26095 = DIRECTION ( 'NONE',  ( -0.000000000000000000, 1.000000000000000000, -0.000000000000000000 ) ) ;
#26096 = CARTESIAN_POINT ( 'NONE',  ( 25.37039736927157563, 3.464101615137752166, 168.7961499886528713 ) ) ;
#26097 = CARTESIAN_POINT ( 'NONE',  ( -7.954856959092309943, 24.02731371789854364, 5.529263428287300108 ) ) ;
#26098 = CARTESIAN_POINT ( 'NONE',  ( -57.32663769728823411, 204.3130714775002730, 3.149950860017883603 ) ) ;
#26099 = DIRECTION ( 'NONE',  ( 0.000000000000000000, 0.000000000000000000, 1.000000000000000000 ) ) ;
#26100 = CARTESIAN_POINT ( 'NONE',  ( 21.00000000000000355, 0.000000000000000000, 50.00000000000001421 ) ) ;
#26101 = CARTESIAN_POINT ( 'NONE',  ( -27.24356964375000345, 194.9093750006145456, 0.000000000000000000 ) ) ;
#26102 = CARTESIAN_POINT ( 'NONE',  ( -13.23911966647199812, 126.9523137178985621, -8.632099005475788900 ) ) ;
#26103 = EDGE_LOOP ( 'NONE', ( #20714, #34914, #20336, #14449, #11606, #17488 ) ) ;
#26104 = CARTESIAN_POINT ( 'NONE',  ( -8.962234695871760692, 39.16018628210144215, 8.715434833791933400 ) ) ;
#26105 = CARTESIAN_POINT ( 'NONE',  ( 15.52041685288908823, 5.908847293266075162, -10.33697644040032060 ) ) ;
#26106 = CARTESIAN_POINT ( 'NONE',  ( 1.069080835302379631E-14, 199.2125000000000057, 27.00000000000000000 ) ) ;
#26107 = CARTESIAN_POINT ( 'NONE',  ( 38.17292378879935200, 7.686353184319896670, 158.6719570163914170 ) ) ;
#26108 = CARTESIAN_POINT ( 'NONE',  ( 24.00000000000000000, -5.196152422706629359, -2.493749998770944387 ) ) ;
#26109 = CARTESIAN_POINT ( 'NONE',  ( 10.31873187879410381, 0.000000000000000000, -9.646874999385518734 ) ) ;
#26110 = FACE_OUTER_BOUND ( 'NONE', #2901, .T. ) ;
#26111 = CARTESIAN_POINT ( 'NONE',  ( -0.1745138560725182642, 84.01018628210145778, 9.500000000000005329 ) ) ;
#26112 = CARTESIAN_POINT ( 'NONE',  ( 20.99999999999999645, 249.6625000000000512, 5.999999999999998224 ) ) ;
#26113 = FACE_OUTER_BOUND ( 'NONE', #30049, .T. ) ;
#26114 = CARTESIAN_POINT ( 'NONE',  ( -12.50000000000000355, 86.31018628210145494, -0.1745138560725492671 ) ) ;
#26115 = DIRECTION ( 'NONE',  ( -0.000000000000000000, -1.000000000000000000, -0.000000000000000000 ) ) ;
#26116 = CARTESIAN_POINT ( 'NONE',  ( 13.49999999999999645, 198.6125000012290513, -23.38268590217984766 ) ) ;
#26117 = ORIENTED_EDGE ( 'NONE', *, *, #12493, .F. ) ;
#26118 = CARTESIAN_POINT ( 'NONE',  ( 36.94067227134398479, 7.646167579472015790E-16, 160.5657900808910767 ) ) ;
#26119 = CARTESIAN_POINT ( 'NONE',  ( 18.12178482187500350, -4.985214923628407568, -8.165624999385473259 ) ) ;
#26120 = CARTESIAN_POINT ( 'NONE',  ( 27.24356964375000700, 195.0968750006145456, 15.72908226750537075 ) ) ;
#26121 = CARTESIAN_POINT ( 'NONE',  ( 24.98966720158235688, -3.604726614523244610, 167.2390325064633885 ) ) ;
#26122 = CARTESIAN_POINT ( 'NONE',  ( 34.12043918868973691, 5.196152422706637353, 165.5461664249225748 ) ) ;
#26123 = CARTESIAN_POINT ( 'NONE',  ( 10.56230152254410903, 7.347880794884117764E-16, -10.00000000000000000 ) ) ;
#26124 = CARTESIAN_POINT ( 'NONE',  ( 26.99999999999999645, 248.8750000000000000, -7.347880794884117764E-16 ) ) ;
#26125 = CARTESIAN_POINT ( 'NONE',  ( -27.24356964374999279, 198.9406250006145171, 15.72908226750539384 ) ) ;
#26126 = CARTESIAN_POINT ( 'NONE',  ( 10.69584247140429589, 113.1523137178985650, 6.932735513424201024 ) ) ;
#26127 = CARTESIAN_POINT ( 'NONE',  ( -10.49813415415989404, 123.9726862821014493, -7.228626920339069173 ) ) ;
#26129 = ORIENTED_EDGE ( 'NONE', *, *, #13142, .F. ) ;
#26128 = ORIENTED_EDGE ( 'NONE', *, *, #8236, .F. ) ;
#26130 = B_SPLINE_CURVE_WITH_KNOTS ( 'NONE', 3,
 ( #15112, #29318, #884, #29696, #29125, #6393, #18340, #17775 ),
 .UNSPECIFIED., .F., .F.,
 ( 4, 2, 2, 4 ),
 ( 0.000000000000000000, 0.002520245793383945297, 0.003780368690075958278, 0.005040491586767971259 ),
 .UNSPECIFIED. ) ;
#26131 = CARTESIAN_POINT ( 'NONE',  ( 27.24356964375000700, 199.0906250006145228, 15.72908226750537075 ) ) ;
#26132 = CARTESIAN_POINT ( 'NONE',  ( 21.00000000000000000, 241.7593750006145115, 6.646953231504538984 ) ) ;
#26133 = CARTESIAN_POINT ( 'NONE',  ( -15.46528703574811736, 89.00231371789853085, 3.257655550456946436 ) ) ;
#26134 = CARTESIAN_POINT ( 'NONE',  ( 15.24356964375000167, -3.323476615752272600, -4.715624999385497063 ) ) ;
#26135 = CARTESIAN_POINT ( 'NONE',  ( 21.00000000000000000, 247.0468750006145058, -6.646953231504538984 ) ) ;
#26136 = CARTESIAN_POINT ( 'NONE',  ( 13.49999999999999645, 197.7125000012290172, -23.38268590217984766 ) ) ;
#26137 = ADVANCED_FACE ( 'NONE', ( #28991 ), #2293, .F. ) ;
#26138 = CARTESIAN_POINT ( 'NONE',  ( 6.840914352311949109, 67.43981371789855928, 6.594114490232462877 ) ) ;
#26139 = CARTESIAN_POINT ( 'NONE',  ( 16.56230152254411436, 7.209453229046475009, -2.053124999385520066 ) ) ;
#26140 = EDGE_CURVE ( 'NONE', #32302, #34717, #18728, .T. ) ;
#26141 = CARTESIAN_POINT ( 'NONE',  ( 20.99999999999999645, 242.6593750006145171, 6.646953231504538984 ) ) ;
#26142 = CARTESIAN_POINT ( 'NONE',  ( -10.49813415416004858, 42.42731371789855643, 7.228626920338839135 ) ) ;
#26143 = CARTESIAN_POINT ( 'NONE',  ( 36.87370277765395343, -3.464101615137444412, 162.5949735130561749 ) ) ;
#26144 = CARTESIAN_POINT ( 'NONE',  ( 10.49813415415989581, 100.9726862821014635, 7.228626920339068285 ) ) ;
#26145 = CARTESIAN_POINT ( 'NONE',  ( 10.56230152254411081, 0.000000000000000000, -4.837499998771033205 ) ) ;
#26146 = EDGE_CURVE ( 'NONE', #24049, #15843, #6414, .T. ) ;
#26147 = CARTESIAN_POINT ( 'NONE',  ( -66.43080436395490551, 205.4999999999999716, -0.1155267958017894420 ) ) ;
#26148 = DIRECTION ( 'NONE',  ( 0.9961946980917462113, 0.000000000000000000, -0.08715574274765118534 ) ) ;
#26149 = CARTESIAN_POINT ( 'NONE',  ( -27.00000000000000355, 198.7250000012290343, -15.58845726811989429 ) ) ;
#26150 = CARTESIAN_POINT ( 'NONE',  ( -14.38691631536207183, 94.93518628210146915, 5.770363421893814682 ) ) ;
#26151 = CARTESIAN_POINT ( 'NONE',  ( -8.962234695871760692, 11.56018628210145316, 8.715434833791933400 ) ) ;
#26152 = CARTESIAN_POINT ( 'NONE',  ( 36.90965452142909697, 3.464101615138126977, 163.0059038247948422 ) ) ;
#26153 = DIRECTION ( 'NONE',  ( 0.000000000000000000, 0.000000000000000000, 1.000000000000000000 ) ) ;
#26154 = CARTESIAN_POINT ( 'NONE',  ( 8.710071997420127943, 128.2851862821014493, 3.796722387233375073 ) ) ;
#26155 = LINE ( 'NONE', #2478, #11248 ) ;
#26156 = CARTESIAN_POINT ( 'NONE',  ( 15.24356964374999990, 242.0593750006145513, -3.323476615752268604 ) ) ;
#26157 = VERTEX_POINT ( 'NONE', #5685 ) ;
#26158 = DIRECTION ( 'NONE',  ( -0.000000000000000000, -1.000000000000000000, -0.000000000000000000 ) ) ;
#26159 = CARTESIAN_POINT ( 'NONE',  ( -6.594114490232312775, 69.06018628210144072, -6.840914352312096547 ) ) ;
#26160 = CARTESIAN_POINT ( 'NONE',  ( 21.00000000000000000, -6.646953231504538984, -1.378124999385478056 ) ) ;
#26161 = CARTESIAN_POINT ( 'NONE',  ( 20.99999999999999645, 247.8624999999999545, 5.999999999999998224 ) ) ;
#26162 = CARTESIAN_POINT ( 'NONE',  ( 2.999999999999997335, 244.5000000000000000, 5.000000000000000000 ) ) ;
#26163 = CARTESIAN_POINT ( 'NONE',  ( 27.24356964375000700, 195.9968750006145513, 15.72908226750537075 ) ) ;
#26164 = CARTESIAN_POINT ( 'NONE',  ( 3.306246199927494800, 194.9999999999999716, 27.04578575729343726 ) ) ;
#26165 = CARTESIAN_POINT ( 'NONE',  ( -27.00000000000000355, 196.9250000012290229, -15.58845726811989429 ) ) ;
#26166 = CARTESIAN_POINT ( 'NONE',  ( -2.064181346179062349, 45.30231371789854933, -9.465287035748106703 ) ) ;
#26167 = CARTESIAN_POINT ( 'NONE',  ( -27.24356964375000345, 199.8218750006145399, -15.72908226750537786 ) ) ;
#26168 = VERTEX_POINT ( 'NONE', #17269 ) ;
#26169 = ORIENTED_EDGE ( 'NONE', *, *, #34842, .T. ) ;
#26170 = CARTESIAN_POINT ( 'NONE',  ( 26.99999999999999645, 239.9687500012290684, -3.464101615137755275 ) ) ;
#26171 = CARTESIAN_POINT ( 'NONE',  ( -4.944772684328424539, 35.81481371789854506, -11.48171059495408031 ) ) ;
#26172 = CARTESIAN_POINT ( 'NONE',  ( 16.56230152254411436, 7.209453229046482114, -7.959374999385476102 ) ) ;
#26173 = CARTESIAN_POINT ( 'NONE',  ( 15.24356964374999990, 0.000000000000000000, -10.15312499938547575 ) ) ;
#26174 = CARTESIAN_POINT ( 'NONE',  ( 4.622313124798831829, 18.56481371789855928, -11.61527771782809282 ) ) ;
#26175 = VERTEX_POINT ( 'NONE', #25785 ) ;
#26176 = CARTESIAN_POINT ( 'NONE',  ( 16.56230152254411436, -7.209453229046482114, -2.784374999385508698 ) ) ;
#26177 = CARTESIAN_POINT ( 'NONE',  ( 27.24356964374999635, 198.2656250006145058, -15.72908226750539029 ) ) ;
#26178 = CARTESIAN_POINT ( 'NONE',  ( 37.48158259977161322, -3.604726614523238837, 166.7484234259230220 ) ) ;
#26179 = CARTESIAN_POINT ( 'NONE',  ( -33.17336230271182984, 215.6869285224997270, 3.149950860017831200 ) ) ;
#26180 = CARTESIAN_POINT ( 'NONE',  ( 23.87821517812499650, 248.6968750006145115, -4.985214923628404904 ) ) ;
#26181 = CARTESIAN_POINT ( 'NONE',  ( -26.74238012849437141, 194.9999999999999432, -4.224268460287527560 ) ) ;
#26182 = CARTESIAN_POINT ( 'NONE',  ( -53.75669563604516554, 209.8844732041982297, -4.499999999999996447 ) ) ;
#26183 = CARTESIAN_POINT ( 'NONE',  ( -35.15997103062156270, 215.5714017266979852, 3.350049139982118618 ) ) ;
#26184 = CARTESIAN_POINT ( 'NONE',  ( 31.35818766391586365, 7.209453229046475009, 168.3946267603846820 ) ) ;
#26185 = VERTEX_POINT ( 'NONE', #17454 ) ;
#26186 = CARTESIAN_POINT ( 'NONE',  ( 26.97716818855048260, 0.000000000000000000, 49.47706554351410801 ) ) ;
#26187 = FACE_OUTER_BOUND ( 'NONE', #10505, .T. ) ;
#26188 = CARTESIAN_POINT ( 'NONE',  ( 3.257655550456945548, 22.30231371789854933, 15.46528703574811736 ) ) ;
#26189 = CARTESIAN_POINT ( 'NONE',  ( -57.92038769728823411, 207.6069050685337913, 8.469044688360781947 ) ) ;
#26190 = CARTESIAN_POINT ( 'NONE',  ( 11.61527771782819940, 7.535186282101452804, -4.622313124798573369 ) ) ;
#26191 =( BOUNDED_CURVE ( )  B_SPLINE_CURVE ( 2, ( #35140, #17917, #34411, #8450, #2935, #14504, #20392, #26060, #20018 ),
 .UNSPECIFIED., .F., .F. ) 
 B_SPLINE_CURVE_WITH_KNOTS ( ( 3, 2, 2, 2, 3 ),
 ( 0.6413043478260869179, 0.6449275362318840354, 0.6521739130434782705, 0.6594202898550725056, 0.6630434782608695121 ),
 .UNSPECIFIED. ) 
 CURVE ( )  GEOMETRIC_REPRESENTATION_ITEM ( )  RATIONAL_B_SPLINE_CURVE ( ( 0.9330127018922194093, 0.9330127018922194093, 1.000000000000000000, 0.8660254037844387076, 1.000000000000000000, 0.8660254037844387076, 1.000000000000000000, 0.9330127018922202975, 0.9330127018922192983 ) ) 
 REPRESENTATION_ITEM ( '' )  );
#26192 = CARTESIAN_POINT ( 'NONE',  ( 12.53471296425194836, 44.62268628210144783, -2.311890736173178418 ) ) ;
#26193 = CARTESIAN_POINT ( 'NONE',  ( 16.56230152254411436, -6.928203230275514990, -4.837499999999994138 ) ) ;
#26194 = ORIENTED_EDGE ( 'NONE', *, *, #8768, .T. ) ;
#26195 = CARTESIAN_POINT ( 'NONE',  ( -44.65997103062156981, 215.5714017266979852, 3.350049139982118618 ) ) ;
#26196 = CARTESIAN_POINT ( 'NONE',  ( 27.00000000000000355, 195.2750000000000057, -3.306546357697854128E-15 ) ) ;
#26197 = CARTESIAN_POINT ( 'NONE',  ( 13.62178482187499640, 195.2093750006145569, -23.59362340125807123 ) ) ;
#26198 = CARTESIAN_POINT ( 'NONE',  ( 13.56230152254410726, 5.196152422706636465, -6.375000000000019540 ) ) ;
#26199 = AXIS2_PLACEMENT_3D ( 'NONE', #27234, #1821, #16429 ) ;
#26200 = CARTESIAN_POINT ( 'NONE',  ( 27.00000000000000355, 196.2875000012290343, -3.306546357697854128E-15 ) ) ;
#26201 = CARTESIAN_POINT ( 'NONE',  ( -4.694659320240884604E-14, 197.4124999999999943, 27.00000000000000000 ) ) ;
#26202 = CARTESIAN_POINT ( 'NONE',  ( 21.00000000000000355, 0.000000000000000000, 50.00000000000001421 ) ) ;
#26203 = CARTESIAN_POINT ( 'NONE',  ( 26.75643035624999655, 244.6843750006145228, -7.049594010296217766E-16 ) ) ;
#26204 = CARTESIAN_POINT ( 'NONE',  ( 1.715153634034445762, 91.87731371789854506, -9.534712964251895073 ) ) ;
#26205 = CARTESIAN_POINT ( 'NONE',  ( 27.80990028412949755, -5.196152422706638241, 162.2586561612075116 ) ) ;
#26206 = ORIENTED_EDGE ( 'NONE', *, *, #29259, .F. ) ;
#26207 = CARTESIAN_POINT ( 'NONE',  ( -59.89955436395490551, 214.8429017333601792, -4.673758765035196383 ) ) ;
#26208 = CARTESIAN_POINT ( 'NONE',  ( -70.80918835584510873, 215.2843023367891249, 7.500000000000000000 ) ) ;
#26209 = CARTESIAN_POINT ( 'NONE',  ( 26.99999999999999645, 247.5437500012290570, 3.464101615137751278 ) ) ;
#26210 = CARTESIAN_POINT ( 'NONE',  ( -11.48171059495408208, 107.1148137178985564, 4.944772684328421875 ) ) ;
#26211 = CARTESIAN_POINT ( 'NONE',  ( 10.31873187879410736, -3.604726614523244610, -1.509374999385515670 ) ) ;
#26212 = CARTESIAN_POINT ( 'NONE',  ( 21.00000000000000000, -6.646953231504538984, -1.040624999385473481 ) ) ;
#26213 = CARTESIAN_POINT ( 'NONE',  ( -4.944772684328424539, 72.61481371789855643, -11.48171059495408031 ) ) ;
#26214 = CARTESIAN_POINT ( 'NONE',  ( 5.778771075727756162E-15, 198.6218750006145513, 31.45816453501075927 ) ) ;
#26215 = ORIENTED_EDGE ( 'NONE', *, *, #26724, .T. ) ;
#26216 = VERTEX_POINT ( 'NONE', #16898 ) ;
#26217 =( BOUNDED_CURVE ( )  B_SPLINE_CURVE ( 2, ( #5713, #11225, #22795, #34346, #8015, #33975, #17108 ),
 .UNSPECIFIED., .F., .F. ) 
 B_SPLINE_CURVE_WITH_KNOTS ( ( 3, 2, 2, 3 ),
 ( 0.000000000000000000, 0.007246376811594271508, 0.01449275362318854302, 0.02173913043478281626 ),
 .UNSPECIFIED. ) 
 CURVE ( )  GEOMETRIC_REPRESENTATION_ITEM ( )  RATIONAL_B_SPLINE_CURVE ( ( 1.000000000000000000, 0.8660254037844387076, 1.000000000000000000, 0.8660254037844387076, 1.000000000000000000, 0.8660254037844348218, 1.000000000000003775 ) ) 
 REPRESENTATION_ITEM ( '' )  );
#26218 = ORIENTED_EDGE ( 'NONE', *, *, #34228, .T. ) ;
#26219 = CARTESIAN_POINT ( 'NONE',  ( 15.24356964375000167, -3.323476615752272600, -4.603124999385474148 ) ) ;
#26220 = CARTESIAN_POINT ( 'NONE',  ( -26.99999999999999645, 195.5374999999999943, 15.58845726811991561 ) ) ;
#26221 = CARTESIAN_POINT ( 'NONE',  ( 15.24356964374999990, 247.0468750006145058, 0.000000000000000000 ) ) ;
#26222 = CARTESIAN_POINT ( 'NONE',  ( 12.53471296425194836, 35.42268628210144499, -2.311890736173178418 ) ) ;
#26223 = CARTESIAN_POINT ( 'NONE',  ( -50.19419563604517265, 203.5000000000000000, 0.1155267958017914542 ) ) ;
#26224 = CARTESIAN_POINT ( 'NONE',  ( 16.85147890419441197, 211.5556954109263756, -5.808099892140870857 ) ) ;
#26225 = CARTESIAN_POINT ( 'NONE',  ( -31.78794563604516910, 206.7903428501025758, 3.378800118222471838 ) ) ;
#26226 = CARTESIAN_POINT ( 'NONE',  ( 24.82131618996136879, 3.464101615137752166, 162.5201233906748541 ) ) ;
#26227 = CARTESIAN_POINT ( 'NONE',  ( 8.962234695871567070, 104.2398137178985564, 8.715434833792127023 ) ) ;
#26228 = CARTESIAN_POINT ( 'NONE',  ( -54.55580436395489841, 214.5000000000000284, 0.1155267958017899832 ) ) ;
#26229 = CARTESIAN_POINT ( 'NONE',  ( -49.40997103062157692, 217.3034525342668815, 4.350049139982096413 ) ) ;
#26230 = CARTESIAN_POINT ( 'NONE',  ( 15.24356964374999990, 3.323476615752268604, -4.340624999385463312 ) ) ;
#26231 = DIRECTION ( 'NONE',  ( 0.000000000000000000, 0.000000000000000000, -1.000000000000000000 ) ) ;
#26232 = CARTESIAN_POINT ( 'NONE',  ( 11.08355503943118769, 76.63981371789854791, 10.83675517735179028 ) ) ;
#26233 = CARTESIAN_POINT ( 'NONE',  ( -53.55877896937850124, 212.1620413398627534, -8.530955311639255356 ) ) ;
#26234 = VERTEX_POINT ( 'NONE', #28437 ) ;
#26235 = DIRECTION ( 'NONE',  ( 0.000000000000000000, 0.000000000000000000, 1.000000000000000000 ) ) ;
#26236 = CARTESIAN_POINT ( 'NONE',  ( -0.1745138560725500443, 102.4101862821014493, 12.50000000000000355 ) ) ;
#26237 = CARTESIAN_POINT ( 'NONE',  ( 6.092822981423978490, 52.38518628210145778, -14.25334919248782306 ) ) ;
#26238 = DIRECTION ( 'NONE',  ( 1.000000000000000000, 0.000000000000000000, 0.000000000000000000 ) ) ;
#26239 = AXIS2_PLACEMENT_3D ( 'NONE', #26576, #6307, #6686 ) ;
#26240 =( REPRESENTATION_RELATIONSHIP ('NONE','NONE', #4304, #9842 ) REPRESENTATION_RELATIONSHIP_WITH_TRANSFORMATION ( #7329 )SHAPE_REPRESENTATION_RELATIONSHIP( ) );
#26241 = CARTESIAN_POINT ( 'NONE',  ( 33.93698784468253393, -5.407089921784861808, 162.0519838440392562 ) ) ;
#26242 = CARTESIAN_POINT ( 'NONE',  ( 11.08355503943142750, 71.36018628210143788, -10.83675517735155225 ) ) ;
#26243 = DIRECTION ( 'NONE',  ( 0.000000000000000000, 0.000000000000000000, 1.000000000000000000 ) ) ;
#26244 = CARTESIAN_POINT ( 'NONE',  ( 19.68408634441910365, 5.407089921784857367, -9.290624999385570959 ) ) ;
#26245 = CARTESIAN_POINT ( 'NONE',  ( -45.25372103062155560, 216.5309553116391612, -1.626142955000564383 ) ) ;
#26246 = EDGE_CURVE ( 'NONE', #34698, #7963, #26155, .T. ) ;
#26247 = CARTESIAN_POINT ( 'NONE',  ( 7.234628195640363302, 195.8174038105676402, -26.99999999999996803 ) ) ;
#26248 = CARTESIAN_POINT ( 'NONE',  ( 7.228626920339068285, 43.47268628210144925, -10.49813415415989581 ) ) ;
#26249 = CARTESIAN_POINT ( 'NONE',  ( -13.62178482187500528, 199.7843750006145456, -23.59362340125807123 ) ) ;
#26250 = CARTESIAN_POINT ( 'NONE',  ( 18.00000000000000000, 5.196152422706630247, -7.668749998770957532 ) ) ;
#26251 = CARTESIAN_POINT ( 'NONE',  ( -8.152565276336710909, 11.84768628210144747, 5.233372021372435512 ) ) ;
#26252 = CARTESIAN_POINT ( 'NONE',  ( 18.12178482187500350, 246.7843750006145456, 4.985214923628407568 ) ) ;
#26253 = ORIENTED_EDGE ( 'NONE', *, *, #6109, .F. ) ;
#26254 = CARTESIAN_POINT ( 'NONE',  ( 26.99999999999999645, 3.464101615137755275, -4.237500000000010481 ) ) ;
#26255 =( BOUNDED_CURVE ( )  B_SPLINE_CURVE ( 2, ( #1405, #36087, #10131, #33254, #16203, #8409, #11244, #31891, #2342 ),
 .UNSPECIFIED., .F., .F. ) 
 B_SPLINE_CURVE_WITH_KNOTS ( ( 3, 2, 2, 2, 3 ),
 ( 0.1458333333333333426, 0.1527777777777777901, 0.1666666666666666574, 0.1805555555555555525, 0.1875000000000000000 ),
 .UNSPECIFIED. ) 
 CURVE ( )  GEOMETRIC_REPRESENTATION_ITEM ( )  RATIONAL_B_SPLINE_CURVE ( ( 0.9330127018922194093, 0.9330127018922194093, 1.000000000000000000, 0.8660254037844387076, 1.000000000000000000, 0.8660254037844387076, 1.000000000000000000, 0.9330127018922194093, 0.9330127018922194093 ) ) 
 REPRESENTATION_ITEM ( '' )  );
#26256 = CARTESIAN_POINT ( 'NONE',  ( 6.225801843091343102, 50.65819137209577150, -3.000000000000000000 ) ) ;
#26257 = CARTESIAN_POINT ( 'NONE',  ( 22.80587116629410716, 7.646167579472015790E-16, -5.315624999385537564 ) ) ;
#26258 = CARTESIAN_POINT ( 'NONE',  ( 37.44726502606470575, -3.604726614523235284, 166.3561717635493835 ) ) ;
#26259 = CARTESIAN_POINT ( 'NONE',  ( 23.99999999999999645, 241.7500000000000000, -5.196152422706631135 ) ) ;
#26260 = CARTESIAN_POINT ( 'NONE',  ( -27.00000000000000355, 198.6500000000000341, 0.000000000000000000 ) ) ;
#26261 = VECTOR ( 'NONE', #20940, 1000.000000000000000 ) ;
#26262 = EDGE_CURVE ( 'NONE', #6369, #13208, #22587, .T. ) ;
#26263 = CARTESIAN_POINT ( 'NONE',  ( -10.49813415415989404, 68.77268628210144641, -7.228626920339069173 ) ) ;
#26264 = ORIENTED_EDGE ( 'NONE', *, *, #1506, .F. ) ;
#26265 = ORIENTED_EDGE ( 'NONE', *, *, #7799, .F. ) ;
#26266 = DIRECTION ( 'NONE',  ( -1.000000000000000000, -6.123233995736766036E-17, 0.000000000000000000 ) ) ;
#26267 = CARTESIAN_POINT ( 'NONE',  ( 22.56230152254412147, 7.347880794884125653E-16, -3.825000000000050804 ) ) ;
#26268 = CARTESIAN_POINT ( 'NONE',  ( 15.24356964374999990, 0.000000000000000000, -5.990624999385463667 ) ) ;
#26269 = PRODUCT_DEFINITION_CONTEXT ( 'detailed design', #28197, 'design' ) ;
#26270 = CARTESIAN_POINT ( 'NONE',  ( 6.092822981423662299, 31.21481371789855430, 14.25334919248795096 ) ) ;
#26271 = CARTESIAN_POINT ( 'NONE',  ( 22.56230152254412147, 7.347880794884125653E-16, -4.275000000000028777 ) ) ;
#26272 = EDGE_CURVE ( 'NONE', #31540, #22269, #1539, .T. ) ;
#26273 = CARTESIAN_POINT ( 'NONE',  ( 15.24356964375000167, 239.9968750006145513, 3.323476615752272600 ) ) ;
#26274 = CARTESIAN_POINT ( 'NONE',  ( -63.05877896937850835, 211.0902445701383101, -4.530955311639234040 ) ) ;
#26275 = EDGE_CURVE ( 'NONE', #24633, #16958, #36623, .T. ) ;
#26276 = CARTESIAN_POINT ( 'NONE',  ( 26.99999999999999289, 0.000000000000000000, -8.000000000000000000 ) ) ;
#26277 = CARTESIAN_POINT ( 'NONE',  ( 34.35249135386247588, -5.196152422706629359, 168.1985348098161808 ) ) ;
#26278 = CARTESIAN_POINT ( 'NONE',  ( 8.843639120294245259, 20.86481371789854578, 3.474262827703527901 ) ) ;
#26279 = CARTESIAN_POINT ( 'NONE',  ( -65.63913769728823411, 206.8500491399821044, -5.686928522499717253 ) ) ;
#26280 = CARTESIAN_POINT ( 'NONE',  ( -37.32961230271184405, 212.3930949314663792, 8.469044688360751749 ) ) ;
#26281 = APPLICATION_PROTOCOL_DEFINITION ( 'draft international standard', 'automotive_design', 1998, #23111 ) ;
#26282 = CARTESIAN_POINT ( 'NONE',  ( 21.40987794368840014, 195.0000000000000000, -16.52969473239648224 ) ) ;
#26283 = CARTESIAN_POINT ( 'NONE',  ( 5.778771075727756162E-15, 195.9218750006145342, 31.45816453501075927 ) ) ;
#26284 = CIRCLE ( 'NONE', #34161, 7.500000000000000000 ) ;
#26285 = CARTESIAN_POINT ( 'NONE',  ( -15.53471296425188442, 126.3773137178985309, -2.908627838312459080 ) ) ;
#26286 = ORIENTED_EDGE ( 'NONE', *, *, #33781, .F. ) ;
#26287 = CARTESIAN_POINT ( 'NONE',  ( -2.660918448318275509, 47.49768628210144783, 12.46528703574805874 ) ) ;
#26288 = LINE ( 'NONE', #23455, #24419 ) ;
#26289 = CARTESIAN_POINT ( 'NONE',  ( 34.45992230116843302, 5.407089921784862696, 168.0291520325897636 ) ) ;
#26290 = CARTESIAN_POINT ( 'NONE',  ( 26.99999999999999645, 7.347880794884117764E-16, -1.518749998770940746 ) ) ;
#26291 = CARTESIAN_POINT ( 'NONE',  ( 16.56230152254411436, -7.209453229046482114, -9.984374999385536853 ) ) ;
#26292 = CARTESIAN_POINT ( 'NONE',  ( 19.68408634441910721, -5.407089921784855591, -2.690624999385549110 ) ) ;
#26293 = CARTESIAN_POINT ( 'NONE',  ( 7.954856959092191815, 54.97268628210144215, 5.529263428287477744 ) ) ;
#26294 = LINE ( 'NONE', #37475, #27357 ) ;
#26295 = CARTESIAN_POINT ( 'NONE',  ( 20.99999999999999645, 0.000000000000000000, -8.000000000000000000 ) ) ;
#26296 = CARTESIAN_POINT ( 'NONE',  ( 8.715434833791931624, 101.2601862821014578, 8.962234695871760692 ) ) ;
#26297 = CARTESIAN_POINT ( 'NONE',  ( 1.069080835302379631E-14, 195.2750000012290457, 27.00000000000000000 ) ) ;
#26298 = ORIENTED_EDGE ( 'NONE', *, *, #16382, .F. ) ;
#26299 = CARTESIAN_POINT ( 'NONE',  ( 24.44548853280171130, -3.604726614523240613, 161.0190418602530258 ) ) ;
#26300 = CARTESIAN_POINT ( 'NONE',  ( 15.24356964374999990, 3.323476615752268604, -7.828124999385470240 ) ) ;
#26302 = EDGE_CURVE ( 'NONE', #8245, #26216, #22900, .T. ) ;
#26301 = CARTESIAN_POINT ( 'NONE',  ( 13.50000000000001421, 196.1000000000000227, 23.38268590217984055 ) ) ;
#26303 = CARTESIAN_POINT ( 'NONE',  ( 31.03952447949476579, 7.209453229046482114, 164.7522898954867685 ) ) ;
#26304 = CARTESIAN_POINT ( 'NONE',  ( 28.00600070531170971, -5.196152422706638241, 164.5000942319139483 ) ) ;
#26305 = CARTESIAN_POINT ( 'NONE',  ( -13.50000000000000533, 198.1250000000000284, -23.38268590217984411 ) ) ;
#26306 = CARTESIAN_POINT ( 'NONE',  ( 15.00000000000000000, 248.1625000000000227, -3.464101615137752166 ) ) ;
#26307 = CARTESIAN_POINT ( 'NONE',  ( -27.24356964375000345, 198.8656250006145285, -15.72908226750537786 ) ) ;
#26308 = EDGE_CURVE ( 'NONE', #23800, #20737, #36256, .T. ) ;
#26309 = CARTESIAN_POINT ( 'NONE',  ( -0.1745138560722763466, 128.3898137178985621, -12.50000000000000355 ) ) ;
#26310 = CARTESIAN_POINT ( 'NONE',  ( 2.660918448318279950, 116.4976862821014549, -12.46528703574805874 ) ) ;
#26312 = ORIENTED_EDGE ( 'NONE', *, *, #12409, .T. ) ;
#26311 = ORIENTED_EDGE ( 'NONE', *, *, #32089, .F. ) ;
#26313 = CARTESIAN_POINT ( 'NONE',  ( -13.62178482187498396, 196.7281250006145399, 23.59362340125808188 ) ) ;
#26314 = CARTESIAN_POINT ( 'NONE',  ( 15.24356964374999990, 241.6093750006145058, -3.323476615752268604 ) ) ;
#26315 = ADVANCED_FACE ( 'NONE', ( #23082 ), #17400, .T. ) ;
#26316 = CARTESIAN_POINT ( 'NONE',  ( 3.257655550456945548, 86.70231371789851949, 15.46528703574811736 ) ) ;
#26317 = CARTESIAN_POINT ( 'NONE',  ( 15.24356964375000167, -3.323476615752272600, -3.815624999385473615 ) ) ;
#26318 = CARTESIAN_POINT ( 'NONE',  ( 23.87821517812499650, 247.9093750006145171, -4.985214923628404904 ) ) ;
#26319 = EDGE_CURVE ( 'NONE', #23956, #31856, #28940, .T. ) ;
#26320 = CARTESIAN_POINT ( 'NONE',  ( 26.99999999999999645, 195.8750000012290400, -15.58845726811990495 ) ) ;
#26321 = CARTESIAN_POINT ( 'NONE',  ( -5.233372021372612259, 69.45231371789853370, 8.152565276336593669 ) ) ;
#26322 = CARTESIAN_POINT ( 'NONE',  ( 16.56230152254411081, -7.209453229046475009, -6.328124999385527083 ) ) ;
#26323 =( BOUNDED_CURVE ( )  B_SPLINE_CURVE ( 2, ( #12703, #23709, #29953, #35819, #9677, #29382, #12893 ),
 .UNSPECIFIED., .F., .F. ) 
 B_SPLINE_CURVE_WITH_KNOTS ( ( 3, 2, 2, 3 ),
 ( 0.3260869565217384136, 0.3333333333333327042, 0.3405797101449269948, 0.3478260869565212854 ),
 .UNSPECIFIED. ) 
 CURVE ( )  GEOMETRIC_REPRESENTATION_ITEM ( )  RATIONAL_B_SPLINE_CURVE ( ( 1.000000000000013545, 0.8660254037844254960, 1.000000000000000000, 0.8660254037844387076, 1.000000000000000000, 0.8660254037844469233, 0.9999999999999917843 ) ) 
 REPRESENTATION_ITEM ( '' )  );
#26324 = CARTESIAN_POINT ( 'NONE',  ( 26.75643035624999655, 242.7718750006145001, -7.049594010296217766E-16 ) ) ;
#26325 = CARTESIAN_POINT ( 'NONE',  ( 11.48171059495408208, 47.31481371789855928, -4.944772684328420986 ) ) ;
#26326 = FACE_OUTER_BOUND ( 'NONE', #5334, .T. ) ;
#26327 = CARTESIAN_POINT ( 'NONE',  ( -12.46528703574805697, 104.9976862821014691, -2.660918448318280838 ) ) ;
#26328 = CARTESIAN_POINT ( 'NONE',  ( 22.56230152254410370, 7.347880794884117764E-16, -3.712499998771018106 ) ) ;
#26329 = CARTESIAN_POINT ( 'NONE',  ( -68.01413769728823411, 212.1499508600178387, 3.954877714930865817 ) ) ;
#26330 = CARTESIAN_POINT ( 'NONE',  ( -12.50000000000000355, 141.5101862821014720, -0.1745138560725492671 ) ) ;
#26331 = CARTESIAN_POINT ( 'NONE',  ( 24.73307100032172201, 3.464101615137450185, 161.5114762576326370 ) ) ;
#26332 = CARTESIAN_POINT ( 'NONE',  ( -8.927990412390661490, 103.2726862821014322, 13.04141134922759804 ) ) ;
#26333 = DIRECTION ( 'NONE',  ( 0.000000000000000000, -0.000000000000000000, -1.000000000000000000 ) ) ;
#26334 = FACE_OUTER_BOUND ( 'NONE', #12642, .T. ) ;
#26335 = CARTESIAN_POINT ( 'NONE',  ( 15.00000000000000000, 0.000000000000000000, -2.643749998770955401 ) ) ;
#26336 = CARTESIAN_POINT ( 'NONE',  ( 8.710071997420127943, 109.8851862821014720, 3.796722387233375073 ) ) ;
#26337 = CARTESIAN_POINT ( 'NONE',  ( 1.255007937094097924E-14, 199.1000000012290627, -27.00000000000000000 ) ) ;
#26338 = VECTOR ( 'NONE', #32603, 1000.000000000000114 ) ;
#26339 = CARTESIAN_POINT ( 'NONE',  ( 0.1745138560725837118, 15.01018628210143291, -15.50000000000000533 ) ) ;
#26340 = CARTESIAN_POINT ( 'NONE',  ( 26.75643035624999655, 243.1843750006144944, 3.323476615752267715 ) ) ;
#26341 = ORIENTED_EDGE ( 'NONE', *, *, #10195, .T. ) ;
#26342 = CARTESIAN_POINT ( 'NONE',  ( 34.54326498017087488, 5.407089921784857367, 168.9817632126399758 ) ) ;
#26343 = CARTESIAN_POINT ( 'NONE',  ( -5.233372021372430183, 60.14768628210144641, -8.152565276336710909 ) ) ;
#26344 = CARTESIAN_POINT ( 'NONE',  ( 15.24356964374999990, 3.323476615752268604, -0.1781249993854788494 ) ) ;
#26345 = ADVANCED_FACE ( 'NONE', ( #34814 ), #31976, .T. ) ;
#26346 = CARTESIAN_POINT ( 'NONE',  ( 26.99999999999999645, 241.6750000000000114, -7.347880794884117764E-16 ) ) ;
#26347 = CARTESIAN_POINT ( 'NONE',  ( 22.56230152254411792, 7.347880794884125653E-16, -7.875000000000048850 ) ) ;
#26348 = DIRECTION ( 'NONE',  ( 0.000000000000000000, 0.000000000000000000, 1.000000000000000000 ) ) ;
#26349 = CARTESIAN_POINT ( 'NONE',  ( 36.95214294612679851, -3.464101615137475942, 163.4915487413387893 ) ) ;
#26350 = CARTESIAN_POINT ( 'NONE',  ( 10.56230152254410903, 0.000000000000000000, -8.437499998771025744 ) ) ;
#26351 = CARTESIAN_POINT ( 'NONE',  ( 5.233372021372610483, 37.25231371789855217, -8.152565276336593669 ) ) ;
#26352 = CARTESIAN_POINT ( 'NONE',  ( 13.62178482187501416, 199.5593750006145513, 23.59362340125806767 ) ) ;
#26353 = ORIENTED_EDGE ( 'NONE', *, *, #19875, .F. ) ;
#26354 = CARTESIAN_POINT ( 'NONE',  ( 15.24356964374999990, 248.3593750006145342, -3.323476615752268604 ) ) ;
#26355 = CARTESIAN_POINT ( 'NONE',  ( 7.228626920338837358, 49.32731371789855501, 10.49813415416005036 ) ) ;
#26356 = CARTESIAN_POINT ( 'NONE',  ( 23.87821517812500005, -4.985214923628404016, -10.00312499938549315 ) ) ;
#26357 = CARTESIAN_POINT ( 'NONE',  ( -8.715434833792127023, 14.53981371789855892, 8.962234695871568846 ) ) ;
#26358 = LINE ( 'NONE', #6471, #34760 ) ;
#26359 = ORIENTED_EDGE ( 'NONE', *, *, #23703, .T. ) ;
#26360 = CARTESIAN_POINT ( 'NONE',  ( 13.44051670066911086, 5.407089921784862696, -2.971874999385532234 ) ) ;
#26361 = CONICAL_SURFACE ( 'NONE', #932, 5.999999999999998224, 0.2617993877991499074 ) ;
#26362 = ORIENTED_EDGE ( 'NONE', *, *, #9673, .T. ) ;
#26363 = CARTESIAN_POINT ( 'NONE',  ( 5.778771075727756162E-15, 198.5656250006145171, 31.45816453501075927 ) ) ;
#26364 = CARTESIAN_POINT ( 'NONE',  ( 31.25523494279520165, -7.209453229046482114, 167.2178717732638233 ) ) ;
#26365 = AXIS2_PLACEMENT_3D ( 'NONE', #18706, #27212, #1235 ) ;
#26366 = CARTESIAN_POINT ( 'NONE',  ( -35.74627896937850124, 203.4690446883607535, -1.626142955000504209 ) ) ;
#26367 = CARTESIAN_POINT ( 'NONE',  ( 26.75643035624999655, 248.5843750006145001, 3.323476615752267271 ) ) ;
#26368 = PRESENTATION_STYLE_ASSIGNMENT (( #1157 ) ) ;
#26369 = FACE_OUTER_BOUND ( 'NONE', #32838, .T. ) ;
#26370 = CARTESIAN_POINT ( 'NONE',  ( -61.67336230271184405, 213.9548777149308023, 2.149950860017852960 ) ) ;
#26371 = CARTESIAN_POINT ( 'NONE',  ( 25.05990503573306682, 0.000000000000000000, 165.2472063767010013 ) ) ;
#26372 = CARTESIAN_POINT ( 'NONE',  ( 37.31166038496018444, 3.464101615137866297, 167.6008518709673183 ) ) ;
#26373 = VERTEX_POINT ( 'NONE', #32157 ) ;
#26374 = CARTESIAN_POINT ( 'NONE',  ( -28.58815133238078232, 203.6511048533163546, 4.874370134510862762 ) ) ;
#26375 = CARTESIAN_POINT ( 'NONE',  ( -8.632099005475794229, 14.25231371789853618, 13.23911966647199812 ) ) ;
#26376 = CARTESIAN_POINT ( 'NONE',  ( -59.10788769728823411, 218.4690446883607535, 2.393094931466250408 ) ) ;
#26377 = CARTESIAN_POINT ( 'NONE',  ( 6.594114490232313663, 128.8601862821014663, 6.840914352312096547 ) ) ;
#26378 = EDGE_CURVE ( 'NONE', #26550, #36019, #25009, .T. ) ;
#26379 = CARTESIAN_POINT ( 'NONE',  ( 7.228626920339068285, 52.67268628210144499, -10.49813415415989581 ) ) ;
#26380 = CARTESIAN_POINT ( 'NONE',  ( 13.56230152254411614, -5.196152422706638241, -5.325000000000079226 ) ) ;
#26381 = EDGE_LOOP ( 'NONE', ( #26206, #23020, #21540, #27185 ) ) ;
#26382 = CARTESIAN_POINT ( 'NONE',  ( -47.03497103062156981, 204.4285982733020148, -3.350049139982115509 ) ) ;
#26383 = EDGE_CURVE ( 'NONE', #35593, #28768, #7094, .T. ) ;
#26384 = CARTESIAN_POINT ( 'NONE',  ( -29.50000000000000711, 252.0000000000000000, 2.500000000000005329 ) ) ;
#26385 = CARTESIAN_POINT ( 'NONE',  ( 5.529263428287477744, 15.87268628210144605, -7.954856959092191815 ) ) ;
#26386 = CARTESIAN_POINT ( 'NONE',  ( -13.62178482187500528, 197.0843750006145285, -23.59362340125807123 ) ) ;
#26387 = CARTESIAN_POINT ( 'NONE',  ( 13.50000000000001421, 198.0125000012290286, 23.38268590217984055 ) ) ;
#26388 = CARTESIAN_POINT ( 'NONE',  ( 15.00000000000000000, 0.000000000000000000, -3.993749998770945719 ) ) ;
#26389 = EDGE_CURVE ( 'NONE', #32692, #22009, #35563, .T. ) ;
#26390 = CARTESIAN_POINT ( 'NONE',  ( -79.65000000000001990, 210.0000000000000000, 3.000000000000000000 ) ) ;
#26391 = CARTESIAN_POINT ( 'NONE',  ( 15.00000000000000000, 240.1562500012290684, 0.000000000000000000 ) ) ;
#26392=STYLED_ITEM('',(#37528),#21232);
#26393 = CARTESIAN_POINT ( 'NONE',  ( 23.87821517812500005, 245.9593750006145569, 4.985214923628404016 ) ) ;
#26394 = CARTESIAN_POINT ( 'NONE',  ( 0.1745138560723095977, 86.98981371789857064, 9.500000000000005329 ) ) ;
#26395 = CARTESIAN_POINT ( 'NONE',  ( 20.99999999999999645, 240.0718750006145399, 6.646953231504538984 ) ) ;
#26396 = ORIENTED_EDGE ( 'NONE', *, *, #10179, .T. ) ;
#26397 = CARTESIAN_POINT ( 'NONE',  ( -54.15997103062156981, 215.5714017266979852, 3.350049139982118618 ) ) ;
#26398 = PRODUCT_RELATED_PRODUCT_CATEGORY ( 'part', '', ( #28915 ) ) ;
#26399 = CARTESIAN_POINT ( 'NONE',  ( 26.99999999999999645, 247.0937500012290400, 3.464101615137751278 ) ) ;
#26400 = CARTESIAN_POINT ( 'NONE',  ( 7.228626920338837358, 104.5273137178985507, 10.49813415416005036 ) ) ;
#26401 = CARTESIAN_POINT ( 'NONE',  ( 13.44051670066911264, -5.407089921784865361, -1.471874999385502925 ) ) ;
#26402 = CARTESIAN_POINT ( 'NONE',  ( 27.46714883140487373, 5.407089921784856479, 159.7383132535862842 ) ) ;
#26403 = CARTESIAN_POINT ( 'NONE',  ( 21.00000000000000000, -6.646953231504538984, -2.840624999385488181 ) ) ;
#26404 = CARTESIAN_POINT ( 'NONE',  ( -0.1745138560722763466, 63.98981371789854933, -12.50000000000000355 ) ) ;
#26405 = CARTESIAN_POINT ( 'NONE',  ( 27.24356964375000700, 197.3468750006145740, 15.72908226750537075 ) ) ;
#26406 = EDGE_LOOP ( 'NONE', ( #5151, #27533, #8003, #12290 ) ) ;
#26407 = ORIENTED_EDGE ( 'NONE', *, *, #29602, .T. ) ;
#26408 = CARTESIAN_POINT ( 'NONE',  ( 26.75643035624999655, 3.323476615752271268, -5.278124999385450877 ) ) ;
#26409 = CARTESIAN_POINT ( 'NONE',  ( 26.75643035624999655, 245.4718750006145171, -7.049594010296217766E-16 ) ) ;
#26410 = CARTESIAN_POINT ( 'NONE',  ( 7.228626920339068285, 43.47268628210144925, -10.49813415415989581 ) ) ;
#26411 = CARTESIAN_POINT ( 'NONE',  ( -46.23586230271182984, 206.8500491399821328, 5.686928522499748340 ) ) ;
#26412 = CARTESIAN_POINT ( 'NONE',  ( -64.84002896937850835, 204.4285982733020433, 3.350049139982171020 ) ) ;
#26413 = CARTESIAN_POINT ( 'NONE',  ( 27.74126513682283601, -5.196152422706632912, 161.4741528376846134 ) ) ;
#26414 = CARTESIAN_POINT ( 'NONE',  ( 12.46528703574811558, 112.0023137178985735, -2.660918448318005503 ) ) ;
#26415 = CARTESIAN_POINT ( 'NONE',  ( -59.30580436395490551, 214.5000000000000284, 0.1155267958017899832 ) ) ;
#26416 =( BOUNDED_CURVE ( )  B_SPLINE_CURVE ( 2, ( #29185, #3227, #14800, #32225, #26346, #382, #23517, #35063, #9113 ),
 .UNSPECIFIED., .F., .F. ) 
 B_SPLINE_CURVE_WITH_KNOTS ( ( 3, 2, 2, 2, 3 ),
 ( 0.7934782608695651884, 0.7971014492753623060, 0.8043478260869565410, 0.8115942028985507761, 0.8152173913043478937 ),
 .UNSPECIFIED. ) 
 CURVE ( )  GEOMETRIC_REPRESENTATION_ITEM ( )  RATIONAL_B_SPLINE_CURVE ( ( 0.9330127018922194093, 0.9330127018922194093, 1.000000000000000000, 0.8660254037844387076, 1.000000000000000000, 0.8660254037844387076, 1.000000000000000000, 0.9330127018922182991, 0.9330127018922192983 ) ) 
 REPRESENTATION_ITEM ( '' )  );
#26417 = CARTESIAN_POINT ( 'NONE',  ( -37.53497103062155560, 202.6965474657331185, -4.350049139982091084 ) ) ;
#26418 = CARTESIAN_POINT ( 'NONE',  ( 18.12178482187499640, 4.985214923628404904, -6.178124999385470772 ) ) ;
#26419 = CARTESIAN_POINT ( 'NONE',  ( 10.56230152254419430, -3.464101615137802348, -4.349999998771035159 ) ) ;
#26420 = CARTESIAN_POINT ( 'NONE',  ( 8.632099005475788900, 74.05231371789854222, -13.23911966647199812 ) ) ;
#26421 = CARTESIAN_POINT ( 'NONE',  ( -61.67336230271184405, 217.4189793300686233, 4.149950860017807663 ) ) ;
#26422 = VERTEX_POINT ( 'NONE', #3913 ) ;
#26423 = CARTESIAN_POINT ( 'NONE',  ( 24.86380461455084756, 0.000000000000000000, 163.0057683059945930 ) ) ;
#26424 = CARTESIAN_POINT ( 'NONE',  ( -8.715434833791929847, 96.66018628210146346, -8.962234695871762469 ) ) ;
#26425 = CARTESIAN_POINT ( 'NONE',  ( 15.53471296425195369, 44.62268628210144783, -2.908627838312120684 ) ) ;
#26426 = CARTESIAN_POINT ( 'NONE',  ( -9.000000000000024869, 210.0000000000000000, 0.000000000000000000 ) ) ;
#26427 = CARTESIAN_POINT ( 'NONE',  ( 33.82899049407978964, 6.917534487978463709, 159.0481132747639492 ) ) ;
#26428 = CARTESIAN_POINT ( 'NONE',  ( 14.25334919248782661, 63.88518628210145778, 6.092822981423971385 ) ) ;
#26429 = AXIS2_PLACEMENT_3D ( 'NONE', #20611, #37278, #3344 ) ;
#26430 = CYLINDRICAL_SURFACE ( 'NONE', #15143, 5.999999999999998224 ) ;
#26431 = CARTESIAN_POINT ( 'NONE',  ( 10.31873187879410736, -3.604726614523240613, -8.203124999385503102 ) ) ;
#26432 = CARTESIAN_POINT ( 'NONE',  ( 19.56230152254412502, -5.196152422706635576, -2.550000000000052225 ) ) ;
#26433 = CARTESIAN_POINT ( 'NONE',  ( -53.36830436395489841, 209.8844732041982581, 6.500000000000000888 ) ) ;
#26434 = CARTESIAN_POINT ( 'NONE',  ( 5.649999999999987921, 244.5000000000000000, 2.500000000000000000 ) ) ;
#26435 = CARTESIAN_POINT ( 'NONE',  ( 8.962234695871762469, 34.56018628210144783, -8.715434833791931624 ) ) ;
#26437 = CARTESIAN_POINT ( 'NONE',  ( -1.926257025242585782E-15, 199.2968750006145342, -31.45816453501075927 ) ) ;
#26436 =( BOUNDED_CURVE ( )  B_SPLINE_CURVE ( 2, ( #24376, #16038, #21726, #27587, #33276, #18888, #35920 ),
 .UNSPECIFIED., .F., .F. ) 
 B_SPLINE_CURVE_WITH_KNOTS ( ( 3, 2, 2, 3 ),
 ( 0.8913043478260829211, 0.8985507246376781554, 0.9057971014492732786, 0.9130434782608684019 ),
 .UNSPECIFIED. ) 
 CURVE ( )  GEOMETRIC_REPRESENTATION_ITEM ( )  RATIONAL_B_SPLINE_CURVE ( ( 1.000000000000073941, 0.8660254037843647668, 1.000000000000000000, 0.8660254037844387076, 1.000000000000000000, 0.8660254037844592467, 0.9999999999999794609 ) ) 
 REPRESENTATION_ITEM ( '' )  );
#26438 = CARTESIAN_POINT ( 'NONE',  ( 25.09912511996950713, 0.000000000000000000, 165.6954939908422944 ) ) ;
#26439 = CARTESIAN_POINT ( 'NONE',  ( 8.710071997420127943, 8.685186282101437172, 3.796722387233375073 ) ) ;
#26440 = CARTESIAN_POINT ( 'NONE',  ( 23.87821517812499650, 247.4593750006145285, -4.985214923628404904 ) ) ;
#26441 = EDGE_LOOP ( 'NONE', ( #28073, #3304, #36013, #9959, #15633, #5583, #17148, #22022, #30992, #18231, #36401, #28636, #21444, #10800, #1140, #35294, #2960, #19896, #13095, #15234, #24692, #4085, #27343, #25602, #20356, #21647, #4735, #4137, #18863, #34741, #6557, #473, #8009, #14795, #15359, #9077, #11026, #18535, #30624, #8111, #33989, #25664, #19486, #25520, #16959, #5686, #33811, #37127 ) ) ;
#26442 = CARTESIAN_POINT ( 'NONE',  ( 15.00000000000000000, 0.000000000000000000, -8.099999999999996092 ) ) ;
#26443 = CARTESIAN_POINT ( 'NONE',  ( 21.00000000000000000, 243.3624999999999829, 5.999999999999998224 ) ) ;
#26444 = CARTESIAN_POINT ( 'NONE',  ( 10.56230152254345001, -3.464101615137374246, -3.449999998771020593 ) ) ;
#26445 = CARTESIAN_POINT ( 'NONE',  ( 16.56230152254411436, -7.209453229046475009, -4.978124999385539873 ) ) ;
#26446 = CARTESIAN_POINT ( 'NONE',  ( 37.52570519453759346, -3.604726614523235284, 167.2527469918319412 ) ) ;
#26447 = CARTESIAN_POINT ( 'NONE',  ( 18.00000000000000355, 241.5249999999999773, 5.196152422706632912 ) ) ;
#26448 = CARTESIAN_POINT ( 'NONE',  ( 36.60569886870491985, 3.464101615137448409, 159.5316748164241005 ) ) ;
#26449 = EDGE_CURVE ( 'NONE', #13344, #21775, #37285, .T. ) ;
#26450 = CARTESIAN_POINT ( 'NONE',  ( 0.1745138560725515708, 42.61018628210144499, -12.50000000000000355 ) ) ;
#26451 = ORIENTED_EDGE ( 'NONE', *, *, #23618, .F. ) ;
#26452 = EDGE_LOOP ( 'NONE', ( #24370, #2884 ) ) ;
#26453 = CARTESIAN_POINT ( 'NONE',  ( 26.99999999999999289, 0.000000000000000000, -8.000000000000000000 ) ) ;
#26454 = CARTESIAN_POINT ( 'NONE',  ( 20.99999999999999645, 0.000000000000000000, -8.000000000000000000 ) ) ;
#26455 = CARTESIAN_POINT ( 'NONE',  ( 26.75643035624999655, 3.323476615752271712, -5.728124999385479477 ) ) ;
#26456 = CARTESIAN_POINT ( 'NONE',  ( -4.622313124798576922, 97.23518628210145209, -11.61527771782819762 ) ) ;
#26457 = CARTESIAN_POINT ( 'NONE',  ( -15.53471296425188442, 25.17731371789854933, -2.908627838312459080 ) ) ;
#26458 = FACE_OUTER_BOUND ( 'NONE', #6833, .T. ) ;
#26459 = CARTESIAN_POINT ( 'NONE',  ( 18.12178482187500350, 241.3843750006145115, 4.985214923628407568 ) ) ;
#26460 = CARTESIAN_POINT ( 'NONE',  ( -33.77455436395489841, 206.6211998817774997, 3.209657149897401585 ) ) ;
#26461 = CYLINDRICAL_SURFACE ( 'NONE', #4631, 5.999999999999998224 ) ;
#26462 = CARTESIAN_POINT ( 'NONE',  ( 27.50146640511176344, 5.407089921784862696, 160.1305649159599227 ) ) ;
#26463 = CARTESIAN_POINT ( 'NONE',  ( -9.500000000000005329, 24.88981371789854080, 0.1745138560723101806 ) ) ;
#26464 = CARTESIAN_POINT ( 'NONE',  ( -61.68080436395489841, 203.5000000000000000, -0.1155267958017335561 ) ) ;
#26465 = ADVANCED_FACE ( 'NONE', ( #15866 ), #12821, .F. ) ;
#26466 = CARTESIAN_POINT ( 'NONE',  ( -35.74627896937850124, 201.4690446883607251, -2.162041339862721845 ) ) ;
#26467 = DIRECTION ( 'NONE',  ( 1.000000000000000000, 0.000000000000000000, 0.000000000000000000 ) ) ;
#26468 = CARTESIAN_POINT ( 'NONE',  ( 19.56230152254410370, 5.196152422706631135, -4.537499998771011178 ) ) ;
#26469 = CARTESIAN_POINT ( 'NONE',  ( 27.24356964375000345, 196.4843750006145626, -3.336375036156643733E-15 ) ) ;
#26470 = CARTESIAN_POINT ( 'NONE',  ( 15.53471296425188797, 130.9773137178985394, 2.908627838312457747 ) ) ;
#26471 = CARTESIAN_POINT ( 'NONE',  ( -57.91294563604515133, 214.6737587650350747, -4.842901733360249317 ) ) ;
#26472 = ORIENTED_EDGE ( 'NONE', *, *, #28486, .F. ) ;
#26473 = CARTESIAN_POINT ( 'NONE',  ( 12.50000000000000355, 44.91018628210144215, 0.1745138560725507937 ) ) ;
#26474 = DIRECTION ( 'NONE',  ( -0.000000000000000000, -0.000000000000000000, 1.000000000000000000 ) ) ;
#26475 = CARTESIAN_POINT ( 'NONE',  ( 25.06157068934916765, 3.604726614523240613, 168.0608931323890829 ) ) ;
#26476 = CARTESIAN_POINT ( 'NONE',  ( 26.99999999999999645, -3.464101615137751278, -3.356249998770971743 ) ) ;
#26477 =( BOUNDED_CURVE ( )  B_SPLINE_CURVE ( 2, ( #10029, #21609, #32590, #6628, #18204, #33159, #7205 ),
 .UNSPECIFIED., .F., .F. ) 
 B_SPLINE_CURVE_WITH_KNOTS ( ( 3, 2, 2, 3 ),
 ( 0.4565217391304355332, 0.4637681159420298238, 0.4710144927536241144, 0.4782608695652184050 ),
 .UNSPECIFIED. ) 
 CURVE ( )  GEOMETRIC_REPRESENTATION_ITEM ( )  RATIONAL_B_SPLINE_CURVE ( ( 0.9999999999999856781, 0.8660254037844530295, 1.000000000000000000, 0.8660254037844387076, 1.000000000000000000, 0.8660254037844202779, 1.000000000000018430 ) ) 
 REPRESENTATION_ITEM ( '' )  );
#26478 = CARTESIAN_POINT ( 'NONE',  ( -65.04538769728823411, 211.8571965466040012, -6.469044688360769513 ) ) ;
#26479 = CARTESIAN_POINT ( 'NONE',  ( 10.31873187879411091, -3.604726614523240613, -1.453124999385536187 ) ) ;
#26480 = CARTESIAN_POINT ( 'NONE',  ( 6.594114490232313663, 64.46018628210146062, 6.840914352312096547 ) ) ;
#26481 = DIRECTION ( 'NONE',  ( 0.08715574274765150453, 0.000000000000000000, 0.9961946980917461003 ) ) ;
#26482 = CARTESIAN_POINT ( 'NONE',  ( -1.045839947578415010E-13, 195.7250000012290343, 27.00000000000000355 ) ) ;
#26483 = EDGE_CURVE ( 'NONE', #26027, #26157, #8307, .T. ) ;
#26484 = CARTESIAN_POINT ( 'NONE',  ( -2.311890736173176641, 88.32268628210144357, -12.53471296425194836 ) ) ;
#26485 = DIRECTION ( 'NONE',  ( 0.08715574274765150453, 0.000000000000000000, 0.9961946980917461003 ) ) ;
#26486 = EDGE_LOOP ( 'NONE', ( #21121, #21154, #1231, #34359 ) ) ;
#26487 = CARTESIAN_POINT ( 'NONE',  ( 24.43895185209563792, 3.604726614523236616, 160.9443272578961626 ) ) ;
#26488 = CARTESIAN_POINT ( 'NONE',  ( 15.00000000000000000, 3.464101615137752166, -0.4874999999999927169 ) ) ;
#26489 = CARTESIAN_POINT ( 'NONE',  ( -7.234628195640354420, 195.7049038117966404, 26.99999999999996803 ) ) ;
#26490 = CARTESIAN_POINT ( 'NONE',  ( 37.25279877505901993, 3.604726614523243278, 164.1334123434321555 ) ) ;
#26491 = CARTESIAN_POINT ( 'NONE',  ( 27.91448717542667168, 5.196152422706636465, 163.4540897989176642 ) ) ;
#26492 = DIRECTION ( 'NONE',  ( 0.000000000000000000, 0.000000000000000000, 1.000000000000000000 ) ) ;
#26493 = CARTESIAN_POINT ( 'NONE',  ( 26.99999999999999645, 247.5625000000000000, -3.464101615137755275 ) ) ;
#26494 = CARTESIAN_POINT ( 'NONE',  ( 27.24356964374999279, 195.1156250006145285, -15.72908226750539207 ) ) ;
#26495 = EDGE_CURVE ( 'NONE', #24827, #7868, #18531, .T. ) ;
#26496 = CARTESIAN_POINT ( 'NONE',  ( 11.48171059495408208, 102.5148137178985621, -4.944772684328420986 ) ) ;
#26497 = CARTESIAN_POINT ( 'NONE',  ( -12.46528703574805874, 114.1976862821014578, -2.660918448318280838 ) ) ;
#26498 = CIRCLE ( 'NONE', #30138, 6.000000000000001776 ) ;
#26500 = ORIENTED_EDGE ( 'NONE', *, *, #31169, .T. ) ;
#26499 = ORIENTED_EDGE ( 'NONE', *, *, #12862, .F. ) ;
#26501 = CARTESIAN_POINT ( 'NONE',  ( -27.24356964374999990, 195.7156250006145513, -15.72908226750537786 ) ) ;
#26502 = CARTESIAN_POINT ( 'NONE',  ( 36.91945954259546880, 3.464101615138031054, 163.1179757295544448 ) ) ;
#26503 = CARTESIAN_POINT ( 'NONE',  ( 2.908627838312458636, 73.47731371789855359, -15.53471296425188442 ) ) ;
#26504 = CARTESIAN_POINT ( 'NONE',  ( 21.00000000000000000, -6.646953231504538984, -4.640624999385471128 ) ) ;
#26505 = CARTESIAN_POINT ( 'NONE',  ( 23.87821517812499650, 248.3593750006145342, -4.985214923628404904 ) ) ;
#26506 = CARTESIAN_POINT ( 'NONE',  ( -0.1745138560725182642, 102.4101862821014493, 9.500000000000005329 ) ) ;
#26507 = PRODUCT_DEFINITION_SHAPE ( 'NONE', 'NONE',  #31497 ) ;
#26508 = CARTESIAN_POINT ( 'NONE',  ( -26.99999999999998934, 197.4500000012290570, 15.58845726811991561 ) ) ;
#26509 = CARTESIAN_POINT ( 'NONE',  ( -1.715153634034442431, 78.07731371789854791, 9.534712964251900402 ) ) ;
#26510 = CARTESIAN_POINT ( 'NONE',  ( 19.68408634441910365, 5.407089921784857367, -4.340624999385561900 ) ) ;
#26511 = AXIS2_PLACEMENT_3D ( 'NONE', #4665, #7524, #19099 ) ;
#26512 = CARTESIAN_POINT ( 'NONE',  ( 20.99999999999999645, 241.0843750006145285, -6.646953231504538984 ) ) ;
#26513 = CARTESIAN_POINT ( 'NONE',  ( 12.53471296425189330, 48.17731371789854933, 2.311890736173451977 ) ) ;
#26514 = CARTESIAN_POINT ( 'NONE',  ( 37.19073179189800271, 7.347880794884117764E-16, 166.2186317273649934 ) ) ;
#26515 = CARTESIAN_POINT ( 'NONE',  ( -10.49813415415989581, 105.5726862821014578, -7.228626920339068285 ) ) ;
#26516 = CARTESIAN_POINT ( 'NONE',  ( 22.56230152254409660, 3.464101615137755275, -7.274999998771023435 ) ) ;
#26517 = CARTESIAN_POINT ( 'NONE',  ( -69.00372103062157692, 214.5309553116392749, -1.090244570138262148 ) ) ;
#26518 = FACE_OUTER_BOUND ( 'NONE', #161, .T. ) ;
#26519 = DIRECTION ( 'NONE',  ( 0.000000000000000000, 0.000000000000000000, -1.000000000000000000 ) ) ;
#26520 = VECTOR ( 'NONE', #14351, 1000.000000000000000 ) ;
#26521 = CARTESIAN_POINT ( 'NONE',  ( -6.092822981423970496, 84.58518628210146062, 14.25334919248782661 ) ) ;
#26522 = CARTESIAN_POINT ( 'NONE',  ( 20.99999999999999645, 185.0294372515228645, 5.999999999999999112 ) ) ;
#26523 =( BOUNDED_CURVE ( )  B_SPLINE_CURVE ( 2, ( #21989, #33536, #4536, #19152, #15926, #27475, #30881 ),
 .UNSPECIFIED., .F., .F. ) 
 B_SPLINE_CURVE_WITH_KNOTS ( ( 3, 2, 2, 3 ),
 ( 0.4347826086956499969, 0.4420289855072442875, 0.4492753623188385781, 0.4565217391304328132 ),
 .UNSPECIFIED. ) 
 CURVE ( )  GEOMETRIC_REPRESENTATION_ITEM ( )  RATIONAL_B_SPLINE_CURVE ( ( 1.000000000000039968, 0.8660254037843986286, 1.000000000000000000, 0.8660254037844387076, 1.000000000000000000, 0.8660254037844746788, 0.9999999999999640288 ) ) 
 REPRESENTATION_ITEM ( '' )  );
#26524 = LINE ( 'NONE', #12509, #5441 ) ;
#26525 = CARTESIAN_POINT ( 'NONE',  ( 2.064181346179272847, 107.2976862821014521, -9.465287035748065847 ) ) ;
#26526 = CARTESIAN_POINT ( 'NONE',  ( -81.00000000000002842, 210.0000000000000000, 0.000000000000000000 ) ) ;
#26527 = CARTESIAN_POINT ( 'NONE',  ( 15.46528703574804986, 17.59768628210143504, 3.257655550457285720 ) ) ;
#26528 = CARTESIAN_POINT ( 'NONE',  ( -13.62178482187500528, 196.1843750006145228, -23.59362340125807123 ) ) ;
#26529 = CARTESIAN_POINT ( 'NONE',  ( 15.24356964375000167, 241.2343750006145058, 3.323476615752272600 ) ) ;
#26530 = ORIENTED_EDGE ( 'NONE', *, *, #1751, .T. ) ;
#26531 = CARTESIAN_POINT ( 'NONE',  ( 37.52897353489062482, 7.646167579472015790E-16, 167.2901042930103586 ) ) ;
#26532 = CARTESIAN_POINT ( 'NONE',  ( 21.00000000000000000, -6.646953231504538984, -0.4781249993854547187 ) ) ;
#26533 = EDGE_CURVE ( 'NONE', #25349, #21187, #6963, .T. ) ;
#26534 = CARTESIAN_POINT ( 'NONE',  ( -1.926257025242585782E-15, 199.2968750006145342, -31.45816453501076637 ) ) ;
#26535 = CARTESIAN_POINT ( 'NONE',  ( -20.80563922340697403, 195.0000000000000284, -17.20829382900668492 ) ) ;
#26536 = FACE_OUTER_BOUND ( 'NONE', #33563, .T. ) ;
#26537 = CARTESIAN_POINT ( 'NONE',  ( 25.37366570962461054, 0.000000000000000000, 168.8335072898312887 ) ) ;
#26538 = CARTESIAN_POINT ( 'NONE',  ( 19.68408634441910721, 5.407089921784857367, -0.7406249993855418268 ) ) ;
#26539 = CARTESIAN_POINT ( 'NONE',  ( -8.710071997420207879, 15.11481371789854933, 3.796722387233182339 ) ) ;
#26540 = CARTESIAN_POINT ( 'NONE',  ( 27.24356964374999279, 199.6718750006145058, -15.72908226750539207 ) ) ;
#26541 = VECTOR ( 'NONE', #35571, 1000.000000000000000 ) ;
#26542 = ORIENTED_EDGE ( 'NONE', *, *, #33928, .T. ) ;
#26543 = CARTESIAN_POINT ( 'NONE',  ( 26.75643035624999655, 249.5218750006145001, -7.049594010296217766E-16 ) ) ;
#26544 = CARTESIAN_POINT ( 'NONE',  ( 4.944772684328420986, 49.61481371789855643, 11.48171059495408208 ) ) ;
#26545 = CARTESIAN_POINT ( 'NONE',  ( 21.00000000000000000, -6.646953231504538984, -1.378124999385478056 ) ) ;
#26546 = CARTESIAN_POINT ( 'NONE',  ( -6.932735513424201912, 14.25231371789853441, 10.69584247140429412 ) ) ;
#26547 = EDGE_CURVE ( 'NONE', #25530, #2674, #19725, .T. ) ;
#26548 =( BOUNDED_CURVE ( )  B_SPLINE_CURVE ( 2, ( #15598, #27154, #4589, #8189, #25052, #22038, #2302 ),
 .UNSPECIFIED., .F., .F. ) 
 B_SPLINE_CURVE_WITH_KNOTS ( ( 3, 2, 2, 3 ),
 ( 0.4999999999999988898, 0.5072463768115932359, 0.5144927536231874710, 0.5217391304347818171 ),
 .UNSPECIFIED. ) 
 CURVE ( )  GEOMETRIC_REPRESENTATION_ITEM ( )  RATIONAL_B_SPLINE_CURVE ( ( 1.000000000000020428, 0.8660254037844181685, 1.000000000000000000, 0.8660254037844387076, 1.000000000000000000, 0.8660254037844530295, 0.9999999999999856781 ) ) 
 REPRESENTATION_ITEM ( '' )  );
#26549 = PLANE ( 'NONE',  #15401 ) ;
#26550 = VERTEX_POINT ( 'NONE', #29690 ) ;
#26551 = CARTESIAN_POINT ( 'NONE',  ( 13.44051670066911264, -5.407089921784865361, -3.271874999385554261 ) ) ;
#26552 = CARTESIAN_POINT ( 'NONE',  ( 13.62178482187499640, 197.8531250006145399, -23.59362340125807123 ) ) ;
#26553 = CARTESIAN_POINT ( 'NONE',  ( 37.21357869082257253, 3.604726614523243278, 163.6851247292908909 ) ) ;
#26554 = CARTESIAN_POINT ( 'NONE',  ( -30.00669563604516910, 209.8844732041982013, -6.500000000000000888 ) ) ;
#26555 = CARTESIAN_POINT ( 'NONE',  ( 20.99999999999999645, 248.7343750006145058, -6.646953231504538984 ) ) ;
#26556 =( LENGTH_UNIT ( ) NAMED_UNIT ( * ) SI_UNIT ( .MILLI., .METRE. ) );
#26557 = CARTESIAN_POINT ( 'NONE',  ( 27.00000000000001776, 11.99999999999999822, 49.73803434254939759 ) ) ;
#26558 = EDGE_CURVE ( 'NONE', #33575, #23156, #16062, .T. ) ;
#26559 = CARTESIAN_POINT ( 'NONE',  ( -56.52752896937850124, 212.3500491399821613, 3.839350919129088435 ) ) ;
#26560 = CARTESIAN_POINT ( 'NONE',  ( -35.95163769728823411, 215.6869285224996986, -3.149950860017881382 ) ) ;
#26561 = CARTESIAN_POINT ( 'NONE',  ( 31.10325711637897328, -7.209453229046475009, 165.4807572684663342 ) ) ;
#26562 = ORIENTED_EDGE ( 'NONE', *, *, #8908, .T. ) ;
#26563 = CARTESIAN_POINT ( 'NONE',  ( 23.99999999999999645, 241.8062500012290457, -5.196152422706631135 ) ) ;
#26564 = CARTESIAN_POINT ( 'NONE',  ( 13.04141134922759804, 137.7726862821014606, 8.927990412390657937 ) ) ;
#26565 = CARTESIAN_POINT ( 'NONE',  ( -61.87872103062156981, 201.4690446883607819, 2.162041339862843525 ) ) ;
#26566 = CARTESIAN_POINT ( 'NONE',  ( -9.534712964251941258, 132.0226862821014322, 1.715153634034234154 ) ) ;
#26567 = CARTESIAN_POINT ( 'NONE',  ( 21.00000000000000000, 249.0437500012290570, -5.999999999999998224 ) ) ;
#26568 = CARTESIAN_POINT ( 'NONE',  ( -6.932735513423968321, 32.54768628210144499, -10.69584247140445221 ) ) ;
#26569 = CARTESIAN_POINT ( 'NONE',  ( 16.56230152254411436, 6.928203230275514990, -5.962500000000031442 ) ) ;
#26570 = EDGE_LOOP ( 'NONE', ( #23733, #35780, #33432, #6834 ) ) ;
#26571 = UNCERTAINTY_MEASURE_WITH_UNIT (LENGTH_MEASURE( 1.000000000000000082E-05 ), #37252, 'distance_accuracy_value', 'NONE');
#26572 = CARTESIAN_POINT ( 'NONE',  ( 3.257655550457285720, 125.6976862821014578, -15.46528703574804986 ) ) ;
#26573 = CARTESIAN_POINT ( 'NONE',  ( 20.99999999999999289, 242.2374999999999545, -5.999999999999997335 ) ) ;
#26574 = CARTESIAN_POINT ( 'NONE',  ( 9.534712964251900402, 140.1773137178985564, 1.715153634034445540 ) ) ;
#26575 = CARTESIAN_POINT ( 'NONE',  ( -27.24356964374999635, 194.9468750006145399, 15.72908226750539384 ) ) ;
#26576 = CARTESIAN_POINT ( 'NONE',  ( 15.12178482187499995, 0.000000000000000000, -0.07031249969274844247 ) ) ;
#26577 = CARTESIAN_POINT ( 'NONE',  ( -7.234628195640302017, 198.7424038105676800, 27.00000000000000711 ) ) ;
#26578 = CARTESIAN_POINT ( 'NONE',  ( -27.00000000000000711, 195.0263594398178100, -9.827196325189913040 ) ) ;
#26579 = CARTESIAN_POINT ( 'NONE',  ( 20.99999999999999645, 0.000000000000000000, -8.000000000000000000 ) ) ;
#26580 = CARTESIAN_POINT ( 'NONE',  ( 21.00000000000000000, 242.5468750006145342, -6.646953231504538984 ) ) ;
#26581 = CARTESIAN_POINT ( 'NONE',  ( 9.500000000000005329, 93.88981371789856212, -0.1745138560723090149 ) ) ;
#26582 = CARTESIAN_POINT ( 'NONE',  ( 18.12178482187500350, 240.4843750006145342, 4.985214923628407568 ) ) ;
#26583 = VERTEX_POINT ( 'NONE', #24525 ) ;
#26584 = CARTESIAN_POINT ( 'NONE',  ( -51.19122103062155560, 208.3738570449993404, -6.530955311639226935 ) ) ;
#26585 = CARTESIAN_POINT ( 'NONE',  ( 15.00000000000000000, 246.0062500012290627, 0.000000000000000000 ) ) ;
#26586 = CARTESIAN_POINT ( 'NONE',  ( -0.1745138560722763466, 91.58981371789856496, -12.50000000000000355 ) ) ;
#26587 = CARTESIAN_POINT ( 'NONE',  ( 22.80587116629412847, 3.604726614523243278, -1.734374999385497551 ) ) ;
#26588 = CARTESIAN_POINT ( 'NONE',  ( 15.00000000000000000, 246.8500000000000227, 0.000000000000000000 ) ) ;
#26589 = CARTESIAN_POINT ( 'NONE',  ( 15.24356964374999990, 0.000000000000000000, -2.053124999385480542 ) ) ;
#26590 = CARTESIAN_POINT ( 'NONE',  ( 8.715434833792128799, 65.13981371789854791, -8.962234695871567070 ) ) ;
#26591 = CARTESIAN_POINT ( 'NONE',  ( 27.24356964374999635, 198.3218750006145399, -15.72908226750539029 ) ) ;
#26592 = ORIENTED_EDGE ( 'NONE', *, *, #23035, .T. ) ;
#26593 = ORIENTED_EDGE ( 'NONE', *, *, #10840, .F. ) ;
#26594 = CARTESIAN_POINT ( 'NONE',  ( 15.24356964374999990, 3.323476615752268604, -4.228124999385472371 ) ) ;
#26595 = CARTESIAN_POINT ( 'NONE',  ( 24.65789917220240213, 0.000000000000000000, 160.6522583305284968 ) ) ;
#26596 = CARTESIAN_POINT ( 'NONE',  ( 26.75643035624999655, 247.2343750006145058, 3.323476615752267715 ) ) ;
#26597 = CARTESIAN_POINT ( 'NONE',  ( -0.1745138560725500443, 38.01018628210144357, 12.50000000000000355 ) ) ;
#26598 = EDGE_CURVE ( 'NONE', #2631, #15329, #7463, .T. ) ;
#26599 = CARTESIAN_POINT ( 'NONE',  ( -44.85044563604515844, 205.1570982666397072, -4.673758765035155527 ) ) ;
#26600 = CARTESIAN_POINT ( 'NONE',  ( 21.00000000000001776, 209.9999999999999432, -5.999999999999996447 ) ) ;
#26601 = CARTESIAN_POINT ( 'NONE',  ( -65.23586230271183695, 206.8500491399821328, 5.686928522499748340 ) ) ;
#26602 = SURFACE_STYLE_FILL_AREA ( #4045 ) ;
#26603 = CARTESIAN_POINT ( 'NONE',  ( 36.76257920565016235, 3.464101615137755275, 161.3248252729892727 ) ) ;
#26604 = CARTESIAN_POINT ( 'NONE',  ( -12.46528703574811558, 79.80231371789857064, 2.660918448318003726 ) ) ;
#26605 = ADVANCED_FACE ( 'NONE', ( #33801 ), #19410, .F. ) ;
#26606 = CARTESIAN_POINT ( 'NONE',  ( -65.83705436395491972, 206.7903428501026042, -3.378800118222489157 ) ) ;
#26608 = EDGE_CURVE ( 'NONE', #16385, #8744, #27612, .T. ) ;
#26607 = CARTESIAN_POINT ( 'NONE',  ( -35.75372103062156981, 218.5309553116391896, -2.162041339862839084 ) ) ;
#26609 = CARTESIAN_POINT ( 'NONE',  ( 15.24356964374999990, 3.323476615752268604, -5.690624999385482496 ) ) ;
#26610 = CARTESIAN_POINT ( 'NONE',  ( 16.56230152254412147, 6.928203230275514990, -0.5625000000000507372 ) ) ;
#26611 = CARTESIAN_POINT ( 'NONE',  ( -0.1745138560722442889, 63.98981371789855643, -15.50000000000000533 ) ) ;
#26612 = CARTESIAN_POINT ( 'NONE',  ( -54.35044563604515844, 203.6929966515019430, -6.137860380172892150 ) ) ;
#26613 = CARTESIAN_POINT ( 'NONE',  ( 10.56230152254410726, 0.000000000000000000, -9.900000000000048317 ) ) ;
#26614 = CARTESIAN_POINT ( 'NONE',  ( -2.311890736173176641, 79.12268628210145494, -12.53471296425194836 ) ) ;
#26615 = CARTESIAN_POINT ( 'NONE',  ( -2.908627838312119351, 42.32268628210145067, -15.53471296425195369 ) ) ;
#26616 = CYLINDRICAL_SURFACE ( 'NONE', #5333, 5.999999999999994671 ) ;
#26617 = CARTESIAN_POINT ( 'NONE',  ( 36.82137784845814821, 3.604726614523243278, 159.2022485878779889 ) ) ;
#26618 = CARTESIAN_POINT ( 'NONE',  ( 6.092822981423978490, 52.38518628210145778, -14.25334919248782306 ) ) ;
#26619 = CARTESIAN_POINT ( 'NONE',  ( 24.00000000000000000, 247.0562500012290457, 5.196152422706629359 ) ) ;
#26620 = CARTESIAN_POINT ( 'NONE',  ( 13.44051670066911619, -5.407089921784859143, -9.515624999385547511 ) ) ;
#26621 = DIRECTION ( 'NONE',  ( 0.000000000000000000, 0.000000000000000000, 1.000000000000000000 ) ) ;
#26622 = CARTESIAN_POINT ( 'NONE',  ( -51.38913769728823411, 206.8500491399821044, -5.686928522499717253 ) ) ;
#26623 = CARTESIAN_POINT ( 'NONE',  ( 22.60769515458672885, 241.3736538117966859, -5.999999999999998224 ) ) ;
#26624 = CARTESIAN_POINT ( 'NONE',  ( 11.61527771782819940, 16.73518628210143788, -4.622313124798573369 ) ) ;
#26625 = CARTESIAN_POINT ( 'NONE',  ( 0.1745138560723095977, 142.1898137178985451, 9.500000000000005329 ) ) ;
#26626 = CARTESIAN_POINT ( 'NONE',  ( 18.12178482187499640, 245.7343750006145342, -4.985214923628404904 ) ) ;
#26627 = AXIS2_PLACEMENT_3D ( 'NONE', #9335, #6488, #29603 ) ;
#26628 = ORIENTED_EDGE ( 'NONE', *, *, #36955, .T. ) ;
#26629 = CARTESIAN_POINT ( 'NONE',  ( 26.99999999999999645, -3.464101615137751278, -7.012500000000010836 ) ) ;
#26630 = DIRECTION ( 'NONE',  ( 0.000000000000000000, -1.000000000000000000, 0.000000000000000000 ) ) ;
#26631 = CARTESIAN_POINT ( 'NONE',  ( 10.56230152254410903, 0.000000000000000000, -3.487499998771015353 ) ) ;
#26632 = CARTESIAN_POINT ( 'NONE',  ( 22.80587116629410716, 7.646167579472015790E-16, -4.415624999385525662 ) ) ;
#26633 = CARTESIAN_POINT ( 'NONE',  ( 24.98803303140584120, 3.604726614523236616, 167.2203538558741798 ) ) ;
#26634 = CARTESIAN_POINT ( 'NONE',  ( 24.00000000000000000, 240.2500000000000000, 5.196152422706629359 ) ) ;
#26635 = CARTESIAN_POINT ( 'NONE',  ( -47.00000000000000711, 244.5000000000000000, 2.500000000000001776 ) ) ;
#26636 = CARTESIAN_POINT ( 'NONE',  ( 11.48171059495397728, 45.48518628210145209, 4.944772684328674117 ) ) ;
#26637 = VERTEX_POINT ( 'NONE', #10482 ) ;
#26638 = ORIENTED_EDGE ( 'NONE', *, *, #34155, .T. ) ;
#26639 = LINE ( 'NONE', #32331, #29720 ) ;
#26640 = PLANE ( 'NONE',  #33450 ) ;
#26641 = FACE_OUTER_BOUND ( 'NONE', #30982, .T. ) ;
#26642 = CARTESIAN_POINT ( 'NONE',  ( 24.77882776526536190, -3.464101615138098111, 162.0344784741307649 ) ) ;
#26643 = CARTESIAN_POINT ( 'NONE',  ( 26.75643035624999655, -3.323476615752267715, -6.253124999385469174 ) ) ;
#26644 = VECTOR ( 'NONE', #8229, 1000.000000000000000 ) ;
#26645 = CARTESIAN_POINT ( 'NONE',  ( 2.311890736173175753, 102.1226862821014691, 12.53471296425194836 ) ) ;
#26646 = CARTESIAN_POINT ( 'NONE',  ( -8.632099005475794229, 14.25231371789853618, 13.23911966647199812 ) ) ;
#26647 = DIRECTION ( 'NONE',  ( 0.000000000000000000, 0.000000000000000000, 1.000000000000000000 ) ) ;
#26648 = CARTESIAN_POINT ( 'NONE',  ( 26.75643035624999655, 240.5968750006145456, 3.323476615752267715 ) ) ;
#26649 = CARTESIAN_POINT ( 'NONE',  ( -66.62127896937849414, 214.5309553116392749, 1.090244570138288127 ) ) ;
#26650 = DIRECTION ( 'NONE',  ( 0.08715574274765150453, 0.000000000000000000, 0.9961946980917461003 ) ) ;
#26651 = CARTESIAN_POINT ( 'NONE',  ( 25.45210587809749825, 0.000000000000000000, 169.7300825181138748 ) ) ;
#26652 = CARTESIAN_POINT ( 'NONE',  ( -11.61527771782809282, 135.8648137178985849, -4.622313124798832717 ) ) ;
#26653 = CARTESIAN_POINT ( 'NONE',  ( -55.94122103062156270, 208.3738570449993404, -6.530955311639226935 ) ) ;
#26654 = CARTESIAN_POINT ( 'NONE',  ( -32.38169563604516554, 210.1155267958018271, 8.500000000000003553 ) ) ;
#26655 = DIRECTION ( 'NONE',  ( 0.000000000000000000, 0.000000000000000000, 1.000000000000000000 ) ) ;
#26656=STYLED_ITEM('',(#37535),#20661);
#26657 = CARTESIAN_POINT ( 'NONE',  ( 15.24356964374999990, 3.323476615752268604, -0.2906249993854698177 ) ) ;
#26658 = CARTESIAN_POINT ( 'NONE',  ( -13.62178482187500528, 198.8281250006145342, -23.59362340125807123 ) ) ;
#26659 = CARTESIAN_POINT ( 'NONE',  ( 8.632099005475788900, 129.2523137178985451, -13.23911966647199812 ) ) ;
#26660 = CARTESIAN_POINT ( 'NONE',  ( -57.31919563604516554, 216.5000000000000000, -0.1155267958017906493 ) ) ;
#26661 = ORIENTED_EDGE ( 'NONE', *, *, #5997, .T. ) ;
#26662 = CARTESIAN_POINT ( 'NONE',  ( 8.715434833791931624, 46.06018628210144072, 8.962234695871760692 ) ) ;
#26663 = CARTESIAN_POINT ( 'NONE',  ( 24.00000000000000000, 245.2562500012290627, 5.196152422706629359 ) ) ;
#26664 = CARTESIAN_POINT ( 'NONE',  ( -3.253724281355068545E-15, 198.6500000012290172, -27.00000000000000355 ) ) ;
#26665 = CARTESIAN_POINT ( 'NONE',  ( 34.28996860281051795, -5.407089921784861808, 166.0865723713108366 ) ) ;
#26666 = CARTESIAN_POINT ( 'NONE',  ( 15.50000000000000533, 109.3101862821014549, 0.1745138560725827404 ) ) ;
#26667 = CARTESIAN_POINT ( 'NONE',  ( -65.24330436395489130, 210.1155267958017134, -6.500000000000000888 ) ) ;
#26668 = CARTESIAN_POINT ( 'NONE',  ( 16.56230152254411436, 7.209453229046475009, -1.603124999385524108 ) ) ;
#26669 = CARTESIAN_POINT ( 'NONE',  ( -9.500000000000005329, 49.51018628210145067, -0.1745138560725176813 ) ) ;
#26670 = CYLINDRICAL_SURFACE ( 'NONE', #26739, 25.00000000000000000 ) ;
#26671 = CARTESIAN_POINT ( 'NONE',  ( -56.70466238434235606, 244.2363183625454894, -7.500000000000000000 ) ) ;
#26672 = CARTESIAN_POINT ( 'NONE',  ( 10.49813415415989581, 100.9726862821014635, 7.228626920339068285 ) ) ;
#26673 = CARTESIAN_POINT ( 'NONE',  ( 27.00000000000000355, 199.7750000000000057, -3.306546357697854128E-15 ) ) ;
#26674 = CYLINDRICAL_SURFACE ( 'NONE', #21049, 5.999999999999999112 ) ;
#26675 = FACE_OUTER_BOUND ( 'NONE', #5281, .T. ) ;
#26676 = CARTESIAN_POINT ( 'NONE',  ( 24.47817193633207822, 3.604726614523236616, 161.3926148720374556 ) ) ;
#26677 = CARTESIAN_POINT ( 'NONE',  ( 21.00000000000000000, -6.928203230275506996, -0.3375000000000047962 ) ) ;
#26678 = DIRECTION ( 'NONE',  ( 0.000000000000000000, 0.000000000000000000, 1.000000000000000000 ) ) ;
#26679 = CARTESIAN_POINT ( 'NONE',  ( 24.83278686463658502, -3.604726614523244610, 165.4458820498982732 ) ) ;
#26680 = PRODUCT_DEFINITION_CONTEXT ( 'detailed design', #9320, 'design' ) ;
#26681 = CARTESIAN_POINT ( 'NONE',  ( 30.88019288723065259, -6.928203230275514990, 162.9311214624256365 ) ) ;
#26682 = CYLINDRICAL_SURFACE ( 'NONE', #3533, 5.999999999999994671 ) ;
#26683 = CARTESIAN_POINT ( 'NONE',  ( 21.00000000000000000, 248.0875000000000057, -6.928203230275506996 ) ) ;
#26684 = CARTESIAN_POINT ( 'NONE',  ( -13.62178482187498396, 195.8281250006145342, 23.59362340125808188 ) ) ;
#26685 = CARTESIAN_POINT ( 'NONE',  ( -10.49813415416004858, 106.8273137178985479, 7.228626920338839135 ) ) ;
#26686 = CARTESIAN_POINT ( 'NONE',  ( 10.49813415415989581, 110.1726862821014521, 7.228626920339069173 ) ) ;
#26687 = AXIS2_PLACEMENT_3D ( 'NONE', #20139, #20520, #402 ) ;
#26688 = ORIENTED_EDGE ( 'NONE', *, *, #14814, .F. ) ;
#26689 = CARTESIAN_POINT ( 'NONE',  ( 13.62178482187499640, 195.6031250006145115, -23.59362340125807123 ) ) ;
#26690 = CARTESIAN_POINT ( 'NONE',  ( 15.24356964374999990, 240.2593750006145115, -3.323476615752268604 ) ) ;
#26691 = CARTESIAN_POINT ( 'NONE',  ( -15.53471296425188442, 71.17731371789855643, -2.908627838312459080 ) ) ;
#26692 = CARTESIAN_POINT ( 'NONE',  ( 26.75643035624999655, 7.049594010296217766E-16, -3.178124999385495641 ) ) ;
#26693 = CARTESIAN_POINT ( 'NONE',  ( 15.24356964374999990, 248.0218750006145285, -3.323476615752268604 ) ) ;
#26694 = CARTESIAN_POINT ( 'NONE',  ( 6.840914352312096547, 108.1601862821014635, -6.594114490232313663 ) ) ;
#26695 = LINE ( 'NONE', #18188, #18596 ) ;
#26696 = CARTESIAN_POINT ( 'NONE',  ( -9.500000000000005329, 80.08981371789856496, 0.1745138560723101806 ) ) ;
#26697 = CARTESIAN_POINT ( 'NONE',  ( 22.80587116629411071, 3.604726614523238837, -6.178124999385540050 ) ) ;
#26698 = CARTESIAN_POINT ( 'NONE',  ( -9.500000000000005329, 107.6898137178985735, 0.1745138560723101806 ) ) ;
#26699 = CARTESIAN_POINT ( 'NONE',  ( 18.12178482187499640, 242.9218750006145058, -4.985214923628404904 ) ) ;
#26700 = CARTESIAN_POINT ( 'NONE',  ( -8.962234695871565293, 53.63981371789855501, -8.715434833792128799 ) ) ;
#26701 =( BOUNDED_SURFACE ( )  B_SPLINE_SURFACE ( 1, 2, ( 
 ( #31211, #1654, #16635, #36705, #27992, #5240, #21763, #4867, #33682, #33494, #33313, #28177, #7353, #19672, #21949, #10744, #24957, #4498, #2395, #16075, #5052, #36515, #36327, #18926, #30477, #27624, #13228, #7540, #10559, #19112, #24777, #22317, #10374, #7722, #30843, #2207, #13788, #30662, #16447, #33869, #4679, #36884, #2022, #13600, #22136, #7911, #10186, #25150, #16261, #27811, #1839, #19484, #16817, #22505, #34052, #28359, #13408, #31031, #19305, #13969, #25518, #16997, #5416, #37071, #11117, #28537, #8281, #22694, #34238, #19854, #31397, #6627, #18013, #21050, #7016, #32964, #18584, #35426, #30126, #21608, #27468, #30315, #27278, #9287, #1121, #29938, #15539, #29743, #23692, #18203, #32777, #32588, #29557, #12311, #27097, #18776, #10028, #6440, #4158, #23885, #21238, #3776, #9474, #12687, #24443, #24259, #15350, #26904, #35802, #20861, #32400, #7203, #12875, #9845, #3965, #1308, #21423, #15728, #33157, #35992, #4339, #15919, #12118, #933, #35237, #3596, #15160, #26709, #740, #6813, #12506, #9661, #24070, #35616, #18388, #4712, #7383, #5274, #36360, #1494, #19336, #7754, #1683, #36548, #36173, #25185, #22537, #16106, #19706, #33528, #30875, #10409, #10219, #2242, #1870, #30510, #16854, #4530, #21983, #13821, #13069, #25368, #24625, #16292, #7942, #7570, #27657, #19145, #28212, #21793, #31245, #27839, #36738, #13258, #36915, #4898, #33346, #28025, #10963, #10590, #34084, #18955, #19518, #10777, #22169, #24808, #22351, #2058, #30695, #13441, #8135, #24991, #33713, #31064, #16479, #13636, #33900, #5088, #16666, #20253, #23459, #20627, #14745, #17598, #34458, #34636, #31612, #31793, #25928, #23092, #34823, #11705, #11891, #28573, #11154, #6014, #14556, #32169, #35013, #34274, #31986, #8499, #22912, #20067, #5830, #17409, #14372, #14001, #17035, #11340, #23280, #2800, #5639, #8317, #6207, #28391, #25553, #19889, #17223, #28761, #37472, #11522, #9056, #8866, #28950, #2428, #37106, #22727, #20443, #2987, #31431, #5452, #26109, #29130, #142, #2612, #25740, #3171, #14188, #37292, #8682, #26291, #326, #16517, #7427, #15959, #27513, #36215, #30358 ),
 ( #10819, #22390, #27697, #1910, #30916, #1725, #25225, #36590, #25031, #30735, #28064, #33200, #10629, #21833, #24851, #10258, #19374, #25407, #36774, #33940, #13859, #31104, #22208, #33757, #1536, #2282, #2099, #7797, #5125, #36958, #4935, #18996, #33574, #13479, #7982, #4382, #13294, #13108, #4570, #13677, #19555, #16705, #30553, #28253, #11004, #7240, #18815, #24663, #33387, #16147, #36400, #10445, #22021, #7610, #19186, #16330, #4757, #27878, #22761, #25962, #29166, #20478, #16890, #28982, #34310, #31649, #31465, #8354, #19636, #34861, #11557, #25773, #28610, #23131, #31284, #5312, #17634, #23314, #34674, #14406, #11745, #8719, #5487, #11187, #17070, #5865, #34493, #2647, #2467, #14784, #26328, #19747, #14041, #14223, #37325, #11375, #22947, #20291, #6048, #37145, #3210, #8534, #31831, #19927, #28426, #8901, #20100, #25590, #364, #5676, #17257, #32017, #22576, #34122, #8172, #28796, #3023, #2834, #17443, #14593, #26145, #179, #4154, #26704, #9656, #14968, #35799, #3771, #9094, #929, #12684, #9469, #24255, #32209, #18384, #35612, #21044, #23686, #32773, #12499, #23497, #735, #9841, #12113, #29552, #3962, #546, #3591, #17823, #35046, #29360, #15345, #7012, #15725, #21418, #1118, #18008, #18198, #15153, #26899, #32581, #6622, #29934, #6808, #32961, #35232, #6246, #27093, #21234, #27275, #18581, #3399, #15536, #12306, #6434, #23880, #30123, #29737, #35418, #20855, #9282, #32394, #11928, #24066, #20663, #26516, #31060, #5084, #35988, #30312, #18952, #21790, #7381, #30506, #22346, #22165, #27835, #16662, #1303, #36543, #16475, #13436, #19514, #36170, #10586, #12872, #4336, #10024, #27464, #24985, #1865, #24439, #13255, #19141, #7938, #4526, #7199, #21605, #10216, #33154, #30690, #7566, #1491, #36356, #18771, #15915, #24804, #4708, #13065, #16102, #24622, #33342, #27654, #1680, #16288, #33709, #10403, #21978, #33523, #7749, #33896, #19332, #30871, #4894, #28020, #2053, #13631, #25181, #36733, #10773, #31981, #31241, #11149, #28945, #28208, #14552, #6010, #5448, #34632, #37100, #5270, #34269, #17405, #2238, #20438, #17030, #25923, #16849, #26105 ) ),
 .UNSPECIFIED., .F., .F., .F. ) 
 B_SPLINE_SURFACE_WITH_KNOTS ( ( 2, 2 ),
 ( 3, 2, 2, 2, 2, 2, 2, 2, 2, 2, 2, 2, 2, 2, 2, 2, 2, 2, 2, 2, 2, 2, 2, 2, 2, 2, 2, 2, 2, 2, 2, 2, 2, 2, 2, 2, 2, 2, 2, 2, 2, 2, 2, 2, 2, 2, 2, 2, 2, 2, 2, 2, 2, 2, 2, 2, 2, 2, 2, 2, 2, 2, 2, 2, 2, 2, 2, 2, 2, 2, 2, 2, 2, 2, 2, 2, 2, 2, 2, 2, 2, 2, 2, 2, 2, 2, 2, 2, 2, 2, 2, 2, 2, 2, 2, 2, 2, 2, 2, 2, 2, 2, 2, 2, 2, 2, 2, 2, 2, 2, 2, 2, 2, 2, 2, 2, 2, 2, 2, 2, 2, 2, 2, 2, 2, 2, 2, 2, 2, 2, 2, 2, 2, 2, 3 ),
 ( 0.000000000000000000, 1.000000000000000000 ),
 ( 0.000000000000000000, 0.007246376811594202987, 0.01449275362318840597, 0.02173913043478260809, 0.02898550724637681195, 0.03623188405797101580, 0.04347826086956521618, 0.05072463768115942351, 0.05797101449275362389, 0.06521739130434782428, 0.07246376811594203160, 0.07971014492753622505, 0.08695652173913043237, 0.09420289855072463969, 0.1014492753623188470, 0.1086956521739130405, 0.1159420289855072478, 0.1231884057971014551, 0.1304347826086956486, 0.1376811594202898559, 0.1449275362318840632, 0.1521739130434782705, 0.1594202898550724501, 0.1666666666666666574, 0.1739130434782608647, 0.1811594202898550721, 0.1884057971014492794, 0.1956521739130434867, 0.2028985507246376940, 0.2101449275362318736, 0.2173913043478260809, 0.2246376811594202882, 0.2318840579710144956, 0.2391304347826087029, 0.2463768115942029102, 0.2536231884057971175, 0.2608695652173912971, 0.2681159420289855322, 0.2753623188405797118, 0.2826086956521738913, 0.2898550724637681264, 0.2971014492753623060, 0.3043478260869565410, 0.3115942028985507206, 0.3188405797101449002, 0.3260869565217391353, 0.3333333333333333148, 0.3405797101449275499, 0.3478260869565217295, 0.3550724637681159646, 0.3623188405797101441, 0.3695652173913043237, 0.3768115942028985588, 0.3840579710144927383, 0.3913043478260869734, 0.3985507246376811530, 0.4057971014492753881, 0.4130434782608695676, 0.4202898550724637472, 0.4275362318840579823, 0.4347826086956521618, 0.4420289855072463969, 0.4492753623188405765, 0.4565217391304347561, 0.4637681159420289911, 0.4710144927536231707, 0.4782608695652174058, 0.4855072463768115854, 0.4927536231884058204, 0.5000000000000000000, 0.5072463768115942351, 0.5144927536231883591, 0.5217391304347825942, 0.5289855072463768293, 0.5362318840579710644, 0.5434782608695651884, 0.5507246376811594235, 0.5579710144927536586, 0.5652173913043477826, 0.5724637681159420177, 0.5797101449275362528, 0.5869565217391304879, 0.5942028985507246119, 0.6014492753623188470, 0.6086956521739130821, 0.6159420289855072062, 0.6231884057971014412, 0.6304347826086956763, 0.6376811594202898004, 0.6449275362318840354, 0.6521739130434782705, 0.6594202898550725056, 0.6666666666666666297, 0.6739130434782608647, 0.6811594202898550998, 0.6884057971014492239, 0.6956521739130434590, 0.7028985507246376940, 0.7101449275362319291, 0.7173913043478260532, 0.7246376811594202882, 0.7318840579710145233, 0.7391304347826086474, 0.7463768115942028825, 0.7536231884057971175, 0.7608695652173913526, 0.7681159420289854767, 0.7753623188405797118, 0.7826086956521739468, 0.7898550724637680709, 0.7971014492753623060, 0.8043478260869565410, 0.8115942028985507761, 0.8188405797101449002, 0.8260869565217391353, 0.8333333333333333703, 0.8405797101449274944, 0.8478260869565217295, 0.8550724637681159646, 0.8623188405797101996, 0.8695652173913043237, 0.8768115942028985588, 0.8840579710144927938, 0.8913043478260869179, 0.8985507246376811530, 0.9057971014492753881, 0.9130434782608695121, 0.9202898550724637472, 0.9275362318840579823, 0.9347826086956522174, 0.9420289855072463414, 0.9492753623188405765, 0.9565217391304348116, 0.9637681159420289356, 0.9662082944262200268 ),
 .UNSPECIFIED. ) 
 GEOMETRIC_REPRESENTATION_ITEM ( )  RATIONAL_B_SPLINE_SURFACE ( (
 ( 1.000000000000000000, 0.8660254037844387076, 1.000000000000000000, 0.8660254037844387076, 1.000000000000000000, 0.8660254037844387076, 1.000000000000000000, 0.8660254037844387076, 1.000000000000000000, 0.8660254037844387076, 1.000000000000000000, 0.8660254037844387076, 1.000000000000000000, 0.8660254037844387076, 1.000000000000000000, 0.8660254037844387076, 1.000000000000000000, 0.8660254037844387076, 1.000000000000000000, 0.8660254037844387076, 1.000000000000000000, 0.8660254037844387076, 1.000000000000000000, 0.8660254037844387076, 1.000000000000000000, 0.8660254037844387076, 1.000000000000000000, 0.8660254037844387076, 1.000000000000000000, 0.8660254037844387076, 1.000000000000000000, 0.8660254037844387076, 1.000000000000000000, 0.8660254037844387076, 1.000000000000000000, 0.8660254037844387076, 1.000000000000000000, 0.8660254037844387076, 1.000000000000000000, 0.8660254037844387076, 1.000000000000000000, 0.8660254037844387076, 1.000000000000000000, 0.8660254037844387076, 1.000000000000000000, 0.8660254037844387076, 1.000000000000000000, 0.8660254037844387076, 1.000000000000000000, 0.8660254037844387076, 1.000000000000000000, 0.8660254037844387076, 1.000000000000000000, 0.8660254037844387076, 1.000000000000000000, 0.8660254037844387076, 1.000000000000000000, 0.8660254037844387076, 1.000000000000000000, 0.8660254037844387076, 1.000000000000000000, 0.8660254037844387076, 1.000000000000000000, 0.8660254037844387076, 1.000000000000000000, 0.8660254037844387076, 1.000000000000000000, 0.8660254037844387076, 1.000000000000000000, 0.8660254037844387076, 1.000000000000000000, 0.8660254037844387076, 1.000000000000000000, 0.8660254037844387076, 1.000000000000000000, 0.8660254037844387076, 1.000000000000000000, 0.8660254037844387076, 1.000000000000000000, 0.8660254037844387076, 1.000000000000000000, 0.8660254037844387076, 1.000000000000000000, 0.8660254037844387076, 1.000000000000000000, 0.8660254037844387076, 1.000000000000000000, 0.8660254037844387076, 1.000000000000000000, 0.8660254037844387076, 1.000000000000000000, 0.8660254037844387076, 1.000000000000000000, 0.8660254037844387076, 1.000000000000000000, 0.8660254037844387076, 1.000000000000000000, 0.8660254037844387076, 1.000000000000000000, 0.8660254037844387076, 1.000000000000000000, 0.8660254037844387076, 1.000000000000000000, 0.8660254037844387076, 1.000000000000000000, 0.8660254037844387076, 1.000000000000000000, 0.8660254037844387076, 1.000000000000000000, 0.8660254037844387076, 1.000000000000000000, 0.8660254037844387076, 1.000000000000000000, 0.8660254037844387076, 1.000000000000000000, 0.8660254037844387076, 1.000000000000000000, 0.8660254037844387076, 1.000000000000000000, 0.8660254037844387076, 1.000000000000000000, 0.8660254037844387076, 1.000000000000000000, 0.8660254037844387076, 1.000000000000000000, 0.8660254037844387076, 1.000000000000000000, 0.8660254037844387076, 1.000000000000000000, 0.8660254037844387076, 1.000000000000000000, 0.8660254037844387076, 1.000000000000000000, 0.8660254037844387076, 1.000000000000000000, 0.8660254037844387076, 1.000000000000000000, 0.8660254037844387076, 1.000000000000000000, 0.8660254037844387076, 1.000000000000000000, 0.8660254037844387076, 1.000000000000000000, 0.8660254037844387076, 1.000000000000000000, 0.8660254037844387076, 1.000000000000000000, 0.8660254037844387076, 1.000000000000000000, 0.8660254037844387076, 1.000000000000000000, 0.8660254037844387076, 1.000000000000000000, 0.8660254037844387076, 1.000000000000000000, 0.8660254037844387076, 1.000000000000000000, 0.8660254037844387076, 1.000000000000000000, 0.8660254037844387076, 1.000000000000000000, 0.8660254037844387076, 1.000000000000000000, 0.8660254037844387076, 1.000000000000000000, 0.8660254037844387076, 1.000000000000000000, 0.8660254037844387076, 1.000000000000000000, 0.8660254037844387076, 1.000000000000000000, 0.8660254037844387076, 1.000000000000000000, 0.8660254037844387076, 1.000000000000000000, 0.8660254037844387076, 1.000000000000000000, 0.8660254037844387076, 1.000000000000000000, 0.8660254037844387076, 1.000000000000000000, 0.8660254037844387076, 1.000000000000000000, 0.8660254037844387076, 1.000000000000000000, 0.8660254037844387076, 1.000000000000000000, 0.8660254037844387076, 1.000000000000000000, 0.8660254037844387076, 1.000000000000000000, 0.8660254037844387076, 1.000000000000000000, 0.8660254037844387076, 1.000000000000000000, 0.8660254037844387076, 1.000000000000000000, 0.8660254037844387076, 1.000000000000000000, 0.8660254037844387076, 1.000000000000000000, 0.8660254037844387076, 1.000000000000000000, 0.8660254037844387076, 1.000000000000000000, 0.8660254037844387076, 1.000000000000000000, 0.8660254037844387076, 1.000000000000000000, 0.8660254037844387076, 1.000000000000000000, 0.8660254037844387076, 1.000000000000000000, 0.8660254037844387076, 1.000000000000000000, 0.8660254037844387076, 1.000000000000000000, 0.8660254037844387076, 1.000000000000000000, 0.8660254037844387076, 1.000000000000000000, 0.8660254037844387076, 1.000000000000000000, 0.8660254037844387076, 1.000000000000000000, 0.8660254037844387076, 1.000000000000000000, 0.8660254037844387076, 1.000000000000000000, 0.8660254037844387076, 1.000000000000000000, 0.8660254037844387076, 1.000000000000000000, 0.8660254037844387076, 1.000000000000000000, 0.8660254037844387076, 1.000000000000000000, 0.8660254037844387076, 1.000000000000000000, 0.8660254037844387076, 1.000000000000000000, 0.8660254037844387076, 1.000000000000000000, 0.8660254037844387076, 1.000000000000000000, 0.8660254037844387076, 1.000000000000000000, 0.8660254037844387076, 1.000000000000000000, 0.8660254037844387076, 1.000000000000000000, 0.8660254037844387076, 1.000000000000000000, 0.8660254037844387076, 1.000000000000000000, 0.8660254037844387076, 1.000000000000000000, 0.8660254037844387076, 1.000000000000000000, 0.8660254037844387076, 1.000000000000000000, 0.8660254037844387076, 1.000000000000000000, 0.8660254037844387076, 1.000000000000000000, 0.8660254037844387076, 1.000000000000000000, 0.9548847740583508159, 0.9401541683247176540),
 ( 1.000000000000000000, 0.8660254037844387076, 1.000000000000000000, 0.8660254037844387076, 1.000000000000000000, 0.8660254037844387076, 1.000000000000000000, 0.8660254037844387076, 1.000000000000000000, 0.8660254037844387076, 1.000000000000000000, 0.8660254037844387076, 1.000000000000000000, 0.8660254037844387076, 1.000000000000000000, 0.8660254037844387076, 1.000000000000000000, 0.8660254037844387076, 1.000000000000000000, 0.8660254037844387076, 1.000000000000000000, 0.8660254037844387076, 1.000000000000000000, 0.8660254037844387076, 1.000000000000000000, 0.8660254037844387076, 1.000000000000000000, 0.8660254037844387076, 1.000000000000000000, 0.8660254037844387076, 1.000000000000000000, 0.8660254037844387076, 1.000000000000000000, 0.8660254037844387076, 1.000000000000000000, 0.8660254037844387076, 1.000000000000000000, 0.8660254037844387076, 1.000000000000000000, 0.8660254037844387076, 1.000000000000000000, 0.8660254037844387076, 1.000000000000000000, 0.8660254037844387076, 1.000000000000000000, 0.8660254037844387076, 1.000000000000000000, 0.8660254037844387076, 1.000000000000000000, 0.8660254037844387076, 1.000000000000000000, 0.8660254037844387076, 1.000000000000000000, 0.8660254037844387076, 1.000000000000000000, 0.8660254037844387076, 1.000000000000000000, 0.8660254037844387076, 1.000000000000000000, 0.8660254037844387076, 1.000000000000000000, 0.8660254037844387076, 1.000000000000000000, 0.8660254037844387076, 1.000000000000000000, 0.8660254037844387076, 1.000000000000000000, 0.8660254037844387076, 1.000000000000000000, 0.8660254037844387076, 1.000000000000000000, 0.8660254037844387076, 1.000000000000000000, 0.8660254037844387076, 1.000000000000000000, 0.8660254037844387076, 1.000000000000000000, 0.8660254037844387076, 1.000000000000000000, 0.8660254037844387076, 1.000000000000000000, 0.8660254037844387076, 1.000000000000000000, 0.8660254037844387076, 1.000000000000000000, 0.8660254037844387076, 1.000000000000000000, 0.8660254037844387076, 1.000000000000000000, 0.8660254037844387076, 1.000000000000000000, 0.8660254037844387076, 1.000000000000000000, 0.8660254037844387076, 1.000000000000000000, 0.8660254037844387076, 1.000000000000000000, 0.8660254037844387076, 1.000000000000000000, 0.8660254037844387076, 1.000000000000000000, 0.8660254037844387076, 1.000000000000000000, 0.8660254037844387076, 1.000000000000000000, 0.8660254037844387076, 1.000000000000000000, 0.8660254037844387076, 1.000000000000000000, 0.8660254037844387076, 1.000000000000000000, 0.8660254037844387076, 1.000000000000000000, 0.8660254037844387076, 1.000000000000000000, 0.8660254037844387076, 1.000000000000000000, 0.8660254037844387076, 1.000000000000000000, 0.8660254037844387076, 1.000000000000000000, 0.8660254037844387076, 1.000000000000000000, 0.8660254037844387076, 1.000000000000000000, 0.8660254037844387076, 1.000000000000000000, 0.8660254037844387076, 1.000000000000000000, 0.8660254037844387076, 1.000000000000000000, 0.8660254037844387076, 1.000000000000000000, 0.8660254037844387076, 1.000000000000000000, 0.8660254037844387076, 1.000000000000000000, 0.8660254037844387076, 1.000000000000000000, 0.8660254037844387076, 1.000000000000000000, 0.8660254037844387076, 1.000000000000000000, 0.8660254037844387076, 1.000000000000000000, 0.8660254037844387076, 1.000000000000000000, 0.8660254037844387076, 1.000000000000000000, 0.8660254037844387076, 1.000000000000000000, 0.8660254037844387076, 1.000000000000000000, 0.8660254037844387076, 1.000000000000000000, 0.8660254037844387076, 1.000000000000000000, 0.8660254037844387076, 1.000000000000000000, 0.8660254037844387076, 1.000000000000000000, 0.8660254037844387076, 1.000000000000000000, 0.8660254037844387076, 1.000000000000000000, 0.8660254037844387076, 1.000000000000000000, 0.8660254037844387076, 1.000000000000000000, 0.8660254037844387076, 1.000000000000000000, 0.8660254037844387076, 1.000000000000000000, 0.8660254037844387076, 1.000000000000000000, 0.8660254037844387076, 1.000000000000000000, 0.8660254037844387076, 1.000000000000000000, 0.8660254037844387076, 1.000000000000000000, 0.8660254037844387076, 1.000000000000000000, 0.8660254037844387076, 1.000000000000000000, 0.8660254037844387076, 1.000000000000000000, 0.8660254037844387076, 1.000000000000000000, 0.8660254037844387076, 1.000000000000000000, 0.8660254037844387076, 1.000000000000000000, 0.8660254037844387076, 1.000000000000000000, 0.8660254037844387076, 1.000000000000000000, 0.8660254037844387076, 1.000000000000000000, 0.8660254037844387076, 1.000000000000000000, 0.8660254037844387076, 1.000000000000000000, 0.8660254037844387076, 1.000000000000000000, 0.8660254037844387076, 1.000000000000000000, 0.8660254037844387076, 1.000000000000000000, 0.8660254037844387076, 1.000000000000000000, 0.8660254037844387076, 1.000000000000000000, 0.8660254037844387076, 1.000000000000000000, 0.8660254037844387076, 1.000000000000000000, 0.8660254037844387076, 1.000000000000000000, 0.8660254037844387076, 1.000000000000000000, 0.8660254037844387076, 1.000000000000000000, 0.8660254037844387076, 1.000000000000000000, 0.8660254037844387076, 1.000000000000000000, 0.8660254037844387076, 1.000000000000000000, 0.8660254037844387076, 1.000000000000000000, 0.8660254037844387076, 1.000000000000000000, 0.8660254037844387076, 1.000000000000000000, 0.8660254037844387076, 1.000000000000000000, 0.8660254037844387076, 1.000000000000000000, 0.8660254037844387076, 1.000000000000000000, 0.8660254037844387076, 1.000000000000000000, 0.8660254037844387076, 1.000000000000000000, 0.8660254037844387076, 1.000000000000000000, 0.8660254037844387076, 1.000000000000000000, 0.8660254037844387076, 1.000000000000000000, 0.8660254037844387076, 1.000000000000000000, 0.8660254037844387076, 1.000000000000000000, 0.8660254037844387076, 1.000000000000000000, 0.8660254037844387076, 1.000000000000000000, 0.8660254037844387076, 1.000000000000000000, 0.8660254037844387076, 1.000000000000000000, 0.8660254037844387076, 1.000000000000000000, 0.8660254037844387076, 1.000000000000000000, 0.9548847740583508159, 0.9401541683247176540) ) ) 
 REPRESENTATION_ITEM ( '' )  SURFACE ( )  );
#26702 = DIRECTION ( 'NONE',  ( 0.08715574274765142126, 0.000000000000000000, 0.9961946980917461003 ) ) ;
#26703 = CARTESIAN_POINT ( 'NONE',  ( 11.61527771782819940, 99.53518628210144925, -4.622313124798573369 ) ) ;
#26704 = CARTESIAN_POINT ( 'NONE',  ( 16.56230152254411436, 6.928203230275506996, -4.949999998771019705 ) ) ;
#26705 = CARTESIAN_POINT ( 'NONE',  ( -68.60788769728823411, 214.4690446883608104, 1.321298161741840893 ) ) ;
#26706 = CARTESIAN_POINT ( 'NONE',  ( 8.962234695871762469, 135.7601862821014720, -8.715434833791931624 ) ) ;
#26707 = CARTESIAN_POINT ( 'NONE',  ( 34.02033052368495447, -5.407089921784855591, 163.0045950240894967 ) ) ;
#26708 = CARTESIAN_POINT ( 'NONE',  ( 14.25334919248782661, 82.28518628210146346, 6.092822981423971385 ) ) ;
#26709 = CARTESIAN_POINT ( 'NONE',  ( 22.80587116629411781, -3.604726614523238837, -4.959374999385524951 ) ) ;
#26710 = CARTESIAN_POINT ( 'NONE',  ( 23.99999999999999645, 248.5000000000000000, -5.196152422706631135 ) ) ;
#26711 = DIRECTION ( 'NONE',  ( 0.000000000000000000, 0.9932091452657081376, 0.1163425707149433469 ) ) ;
#26712 = CARTESIAN_POINT ( 'NONE',  ( 10.49999999999999645, 237.0000000000000000, 5.000000000000000000 ) ) ;
#26713 = CARTESIAN_POINT ( 'NONE',  ( 9.465287035748067623, 118.7976862821014521, 2.064181346179272847 ) ) ;
#26714 = LINE ( 'NONE', #15733, #19512 ) ;
#26715 = CARTESIAN_POINT ( 'NONE',  ( -15.53471296425195369, 12.42268628210144144, 2.908627838312118019 ) ) ;
#26716 = CARTESIAN_POINT ( 'NONE',  ( -13.62178482187498396, 195.8843750006145399, 23.59362340125808188 ) ) ;
#26717 = CARTESIAN_POINT ( 'NONE',  ( 23.87821517812500005, 241.7968750006145342, 4.985214923628404016 ) ) ;
#26718 = EDGE_LOOP ( 'NONE', ( #9703, #6843 ) ) ;
#26719 = CARTESIAN_POINT ( 'NONE',  ( 28.01623001071507701, 5.407089921784856479, 166.0143398515642730 ) ) ;
#26720 = CARTESIAN_POINT ( 'NONE',  ( 15.24356964374999990, 3.323476615752268604, -3.778124999385444660 ) ) ;
#26721 = CARTESIAN_POINT ( 'NONE',  ( 15.00000000000000000, 0.000000000000000000, -5.343749998770963572 ) ) ;
#26722 = CARTESIAN_POINT ( 'NONE',  ( 1.255007937094097924E-14, 199.1000000012290627, -27.00000000000000355 ) ) ;
#26723 = CARTESIAN_POINT ( 'NONE',  ( 1.069080835302379631E-14, 199.3250000012290286, 27.00000000000000000 ) ) ;
#26724 = EDGE_CURVE ( 'NONE', #12557, #11818, #31269, .T. ) ;
#26725 = CARTESIAN_POINT ( 'NONE',  ( 13.50000000000001421, 198.8000000000000114, 23.38268590217984055 ) ) ;
#26726 = CARTESIAN_POINT ( 'NONE',  ( 3.796722387233182339, 22.01481371789855501, 8.710071997420207879 ) ) ;
#26727 = CARTESIAN_POINT ( 'NONE',  ( 13.62178482187499640, 197.0093750006145399, -23.59362340125807123 ) ) ;
#26729 = ORIENTED_EDGE ( 'NONE', *, *, #34869, .F. ) ;
#26728 = ORIENTED_EDGE ( 'NONE', *, *, #13511, .F. ) ;
#26730 = CARTESIAN_POINT ( 'NONE',  ( 15.24356964374999990, 247.0468750006145058, 0.000000000000000000 ) ) ;
#26731 = CARTESIAN_POINT ( 'NONE',  ( 0.1745138560722779009, 31.78981371789854649, 12.50000000000000355 ) ) ;
#26732 = CARTESIAN_POINT ( 'NONE',  ( 21.00000000000000000, -6.646953231504538984, -1.828124999385473792 ) ) ;
#26733 = CARTESIAN_POINT ( 'NONE',  ( 10.83675517735179206, 129.5398137178985678, -11.08355503943118769 ) ) ;
#26734 = CARTESIAN_POINT ( 'NONE',  ( 15.00000000000000000, 0.000000000000000000, -7.593749998770965348 ) ) ;
#26735 = ADVANCED_FACE ( 'NONE', ( #27552 ), #1768, .T. ) ;
#26736 = CARTESIAN_POINT ( 'NONE',  ( 25.28542051998549667, 0.000000000000000000, 167.8248601567890432 ) ) ;
#26737 = ORIENTED_EDGE ( 'NONE', *, *, #7630, .T. ) ;
#26738 = CARTESIAN_POINT ( 'NONE',  ( 19.68408634441912142, -5.407089921784861808, -2.746874999385529037 ) ) ;
#26739 = AXIS2_PLACEMENT_3D ( 'NONE', #7161, #32361, #4118 ) ;
#26740 = CARTESIAN_POINT ( 'NONE',  ( 5.778771075727756162E-15, 199.4656250006145797, 31.45816453501075927 ) ) ;
#26741 = CARTESIAN_POINT ( 'NONE',  ( 37.24626209435294300, -3.604726614523238837, 164.0586977410752638 ) ) ;
#26742 = APPLICATION_CONTEXT ( 'automotive_design' ) ;
#26743 = CARTESIAN_POINT ( 'NONE',  ( -67.01711230271185116, 218.4690446883607535, -2.393094931466363651 ) ) ;
#26744 = CARTESIAN_POINT ( 'NONE',  ( 23.87821517812499650, 248.2468750006145228, -4.985214923628404904 ) ) ;
#26745 = SURFACE_SIDE_STYLE ('',( #3249 ) ) ;
#26746 = EDGE_CURVE ( 'NONE', #18743, #20463, #19935, .T. ) ;
#26747 = CARTESIAN_POINT ( 'NONE',  ( 27.00000000000000355, 196.6250000000000284, -3.306546357697854128E-15 ) ) ;
#26748 = CARTESIAN_POINT ( 'NONE',  ( -50.78794563604517975, 206.7903428501025758, 3.378800118222471838 ) ) ;
#26749 =( BOUNDED_CURVE ( )  B_SPLINE_CURVE ( 2, ( #6538, #23231, #14883, #9007, #20395, #18111, #6350, #17920, #17730, #6156, #29465, #17362, #3500, #31247, #5276, #15069, #28903, #12219, #26064, #93, #11655, #20577, #29272, #34779, #29083, #3125, #3311, #14693, #33251, #16201, #840, #24355, #12785, #12408, #27187, #30031, #21144, #18491, #7291, #1403, #18865, #1027, #30223, #21702, #7475, #4622, #35708, #10312, #4064, #1212, #15636, #24164, #32682, #36267, #18681, #35897, #6920, #6726, #27000, #29839, #18299, #9940, #9759, #10129, #33434, #32873, #21520, #3875, #21334, #21884, #33066, #7111, #4249, #15449, #12979, #19054, #15823, #30412, #30605, #27373, #24536, #36085, #23981, #4435, #16016, #35526, #27564, #1593, #13161, #24717, #9570, #12600, #22444, #34179, #13911, #33991, #14092, #25088, #16754, #36829, #8035, #19243, #27750, #28302, #5362, #7850, #33813, #10494, #16387, #30784, #22073, #2148, #13533, #22261, #19974, #10682, #37198, #4989, #1780, #31517, #19423, #30973, #8224, #33625, #19609, #7665, #11057, #10871, #22814, #16572, #13729, #5178, #5542, #2340, #25462 ),
 .UNSPECIFIED., .F., .F. ) 
 B_SPLINE_CURVE_WITH_KNOTS ( ( 3, 2, 2, 2, 2, 2, 2, 2, 2, 2, 2, 2, 2, 2, 2, 2, 2, 2, 2, 2, 2, 2, 2, 2, 2, 2, 2, 2, 2, 2, 2, 2, 2, 2, 2, 2, 2, 2, 2, 2, 2, 2, 2, 2, 2, 2, 2, 2, 2, 2, 2, 2, 2, 2, 2, 2, 2, 2, 2, 2, 2, 2, 2, 2, 2, 2, 2, 3 ),
 ( 0.000000000000000000, 0.01388888888888888812, 0.02777777777777777624, 0.04166666666666666435, 0.05555555555555555247, 0.06944444444444444753, 0.08333333333333332871, 0.09722222222222222376, 0.1111111111111111049, 0.1250000000000000000, 0.1388888888888888951, 0.1527777777777777901, 0.1666666666666666574, 0.1805555555555555525, 0.1944444444444444475, 0.2083333333333333426, 0.2222222222222222099, 0.2361111111111111049, 0.2500000000000000000, 0.2638888888888888951, 0.2777777777777777901, 0.2916666666666666852, 0.3055555555555555802, 0.3194444444444444198, 0.3333333333333333148, 0.3472222222222222099, 0.3611111111111111049, 0.3750000000000000000, 0.3888888888888888951, 0.4027777777777777901, 0.4166666666666666852, 0.4305555555555555802, 0.4444444444444444198, 0.4583333333333333148, 0.4722222222222222099, 0.4861111111111111049, 0.5000000000000000000, 0.5138888888888888395, 0.5277777777777777901, 0.5416666666666666297, 0.5555555555555555802, 0.5694444444444444198, 0.5833333333333333703, 0.5972222222222222099, 0.6111111111111111605, 0.6250000000000000000, 0.6388888888888888395, 0.6527777777777777901, 0.6666666666666666297, 0.6805555555555555802, 0.6944444444444444198, 0.7083333333333333703, 0.7222222222222222099, 0.7361111111111111605, 0.7500000000000000000, 0.7638888888888888395, 0.7777777777777777901, 0.7916666666666666297, 0.8055555555555555802, 0.8194444444444444198, 0.8333333333333333703, 0.8472222222222222099, 0.8611111111111111605, 0.8750000000000000000, 0.8888888888888888395, 0.9027777777777777901, 0.9166666666666666297, 0.9258785558287928596 ),
 .UNSPECIFIED. ) 
 CURVE ( )  GEOMETRIC_REPRESENTATION_ITEM ( )  RATIONAL_B_SPLINE_CURVE ( ( 1.000000000000000000, 0.8660254037844387076, 1.000000000000000000, 0.8660254037844387076, 1.000000000000000000, 0.8660254037844387076, 1.000000000000000000, 0.8660254037844387076, 1.000000000000000000, 0.8660254037844387076, 1.000000000000000000, 0.8660254037844387076, 1.000000000000000000, 0.8660254037844387076, 1.000000000000000000, 0.8660254037844387076, 1.000000000000000000, 0.8660254037844387076, 1.000000000000000000, 0.8660254037844387076, 1.000000000000000000, 0.8660254037844387076, 1.000000000000000000, 0.8660254037844387076, 1.000000000000000000, 0.8660254037844387076, 1.000000000000000000, 0.8660254037844387076, 1.000000000000000000, 0.8660254037844387076, 1.000000000000000000, 0.8660254037844387076, 1.000000000000000000, 0.8660254037844387076, 1.000000000000000000, 0.8660254037844387076, 1.000000000000000000, 0.8660254037844387076, 1.000000000000000000, 0.8660254037844387076, 1.000000000000000000, 0.8660254037844387076, 1.000000000000000000, 0.8660254037844387076, 1.000000000000000000, 0.8660254037844387076, 1.000000000000000000, 0.8660254037844387076, 1.000000000000000000, 0.8660254037844387076, 1.000000000000000000, 0.8660254037844387076, 1.000000000000000000, 0.8660254037844387076, 1.000000000000000000, 0.8660254037844387076, 1.000000000000000000, 0.8660254037844387076, 1.000000000000000000, 0.8660254037844387076, 1.000000000000000000, 0.8660254037844387076, 1.000000000000000000, 0.8660254037844387076, 1.000000000000000000, 0.8660254037844387076, 1.000000000000000000, 0.8660254037844387076, 1.000000000000000000, 0.8660254037844387076, 1.000000000000000000, 0.8660254037844387076, 1.000000000000000000, 0.8660254037844387076, 1.000000000000000000, 0.8660254037844387076, 1.000000000000000000, 0.8660254037844387076, 1.000000000000000000, 0.8660254037844387076, 1.000000000000000000, 0.8660254037844387076, 1.000000000000000000, 0.8660254037844387076, 1.000000000000000000, 0.8660254037844387076, 1.000000000000000000, 0.8660254037844387076, 1.000000000000000000, 0.8660254037844387076, 1.000000000000000000, 0.8660254037844387076, 1.000000000000000000, 0.8660254037844387076, 1.000000000000000000, 0.8660254037844387076, 1.000000000000000000, 0.8660254037844387076, 1.000000000000000000, 0.8660254037844387076, 1.000000000000000000, 0.8660254037844387076, 1.000000000000000000, 0.8660254037844387076, 1.000000000000000000, 0.8660254037844387076, 1.000000000000000000, 0.8660254037844387076, 1.000000000000000000, 0.8660254037844387076, 1.000000000000000000, 0.8660254037844387076, 1.000000000000000000, 0.8660254037844387076, 1.000000000000000000, 0.8660254037844387076, 1.000000000000000000, 0.8660254037844387076, 1.000000000000000000, 0.8660254037844387076, 1.000000000000000000, 0.8660254037844387076, 1.000000000000000000, 0.8660254037844387076, 1.000000000000000000, 0.8660254037844387076, 1.000000000000000000, 0.8660254037844387076, 1.000000000000000000, 0.8660254037844387076, 1.000000000000000000, 0.8660254037844387076, 1.000000000000000000, 0.9111405425767590271, 0.9401542252352144136 ) ) 
 REPRESENTATION_ITEM ( '' )  );
#26750 = CARTESIAN_POINT ( 'NONE',  ( -37.53497103062156981, 204.4285982733020148, -3.350049139982115509 ) ) ;
#26751 = CARTESIAN_POINT ( 'NONE',  ( 24.98803303140584120, 3.604726614523236616, 167.2203538558741798 ) ) ;
#26752 = VERTEX_POINT ( 'NONE', #19229 ) ;
#26753 = CARTESIAN_POINT ( 'NONE',  ( 15.00000000000000000, 0.000000000000000000, -6.299999999999999822 ) ) ;
#26754 = CARTESIAN_POINT ( 'NONE',  ( -2.908627838312119351, 134.3226862821014436, -15.53471296425195369 ) ) ;
#26755 = CARTESIAN_POINT ( 'NONE',  ( -65.83705436395491972, 203.8621396198270475, -6.307003348497942419 ) ) ;
#26756 = VECTOR ( 'NONE', #23844, 1000.000000000000000 ) ;
#26757 = CARTESIAN_POINT ( 'NONE',  ( 5.233372021372432847, 129.1476862821014322, 8.152565276336710909 ) ) ;
#26758 = CARTESIAN_POINT ( 'NONE',  ( 15.00000000000000000, 246.4187500012290286, -3.464101615137752610 ) ) ;
#26759 = CARTESIAN_POINT ( 'NONE',  ( -4.622313124798576922, 23.63518628210144357, -11.61527771782819762 ) ) ;
#26760 = CARTESIAN_POINT ( 'NONE',  ( 10.56230152254411259, -3.464101615137761048, -6.262500000000039257 ) ) ;
#26761 = VERTEX_POINT ( 'NONE', #36631 ) ;
#26762 = DIRECTION ( 'NONE',  ( -4.130293990420971855E-17, 1.000000000000000000, 0.000000000000000000 ) ) ;
#26763 = CARTESIAN_POINT ( 'NONE',  ( 10.83675517735155225, 119.6601862821014635, 11.08355503943142573 ) ) ;
#26764 = CARTESIAN_POINT ( 'NONE',  ( 38.04237167757722915, 114.1383727779940074, 0.5000000000000000000 ) ) ;
#26765 = CARTESIAN_POINT ( 'NONE',  ( 7.954856959092311719, 139.0273137178985507, -5.529263428287300108 ) ) ;
#26766 = CARTESIAN_POINT ( 'NONE',  ( -1.926257025242585782E-15, 198.7906250006145399, -31.45816453501075927 ) ) ;
#26767 = CARTESIAN_POINT ( 'NONE',  ( -14.50000000000000000, 215.7563705986615901, -5.555555555555558023 ) ) ;
#26768 = CARTESIAN_POINT ( 'NONE',  ( 20.03537803801927808, -5.091549871530747673, -10.00000000000000000 ) ) ;
#26769 = CARTESIAN_POINT ( 'NONE',  ( 25.18249928241153413, 0.000000000000000000, 169.4431132759913794 ) ) ;
#26770 = FACE_OUTER_BOUND ( 'NONE', #8608, .T. ) ;
#26771 =( BOUNDED_CURVE ( )  B_SPLINE_CURVE ( 2, ( #15177, #20876, #32415, #6459, #18030, #32979, #29573 ),
 .UNSPECIFIED., .F., .F. ) 
 B_SPLINE_CURVE_WITH_KNOTS ( ( 3, 2, 2, 3 ),
 ( 0.4130434782608686239, 0.4202898550724629145, 0.4275362318840573161, 0.4347826086956516067 ),
 .UNSPECIFIED. ) 
 CURVE ( )  GEOMETRIC_REPRESENTATION_ITEM ( )  RATIONAL_B_SPLINE_CURVE ( ( 1.000000000000017542, 0.8660254037844213881, 1.000000000000000000, 0.8660254037844387076, 1.000000000000000000, 0.8660254037844489217, 0.9999999999999897859 ) ) 
 REPRESENTATION_ITEM ( '' )  );
#26772 = CARTESIAN_POINT ( 'NONE',  ( -8.152565276336593669, 71.75231371789854506, -5.233372021372610483 ) ) ;
#26773 = CARTESIAN_POINT ( 'NONE',  ( 15.24356964375000167, 240.4468750006145399, 3.323476615752272600 ) ) ;
#26774 = ORIENTED_EDGE ( 'NONE', *, *, #37465, .T. ) ;
#26775 = CARTESIAN_POINT ( 'NONE',  ( 18.00000000000000000, 242.7812500012290400, -5.196152422706630247 ) ) ;
#26776 = CARTESIAN_POINT ( 'NONE',  ( 4.944772684328420986, 104.8148137178985593, 11.48171059495408208 ) ) ;
#26777 = EDGE_CURVE ( 'NONE', #35535, #10416, #32531, .T. ) ;
#26778 = CARTESIAN_POINT ( 'NONE',  ( 16.56230152254411436, 7.209453229046482114, -4.359374999385510208 ) ) ;
#26779 = CARTESIAN_POINT ( 'NONE',  ( 15.00000000000000178, 246.8874999999999886, 3.464101615137757051 ) ) ;
#26780 = CARTESIAN_POINT ( 'NONE',  ( 18.12178482187499640, 4.985214923628404904, -5.728124999385491911 ) ) ;
#26781 = CARTESIAN_POINT ( 'NONE',  ( -8.962234695871565293, 53.63981371789855501, -8.715434833792128799 ) ) ;
#26782 = CARTESIAN_POINT ( 'NONE',  ( 13.62178482187499640, 197.4593750006145285, -23.59362340125807123 ) ) ;
#26783 = ORIENTED_EDGE ( 'NONE', *, *, #22577, .T. ) ;
#26784 = ORIENTED_EDGE ( 'NONE', *, *, #14814, .T. ) ;
#26785 = CARTESIAN_POINT ( 'NONE',  ( 15.24356964374999990, 0.000000000000000000, -5.540624999385457272 ) ) ;
#26786 = CARTESIAN_POINT ( 'NONE',  ( 16.56230152254411792, 6.928203230275514990, -1.012500000000046585 ) ) ;
#26787 = CARTESIAN_POINT ( 'NONE',  ( 15.24356964375000167, 245.2843750006144887, 3.323476615752272600 ) ) ;
#26788 = CARTESIAN_POINT ( 'NONE',  ( 8.962234695871762469, 43.76018628210144357, -8.715434833791931624 ) ) ;
#26789 = VECTOR ( 'NONE', #24186, 1000.000000000000000 ) ;
#26790 = CARTESIAN_POINT ( 'NONE',  ( -40.89211230271182274, 203.5309553116391896, 1.857196546604092724 ) ) ;
#26791 = CARTESIAN_POINT ( 'NONE',  ( 10.31873187879411091, 0.000000000000000000, -0.1406249993855246405 ) ) ;
#26792 = CARTESIAN_POINT ( 'NONE',  ( -63.45461230271182274, 208.1428034533959135, -6.469044688360754414 ) ) ;
#26793 =( NAMED_UNIT ( * ) SI_UNIT ( $, .STERADIAN. ) SOLID_ANGLE_UNIT ( ) );
#26794 = CARTESIAN_POINT ( 'NONE',  ( -47.00000000000000711, 237.0000000000000000, -2.499999999999998224 ) ) ;
#26795 = CARTESIAN_POINT ( 'NONE',  ( 10.69584247140429589, 76.35231371789855359, 6.932735513424201024 ) ) ;
#26796 = CARTESIAN_POINT ( 'NONE',  ( -64.25372103062157692, 214.5309553116392749, -1.090244570138262148 ) ) ;
#26797 = CARTESIAN_POINT ( 'NONE',  ( -36.14955436395489841, 216.3070033484980002, -6.137860380172975638 ) ) ;
#26798 = CARTESIAN_POINT ( 'NONE',  ( 23.87821517812499650, 4.985214923628404904, -6.253124999385489602 ) ) ;
#26799 = CARTESIAN_POINT ( 'NONE',  ( 10.56230152254438615, 3.464101615137917811, -0.4875000000000282441 ) ) ;
#26800 = CARTESIAN_POINT ( 'NONE',  ( 2.908627838312458636, 64.27731371789853654, -15.53471296425188442 ) ) ;
#26801 = CARTESIAN_POINT ( 'NONE',  ( -64.04836230271183695, 202.5810206699313767, -4.149950860017804111 ) ) ;
#26802 = AXIS2_PLACEMENT_3D ( 'NONE', #36671, #30999, #1804 ) ;
#26803 = CARTESIAN_POINT ( 'NONE',  ( 26.99999999999999645, 240.7374999999999545, 3.464101615137751278 ) ) ;
#26804 = CARTESIAN_POINT ( 'NONE',  ( -6.932735513423968321, 87.74768628210145494, -10.69584247140445221 ) ) ;
#26805 = CARTESIAN_POINT ( 'NONE',  ( 6.092822981423978490, 33.98518628210143788, -14.25334919248782306 ) ) ;
#26807 = EDGE_CURVE ( 'NONE', #36105, #28452, #27673, .T. ) ;
#26806 = DIRECTION ( 'NONE',  ( -0.000000000000000000, 1.000000000000000000, -0.000000000000000000 ) ) ;
#26808 = CARTESIAN_POINT ( 'NONE',  ( 27.55375985076035761, -5.407089921784865361, 160.7282817348149706 ) ) ;
#26809 = CARTESIAN_POINT ( 'NONE',  ( 11.08355503943142750, 43.76018628210144357, -10.83675517735155225 ) ) ;
#26810 = CARTESIAN_POINT ( 'NONE',  ( 22.60769515458674306, 247.0388461906614168, 5.999999999999992895 ) ) ;
#26811 = DIRECTION ( 'NONE',  ( -1.000000000000000000, 0.000000000000000000, 1.636531581110199847E-16 ) ) ;
#26812 = DIRECTION ( 'NONE',  ( -0.000000000000000000, -1.000000000000000000, -0.000000000000000000 ) ) ;
#26813 = CARTESIAN_POINT ( 'NONE',  ( -34.17038769728823411, 208.1428034533959703, 6.469044688360770401 ) ) ;
#26814 = CARTESIAN_POINT ( 'NONE',  ( 23.99999999999999645, 241.3562500012290286, -5.196152422706631135 ) ) ;
#26815 = CARTESIAN_POINT ( 'NONE',  ( -4.622313124798576922, 14.43518628210144250, -11.61527771782819762 ) ) ;
#26816 = DIRECTION ( 'NONE',  ( 0.000000000000000000, 0.000000000000000000, 1.000000000000000000 ) ) ;
#26817 = CARTESIAN_POINT ( 'NONE',  ( 8.843639120294245259, 122.0648137178985877, 3.474262827703527901 ) ) ;
#26818 = CARTESIAN_POINT ( 'NONE',  ( 23.87821517812500005, 247.3093750006145228, 4.985214923628404016 ) ) ;
#26819 = ORIENTED_EDGE ( 'NONE', *, *, #29509, .T. ) ;
#26820 = CARTESIAN_POINT ( 'NONE',  ( 23.99999999999999645, 5.196152422706631135, -7.349999999999995204 ) ) ;
#26821 = CARTESIAN_POINT ( 'NONE',  ( 2.999999999999997335, 244.5000000000000000, 1.000000000000000000 ) ) ;
#26822 = EDGE_CURVE ( 'NONE', #10334, #2700, #14923, .T. ) ;
#26823 = DIRECTION ( 'NONE',  ( -0.000000000000000000, 1.000000000000000000, -0.000000000000000000 ) ) ;
#26824 = CARTESIAN_POINT ( 'NONE',  ( 19.68408634441910721, -5.407089921784855591, -7.640624999385531524 ) ) ;
#26825 = CARTESIAN_POINT ( 'NONE',  ( 28.05545009495152087, 5.407089921784856479, 166.4626274657055660 ) ) ;
#26826 = FACE_OUTER_BOUND ( 'NONE', #14616, .T. ) ;
#26827 = CARTESIAN_POINT ( 'NONE',  ( 13.49999999999999645, 199.8499999999999943, -23.38268590217984766 ) ) ;
#26828 = CARTESIAN_POINT ( 'NONE',  ( -4.944772684328673229, 47.78518628210144925, 11.48171059495397728 ) ) ;
#26829 = VERTEX_POINT ( 'NONE', #25265 ) ;
#26830 = ADVANCED_FACE ( 'NONE', ( #36817 ), #10859, .F. ) ;
#26831 = ORIENTED_EDGE ( 'NONE', *, *, #9631, .T. ) ;
#26832 = LINE ( 'NONE', #36107, #24294 ) ;
#26833 = CARTESIAN_POINT ( 'NONE',  ( 10.56230152254410903, 0.000000000000000000, -2.250000000000057732 ) ) ;
#26834 = CARTESIAN_POINT ( 'NONE',  ( 24.00000000000000000, 246.5499999999999829, 5.196152422706629359 ) ) ;
#26835 = CARTESIAN_POINT ( 'NONE',  ( 27.00000000000000355, 195.2750000000000057, -3.306546357697854128E-15 ) ) ;
#26836 = CARTESIAN_POINT ( 'NONE',  ( 23.87821517812499650, 4.985214923628404904, -5.690624999385468286 ) ) ;
#26837 = CARTESIAN_POINT ( 'NONE',  ( -8.715434833791929847, 87.46018628210144641, -8.962234695871762469 ) ) ;
#26838 = CARTESIAN_POINT ( 'NONE',  ( 15.53471296425188797, 20.57731371789854435, 2.908627838312457747 ) ) ;
#26839 = CARTESIAN_POINT ( 'NONE',  ( 16.56230152254411081, -6.928203230275506996, -3.824999998771014376 ) ) ;
#26840 = CARTESIAN_POINT ( 'NONE',  ( 33.81648353596441581, 5.196152422706631135, 162.0719374165519469 ) ) ;
#26841 = CARTESIAN_POINT ( 'NONE',  ( -67.41294563604516554, 213.2096571498974527, -3.378800118222469617 ) ) ;
#26842 = CARTESIAN_POINT ( 'NONE',  ( 18.00000000000000000, 245.4250000000000114, -5.196152422706630247 ) ) ;
#26843 = CARTESIAN_POINT ( 'NONE',  ( 36.85732959234155004, 7.646167579472024665E-16, 159.6131789008408646 ) ) ;
#26844 = CARTESIAN_POINT ( 'NONE',  ( 10.69584247140429589, 131.5523137178985564, 6.932735513424201024 ) ) ;
#26845 = CARTESIAN_POINT ( 'NONE',  ( -56.33705436395489841, 205.3262412349647263, -4.842901733360204020 ) ) ;
#26846 = CARTESIAN_POINT ( 'NONE',  ( -69.79538769728823411, 212.3930949314662371, -8.469044688360781947 ) ) ;
#26847 = CIRCLE ( 'NONE', #25033, 9.999999999999994671 ) ;
#26848 = CONTEXT_DEPENDENT_SHAPE_REPRESENTATION ( #30133, #14706 ) ;
#26849 = CARTESIAN_POINT ( 'NONE',  ( 15.24356964375000167, -3.323476615752272600, -0.6656249993855035685 ) ) ;
#26850 = CARTESIAN_POINT ( 'NONE',  ( -13.62178482187498396, 198.9781250006145399, 23.59362340125808188 ) ) ;
#26851 = CARTESIAN_POINT ( 'NONE',  ( 15.50000000000000533, 121.4898137178985564, -0.1745138560722452326 ) ) ;
#26852 = CARTESIAN_POINT ( 'NONE',  ( -56.32961230271183695, 211.8571965466040297, 6.469044688360755302 ) ) ;
#26853 = EDGE_LOOP ( 'NONE', ( #11618, #30905, #12800, #3046 ) ) ;
#26854 = CARTESIAN_POINT ( 'NONE',  ( -2.311890736173176641, 33.12268628210144072, -12.53471296425194836 ) ) ;
#26855 = CARTESIAN_POINT ( 'NONE',  ( 15.00000000000000178, 244.6937500012290627, 3.464101615137757051 ) ) ;
#26856 = CARTESIAN_POINT ( 'NONE',  ( 20.99999999999998579, 247.2437500012290457, -5.999999999999997335 ) ) ;
#26857 = CARTESIAN_POINT ( 'NONE',  ( 34.42070221693199272, 5.407089921784862696, 167.5808644184484706 ) ) ;
#26858 = CARTESIAN_POINT ( 'NONE',  ( -13.04141134922759804, 96.37268628210144072, -8.927990412390657937 ) ) ;
#26859 = CARTESIAN_POINT ( 'NONE',  ( -66.23288769728823411, 203.5309553116391896, -1.857196546604028997 ) ) ;
#26860 = CARTESIAN_POINT ( 'NONE',  ( 16.56230152254411081, -7.209453229046475009, -2.728124999385529215 ) ) ;
#26861 = CARTESIAN_POINT ( 'NONE',  ( -9.534712964251941258, 49.22268628210144215, 1.715153634034234154 ) ) ;
#26862 = EDGE_CURVE ( 'NONE', #25843, #37126, #14604, .T. ) ;
#26863 = LINE ( 'NONE', #9246, #10428 ) ;
#26864 = CARTESIAN_POINT ( 'NONE',  ( -35.35788769728823411, 218.4690446883607535, 2.393094931466250408 ) ) ;
#26865 = CARTESIAN_POINT ( 'NONE',  ( -10.69584247140444866, 76.24768628210144072, 6.932735513423972762 ) ) ;
#26866 = DIRECTION ( 'NONE',  ( -0.000000000000000000, -1.000000000000000000, -0.000000000000000000 ) ) ;
#26867 = CARTESIAN_POINT ( 'NONE',  ( 10.56230152254410903, 0.000000000000000000, -7.987499998771019349 ) ) ;
#26868 = VERTEX_POINT ( 'NONE', #17117 ) ;
#26869 = CARTESIAN_POINT ( 'NONE',  ( 24.00000000000000000, 244.8062500012290457, 5.196152422706629359 ) ) ;
#26870 = CARTESIAN_POINT ( 'NONE',  ( 18.00000000000000000, 5.196152422706630247, -0.5249999999999976907 ) ) ;
#26871 = CYLINDRICAL_SURFACE ( 'NONE', #21207, 5.999999999999999112 ) ;
#26872 = CARTESIAN_POINT ( 'NONE',  ( 37.24953043470598146, 7.646167579472024665E-16, 164.0960550422537096 ) ) ;
#26873 = CARTESIAN_POINT ( 'NONE',  ( 31.01746318205820785, 6.928203230275514990, 164.5001281119201053 ) ) ;
#26874 = CYLINDRICAL_SURFACE ( 'NONE', #25313, 5.999999999999998224 ) ;
#26875 = CARTESIAN_POINT ( 'NONE',  ( 15.00000000000000000, 249.5499999999999829, 0.000000000000000000 ) ) ;
#26876 = CARTESIAN_POINT ( 'NONE',  ( -27.24356964375000345, 195.7156250006145513, -15.72908226750537786 ) ) ;
#26877 = ADVANCED_FACE ( 'NONE', ( #34537 ), #26005, .T. ) ;
#26878 = CARTESIAN_POINT ( 'NONE',  ( 10.69584247140429589, 103.9523137178985621, 6.932735513424201024 ) ) ;
#26879 = CARTESIAN_POINT ( 'NONE',  ( -12.46528703574805874, 95.79768628210145209, -2.660918448318280838 ) ) ;
#26880 = EDGE_LOOP ( 'NONE', ( #27718, #2819, #7683 ) ) ;
#26881 = ORIENTED_EDGE ( 'NONE', *, *, #7534, .F. ) ;
#26882 = CARTESIAN_POINT ( 'NONE',  ( -27.24356964375000345, 196.2031250006145342, 0.000000000000000000 ) ) ;
#26883 = DIRECTION ( 'NONE',  ( -0.000000000000000000, 1.000000000000000000, -0.000000000000000000 ) ) ;
#26884 = CARTESIAN_POINT ( 'NONE',  ( 0.1745138560722461762, 68.58981371789855075, 15.50000000000000533 ) ) ;
#26885 = CARTESIAN_POINT ( 'NONE',  ( 26.75643035624999655, -3.323476615752267715, -3.665624999385485694 ) ) ;
#26886 = CARTESIAN_POINT ( 'NONE',  ( 21.00000000000000000, 248.3968750006145285, -6.646953231504538984 ) ) ;
#26887 = CARTESIAN_POINT ( 'NONE',  ( 8.152565276336714462, 108.4476862821014294, -5.233372021372432847 ) ) ;
#26888 = AXIS2_PLACEMENT_3D ( 'NONE', #28864, #26025, #5372 ) ;
#26889 = CARTESIAN_POINT ( 'NONE',  ( 6.932735513423970097, 110.7476862821014549, 10.69584247140445044 ) ) ;
#26890 = DIRECTION ( 'NONE',  ( 0.000000000000000000, 0.000000000000000000, 1.000000000000000000 ) ) ;
#26891 = CARTESIAN_POINT ( 'NONE',  ( 6.594114490232462877, 55.93981371789855217, -6.840914352311949109 ) ) ;
#26892 = PRESENTATION_LAYER_ASSIGNMENT (  '', '', ( #5694 ) ) ;
#26893 = CARTESIAN_POINT ( 'NONE',  ( 13.44051670066911086, 5.407089921784856479, -4.265624999385542182 ) ) ;
#26894 = CARTESIAN_POINT ( 'NONE',  ( -3.474262827703527901, 105.9648137178985650, 8.843639120294245259 ) ) ;
#26895 = CARTESIAN_POINT ( 'NONE',  ( 15.24356964374999990, 240.7468750006144944, 0.000000000000000000 ) ) ;
#26896 = CARTESIAN_POINT ( 'NONE',  ( 4.622313124798831829, 36.96481371789854364, -11.61527771782809282 ) ) ;
#26897 = CARTESIAN_POINT ( 'NONE',  ( 25.22005371303209387, -3.464101615137879620, 167.0777141344445909 ) ) ;
#26898 = CARTESIAN_POINT ( 'NONE',  ( 11.48171059495397728, 109.8851862821014436, 4.944772684328674117 ) ) ;
#26899 = CARTESIAN_POINT ( 'NONE',  ( 16.56230152254411081, 6.928203230275506996, -6.299999998771006915 ) ) ;
#26900 = CARTESIAN_POINT ( 'NONE',  ( -34.56622103062155560, 211.6261429550005744, 6.530955311639227823 ) ) ;
#26901 = CARTESIAN_POINT ( 'NONE',  ( 23.99999999999999645, 5.196152422706631135, -7.293749998770943321 ) ) ;
#26902 = CARTESIAN_POINT ( 'NONE',  ( 34.07262396933355575, 5.407089921784857367, 163.6023118429445162 ) ) ;
#26903 = CARTESIAN_POINT ( 'NONE',  ( -13.23911966647218463, 85.44768628210142936, 8.632099005475506459 ) ) ;
#26904 = CARTESIAN_POINT ( 'NONE',  ( 10.31873187879410558, -3.604726614523244610, -4.209374999385490312 ) ) ;
#26905 = CARTESIAN_POINT ( 'NONE',  ( 13.56230152254410726, 5.196152422706630247, -3.112499998771029119 ) ) ;
#26906 = CARTESIAN_POINT ( 'NONE',  ( -54.50000000000000711, 237.0000000000000000, 2.500000000000000000 ) ) ;
#26907 = CARTESIAN_POINT ( 'NONE',  ( 15.00000000000053468, -3.464101615138063472, -5.756249998770931242 ) ) ;
#26908 = CARTESIAN_POINT ( 'NONE',  ( 9.500000000000005329, 109.3101862821014549, 0.1745138560725188748 ) ) ;
#26909 = FACE_OUTER_BOUND ( 'NONE', #31085, .T. ) ;
#26910 = CARTESIAN_POINT ( 'NONE',  ( -0.1745138560725500443, 130.0101862821014436, 12.50000000000000355 ) ) ;
#26911 = CARTESIAN_POINT ( 'NONE',  ( -27.24356964374999990, 195.7718750006145569, -15.72908226750537786 ) ) ;
#26912 = CARTESIAN_POINT ( 'NONE',  ( 23.87821517812499650, 243.2968750006145058, -4.985214923628404904 ) ) ;
#26913 = ORIENTED_EDGE ( 'NONE', *, *, #31608, .F. ) ;
#26914 = CARTESIAN_POINT ( 'NONE',  ( 37.40804494182826545, -3.604726614523235284, 165.9078841494080336 ) ) ;
#26915 = CARTESIAN_POINT ( 'NONE',  ( 23.87821517812499650, 4.985214923628404904, -2.540624999385482141 ) ) ;
#26916 = CARTESIAN_POINT ( 'NONE',  ( 24.00000000000000000, -5.196152422706629359, -4.743749998770946164 ) ) ;
#26917 = CARTESIAN_POINT ( 'NONE',  ( 15.02283181144952628, 7.347880794884122694E-16, 50.52293445648592751 ) ) ;
#26918 = CARTESIAN_POINT ( 'NONE',  ( 1.069080835302379631E-14, 199.6625000000000227, 27.00000000000000000 ) ) ;
#26919 = CARTESIAN_POINT ( 'NONE',  ( 6.594114490232462877, 19.13981371789855146, -6.840914352311949109 ) ) ;
#26920 = CARTESIAN_POINT ( 'NONE',  ( -27.24356964375000345, 196.6718750006145342, -15.72908226750537786 ) ) ;
#26922 = VERTEX_POINT ( 'NONE', #8952 ) ;
#26921 = ORIENTED_EDGE ( 'NONE', *, *, #11433, .T. ) ;
#26923 = CARTESIAN_POINT ( 'NONE',  ( 26.75643035624999655, 246.8218750006145115, -7.049594010296217766E-16 ) ) ;
#26924 = CARTESIAN_POINT ( 'NONE',  ( 12.53471296425189330, 29.77731371789854720, 2.311890736173451533 ) ) ;
#26925 = CARTESIAN_POINT ( 'NONE',  ( 21.00000000000000000, -6.646953231504538984, -2.278124999385469529 ) ) ;
#26926 = CARTESIAN_POINT ( 'NONE',  ( 6.092822981423662299, 132.4148137178985678, 14.25334919248795096 ) ) ;
#26927 = CARTESIAN_POINT ( 'NONE',  ( 15.00000000000000000, 0.000000000000000000, -6.243749998770947940 ) ) ;
#26928 = CYLINDRICAL_SURFACE ( 'NONE', #10465, 3.999999999999996447 ) ;
#26929 = ORIENTED_EDGE ( 'NONE', *, *, #4742, .T. ) ;
#26930 = CARTESIAN_POINT ( 'NONE',  ( 19.68408634441911431, 5.407089921784862696, -5.746874999385531702 ) ) ;
#26931 = ORIENTED_EDGE ( 'NONE', *, *, #4147, .T. ) ;
#26932 = CARTESIAN_POINT ( 'NONE',  ( -27.24356964374999635, 196.2406250006145285, 15.72908226750539384 ) ) ;
#26933 = CARTESIAN_POINT ( 'NONE',  ( -8.715434833791929847, 133.4601862821014606, -8.962234695871762469 ) ) ;
#26934 = CARTESIAN_POINT ( 'NONE',  ( 24.79029844004710625, 0.000000000000000000, 164.9602371345785343 ) ) ;
#26935 = CARTESIAN_POINT ( 'NONE',  ( -56.13169563604517265, 210.1155267958018271, 8.500000000000003553 ) ) ;
#26936 = CARTESIAN_POINT ( 'NONE',  ( 18.12178482187499640, 245.6218750006145228, -4.985214923628404904 ) ) ;
#26937 = CARTESIAN_POINT ( 'NONE',  ( 7.234628195640269155, 196.5325961894323257, 27.00000000000003197 ) ) ;
#26938 = CARTESIAN_POINT ( 'NONE',  ( -46.03794563604517975, 206.7903428501025758, 3.378800118222471838 ) ) ;
#26940 = ADVANCED_FACE ( 'NONE', ( #25448 ), #34353, .T. ) ;
#26939 = CARTESIAN_POINT ( 'NONE',  ( 2.999999999999997335, 244.5000000000000000, 5.000000000000000888 ) ) ;
#26941 = CARTESIAN_POINT ( 'NONE',  ( 24.91286120328598841, 0.000000000000000000, 166.3611359287700395 ) ) ;
#26942 = EDGE_LOOP ( 'NONE', ( #7401, #1000, #14991 ) ) ;
#26943 = CIRCLE ( 'NONE', #5156, 4.899999999999999467 ) ;
#26944 = CARTESIAN_POINT ( 'NONE',  ( -15.46528703574804986, 132.5976862821014493, -3.257655550457287497 ) ) ;
#26945 = CARTESIAN_POINT ( 'NONE',  ( -54.15997103062156981, 217.3034525342668815, 4.350049139982096413 ) ) ;
#26946 = CARTESIAN_POINT ( 'NONE',  ( -9.465287035748065847, 123.3976862821014606, -2.064181346179273735 ) ) ;
#26947 = CARTESIAN_POINT ( 'NONE',  ( 22.56230152254410015, 7.347880794884117764E-16, -7.312499998771010645 ) ) ;
#26948 = CARTESIAN_POINT ( 'NONE',  ( -12.50000000000000355, 21.91018628210143859, -0.1745138560725492671 ) ) ;
#26949 = CARTESIAN_POINT ( 'NONE',  ( 22.56230152254411792, 7.347880794884125653E-16, -6.975000000000036948 ) ) ;
#26950 = ORIENTED_EDGE ( 'NONE', *, *, #7484, .F. ) ;
#26951 = CARTESIAN_POINT ( 'NONE',  ( 13.50000000000001421, 197.5625000012290400, 23.38268590217984055 ) ) ;
#26952 = CARTESIAN_POINT ( 'NONE',  ( 8.632099005475504683, 129.1476862821014322, 13.23911966647218996 ) ) ;
#26953 = CARTESIAN_POINT ( 'NONE',  ( 22.56230152254320842, -3.464101615138272638, -5.999999998771010645 ) ) ;
#26954 = CARTESIAN_POINT ( 'NONE',  ( 2.064181346179061460, 141.9023137178985507, 9.465287035748106703 ) ) ;
#26955 = CARTESIAN_POINT ( 'NONE',  ( -13.62178482187500528, 199.2781250006145228, -23.59362340125807123 ) ) ;
#26956 = CARTESIAN_POINT ( 'NONE',  ( 20.99999999999999645, 6.928203230275506996, -1.462500000000010125 ) ) ;
#26957 = CARTESIAN_POINT ( 'NONE',  ( 16.56230152254411436, 6.928203230275514990, -5.512500000000034817 ) ) ;
#26958 = CARTESIAN_POINT ( 'NONE',  ( 0.000000000000000000, 0.000000000000000000, -2.500000000000000000 ) ) ;
#26959 = EDGE_CURVE ( 'NONE', #25991, #22829, #21597, .T. ) ;
#26960 = DIRECTION ( 'NONE',  ( -0.000000000000000000, -1.000000000000000000, -0.000000000000000000 ) ) ;
#26961 = CARTESIAN_POINT ( 'NONE',  ( 8.152565276336593669, 76.35231371789853938, 5.233372021372610483 ) ) ;
#26962 = CARTESIAN_POINT ( 'NONE',  ( 22.56230152254410370, 7.347880794884117764E-16, -4.162499998770996967 ) ) ;
#26963 = VERTEX_POINT ( 'NONE', #2693 ) ;
#26964 = AXIS2_PLACEMENT_3D ( 'NONE', #7997, #11020, #34510 ) ;
#26965 = CARTESIAN_POINT ( 'NONE',  ( 23.99999999999999645, 244.5062500012290627, -5.196152422706631135 ) ) ;
#26966 = CARTESIAN_POINT ( 'NONE',  ( -2.660918448318005058, 82.10231371789855359, -12.46528703574811558 ) ) ;
#26967 = CARTESIAN_POINT ( 'NONE',  ( 19.68408634441911076, 5.407089921784862696, -3.946874999385563410 ) ) ;
#26968 = CARTESIAN_POINT ( 'NONE',  ( -11.32995696862643875, 142.9999999999997442, 7.763613995393375156 ) ) ;
#26969 = CARTESIAN_POINT ( 'NONE',  ( 23.87821517812500005, -4.985214923628404016, -3.703124999385493332 ) ) ;
#26970 = CARTESIAN_POINT ( 'NONE',  ( 8.962234695871567070, 49.03981371789854649, 8.715434833792127023 ) ) ;
#26971 = EDGE_CURVE ( 'NONE', #8056, #4638, #16930, .T. ) ;
#26972 = CIRCLE ( 'NONE', #20930, 24.80000000000000426 ) ;
#26973 = EDGE_LOOP ( 'NONE', ( #35351, #22823 ) ) ;
#26974 = APPLICATION_CONTEXT ( 'automotive_design' ) ;
#26975 = ORIENTED_EDGE ( 'NONE', *, *, #36583, .F. ) ;
#26976 = CARTESIAN_POINT ( 'NONE',  ( 25.02395329185000250, -3.464101615137956003, 164.8362760637381541 ) ) ;
#26977 = CARTESIAN_POINT ( 'NONE',  ( 18.12178482187499640, 245.1718750006145058, -4.985214923628404904 ) ) ;
#26978 = CARTESIAN_POINT ( 'NONE',  ( -4.944772684328673229, 29.38518628210144712, 11.48171059495397728 ) ) ;
#26979 =( BOUNDED_CURVE ( )  B_SPLINE_CURVE ( 2, ( #6375, #17577, #20987, #11870, #9036, #23818, #31966, #31775, #677 ),
 .UNSPECIFIED., .F., .F. ) 
 B_SPLINE_CURVE_WITH_KNOTS ( ( 3, 2, 2, 2, 3 ),
 ( 0.05434782608695652023, 0.05797101449275362389, 0.06521739130434782428, 0.07246376811594203160, 0.07608695652173913526 ),
 .UNSPECIFIED. ) 
 CURVE ( )  GEOMETRIC_REPRESENTATION_ITEM ( )  RATIONAL_B_SPLINE_CURVE ( ( 0.9330127018922191873, 0.9330127018922191873, 1.000000000000000000, 0.8660254037844387076, 1.000000000000000000, 0.8660254037844387076, 1.000000000000000000, 0.9330127018922191873, 0.9330127018922192983 ) ) 
 REPRESENTATION_ITEM ( '' )  );
#26980 = CARTESIAN_POINT ( 'NONE',  ( -39.30877896937849414, 211.6261429550004891, -6.530955311639245586 ) ) ;
#26981 = CARTESIAN_POINT ( 'NONE',  ( 22.80587116629410716, 7.646167579472015790E-16, -0.8156249993855335667 ) ) ;
#26982 = CARTESIAN_POINT ( 'NONE',  ( -66.42336230271182274, 215.6869285224997270, 3.149950860017831200 ) ) ;
#26983 = CARTESIAN_POINT ( 'NONE',  ( 24.66443585301559693, 3.464101615137752166, 160.7269729341097104 ) ) ;
#26984 = CARTESIAN_POINT ( 'NONE',  ( -7.228626920338836470, 90.72731371789853938, -10.49813415416005213 ) ) ;
#26985 = CARTESIAN_POINT ( 'NONE',  ( -46.24330436395489841, 210.1155267958017703, -4.499999999999996447 ) ) ;
#26986 = CARTESIAN_POINT ( 'NONE',  ( -68.80580436395490551, 216.5000000000000000, 0.1155267958017343610 ) ) ;
#26987 = CARTESIAN_POINT ( 'NONE',  ( 26.75643035624999655, -3.323476615752267271, -7.265624999385483562 ) ) ;
#26988 = CARTESIAN_POINT ( 'NONE',  ( -0.1745138560722442889, 54.78981371789855359, -15.50000000000000533 ) ) ;
#26989 = CARTESIAN_POINT ( 'NONE',  ( -40.69419563604516554, 201.5000000000000000, 0.1155267958018195706 ) ) ;
#26990 = EDGE_CURVE ( 'NONE', #24049, #31166, #14269, .T. ) ;
#26991 = DIRECTION ( 'NONE',  ( -0.1155267958017759666, -0.9933043639548629899, 2.756973438308332598E-14 ) ) ;
#26992 = CARTESIAN_POINT ( 'NONE',  ( -10.69584247140444866, 85.44768628210144357, 6.932735513423972762 ) ) ;
#26993 = CARTESIAN_POINT ( 'NONE',  ( -14.38691631536207183, 21.33518628210144641, 5.770363421893814682 ) ) ;
#26994 = VECTOR ( 'NONE', #26762, 1000.000000000000000 ) ;
#26995 = CARTESIAN_POINT ( 'NONE',  ( 22.56230152254412857, -3.464101615137755275, -0.2625000000000429212 ) ) ;
#26996 =( BOUNDED_CURVE ( )  B_SPLINE_CURVE ( 2, ( #29872, #27401, #1055, #12813, #13009, #10157, #33095 ),
 .UNSPECIFIED., .F., .F. ) 
 B_SPLINE_CURVE_WITH_KNOTS ( ( 3, 2, 2, 3 ),
 ( 0.4347826086956553260, 0.4420289855072487284, 0.4492753623188421308, 0.4565217391304354777 ),
 .UNSPECIFIED. ) 
 CURVE ( )  GEOMETRIC_REPRESENTATION_ITEM ( )  RATIONAL_B_SPLINE_CURVE ( ( 0.9999999999999414912, 0.8660254037844972164, 1.000000000000000000, 0.8660254037844387076, 1.000000000000000000, 0.8660254037844253849, 1.000000000000013323 ) ) 
 REPRESENTATION_ITEM ( '' )  );
#26997 = DIRECTION ( 'NONE',  ( -0.000000000000000000, 1.000000000000000000, -0.000000000000000000 ) ) ;
#26998 = ORIENTED_EDGE ( 'NONE', *, *, #1630, .F. ) ;
#26999 = CARTESIAN_POINT ( 'NONE',  ( 13.23911966647218996, 44.04768628210143788, -8.632099005475504683 ) ) ;
#27000 = CARTESIAN_POINT ( 'NONE',  ( -13.62178482187498396, 197.6281250006145171, 23.59362340125808188 ) ) ;
#27001 = ADVANCED_FACE ( 'NONE', ( #2876 ), #5909, .F. ) ;
#27002 = CARTESIAN_POINT ( 'NONE',  ( 22.56230152254410370, 7.347880794884117764E-16, -0.5624999987710044280 ) ) ;
#27003 = DIRECTION ( 'NONE',  ( 0.000000000000000000, 0.000000000000000000, -1.000000000000000000 ) ) ;
#27004 = CARTESIAN_POINT ( 'NONE',  ( -31.99330436395490196, 210.1155267958017134, -6.500000000000000888 ) ) ;
#27005 = CARTESIAN_POINT ( 'NONE',  ( 25.36386068845838082, 0.000000000000000000, 168.7214353850716293 ) ) ;
#27006 = CARTESIAN_POINT ( 'NONE',  ( 7.228626920339068285, 25.07268628210144712, -10.49813415415989581 ) ) ;
#27007 = CARTESIAN_POINT ( 'NONE',  ( 21.00000000000000000, 249.5218750006145285, 6.646953231504538984 ) ) ;
#27008 = CARTESIAN_POINT ( 'NONE',  ( -8.152565276336593669, 126.9523137178985621, -5.233372021372610483 ) ) ;
#27009 = CARTESIAN_POINT ( 'NONE',  ( 20.99999999999999645, 245.4718750006145456, 6.646953231504538984 ) ) ;
#27010 = ORIENTED_EDGE ( 'NONE', *, *, #7177, .T. ) ;
#27011 = CARTESIAN_POINT ( 'NONE',  ( 18.00000000000000000, 5.196152422706630247, -7.275000000000003908 ) ) ;
#27012 = DIRECTION ( 'NONE',  ( -0.000000000000000000, -1.000000000000000000, -0.000000000000000000 ) ) ;
#27013 = VECTOR ( 'NONE', #34908, 1000.000000000000000 ) ;
#27014 = EDGE_CURVE ( 'NONE', #28321, #27758, #31539, .T. ) ;
#27015 = CARTESIAN_POINT ( 'NONE',  ( 0.1745138560722779009, 132.9898137178985564, 12.50000000000000355 ) ) ;
#27016 = CARTESIAN_POINT ( 'NONE',  ( 10.31873187879411091, -3.604726614523240613, -5.953124999385525307 ) ) ;
#27017 = CARTESIAN_POINT ( 'NONE',  ( 30.94637677943320497, -7.209453229046475009, 163.6876068119012189 ) ) ;
#27018 = CARTESIAN_POINT ( 'NONE',  ( 25.43903251657820164, 3.464101615137743728, 169.5806533121757411 ) ) ;
#27019 = CARTESIAN_POINT ( 'NONE',  ( -13.50000000000000533, 199.0250000000000057, -23.38268590217984411 ) ) ;
#27020 = CARTESIAN_POINT ( 'NONE',  ( -2.660918448318275509, 56.69768628210145067, 12.46528703574805874 ) ) ;
#27021 = ORIENTED_EDGE ( 'NONE', *, *, #4942, .T. ) ;
#27022 = ORIENTED_EDGE ( 'NONE', *, *, #9463, .F. ) ;
#27023 = CARTESIAN_POINT ( 'NONE',  ( -7.234628195640354420, 196.0424038105676630, 26.99999999999996803 ) ) ;
#27024 = CARTESIAN_POINT ( 'NONE',  ( 14.99999999999960387, -3.464101615137527457, -2.662500000000015188 ) ) ;
#27025 = DIRECTION ( 'NONE',  ( 1.000000000000000000, 0.000000000000000000, 0.000000000000000000 ) ) ;
#27026 = CARTESIAN_POINT ( 'NONE',  ( 19.39230484541326405, 248.2924038105676630, 5.999999999999995559 ) ) ;
#27027 = CARTESIAN_POINT ( 'NONE',  ( 21.00000000000000000, -6.646953231504538984, -8.578124999385442706 ) ) ;
#27028 = CARTESIAN_POINT ( 'NONE',  ( 8.962234695871762469, 98.96018628210146062, -8.715434833791931624 ) ) ;
#27029 = CARTESIAN_POINT ( 'NONE',  ( 14.25334919248795451, 19.71481371789854720, -6.092822981423661410 ) ) ;
#27030 = CARTESIAN_POINT ( 'NONE',  ( 26.99999999999999289, 0.000000000000000000, -8.000000000000000000 ) ) ;
#27031 = ADVANCED_FACE ( 'NONE', ( #28842 ), #14635, .F. ) ;
#27032 = CARTESIAN_POINT ( 'NONE',  ( 30.83116778204221475, 6.928203230275506996, 162.3707619459733564 ) ) ;
#27033 = CARTESIAN_POINT ( 'NONE',  ( -62.46502896937850124, 213.8393509191290889, -2.350049139982142155 ) ) ;
#27034 = CARTESIAN_POINT ( 'NONE',  ( 26.99999999999999645, 7.347880794884117764E-16, -1.124999999999987121 ) ) ;
#27035 = CARTESIAN_POINT ( 'NONE',  ( 28.27727295472088542, 5.196152422706630247, 167.6007502309489041 ) ) ;
#27036 = CARTESIAN_POINT ( 'NONE',  ( -12.46528703574811558, 144.2023137178985621, 2.660918448318003726 ) ) ;
#27037 = CARTESIAN_POINT ( 'NONE',  ( -47.62872103062154849, 203.4690446883607535, 1.626142955000567936 ) ) ;
#27038 = CARTESIAN_POINT ( 'NONE',  ( -34.75669563604515844, 209.8844732041981729, -8.500000000000003553 ) ) ;
#27039 = CONTEXT_DEPENDENT_SHAPE_REPRESENTATION ( #10035, #29217 ) ;
#27040 = CARTESIAN_POINT ( 'NONE',  ( 26.99999999999999645, 247.0749999999999886, -7.347880794884117764E-16 ) ) ;
#27041 = CARTESIAN_POINT ( 'NONE',  ( -1.926257025242585782E-15, 197.8906250006145342, -31.45816453501075927 ) ) ;
#27042 = CARTESIAN_POINT ( 'NONE',  ( -13.04141134922778456, 106.8273137178985479, 8.927990412390377273 ) ) ;
#27043 = CARTESIAN_POINT ( 'NONE',  ( -56.13169563604517265, 210.1155267958017703, 6.500000000000000888 ) ) ;
#27044 = CIRCLE ( 'NONE', #6479, 27.00000000000000355 ) ;
#27045 = EDGE_CURVE ( 'NONE', #8971, #19908, #8212, .T. ) ;
#27046 = VERTEX_POINT ( 'NONE', #25632 ) ;
#27047 = CARTESIAN_POINT ( 'NONE',  ( -12.46528703574805697, 22.19768628210145067, -2.660918448318280838 ) ) ;
#27048 = CARTESIAN_POINT ( 'NONE',  ( 18.00000000000000355, -5.196152422706632912, -6.225000000000008527 ) ) ;
#27049 = DIRECTION ( 'NONE',  ( 0.000000000000000000, 0.000000000000000000, 1.000000000000000000 ) ) ;
#27050 = CARTESIAN_POINT ( 'NONE',  ( 25.02235060511272735, 3.604726614523240613, 167.6126055182478183 ) ) ;
#27051 = CARTESIAN_POINT ( 'NONE',  ( 15.50000000000000533, 100.1101862821014521, 0.1745138560725827404 ) ) ;
#27052 = CARTESIAN_POINT ( 'NONE',  ( -61.87872103062155560, 203.4690446883607535, 1.626142955000567936 ) ) ;
#27053 = CARTESIAN_POINT ( 'NONE',  ( 10.31873187879411269, 3.604726614523236616, -3.778124999385508609 ) ) ;
#27054 = CARTESIAN_POINT ( 'NONE',  ( 3.796722387233379514, 61.58518628210146062, -8.710071997420127943 ) ) ;
#27055 = CYLINDRICAL_SURFACE ( 'NONE', #11000, 2.649999999999999467 ) ;
#27056 = CARTESIAN_POINT ( 'NONE',  ( -40.89955436395489841, 216.3070033484980002, -6.137860380172975638 ) ) ;
#27057 = CARTESIAN_POINT ( 'NONE',  ( 22.80587116629411781, 7.646167579472024665E-16, -9.871874999385521932 ) ) ;
#27058 = CARTESIAN_POINT ( 'NONE',  ( 12.53471296425194836, 72.22268628210143504, -2.311890736173178418 ) ) ;
#27059 = CYLINDRICAL_SURFACE ( 'NONE', #28749, 4.000000000000000888 ) ;
#27060 = CARTESIAN_POINT ( 'NONE',  ( 23.99999999999999645, 247.6562500012290400, -5.196152422706631135 ) ) ;
#27062 = VERTEX_POINT ( 'NONE', #29022 ) ;
#27061 = CARTESIAN_POINT ( 'NONE',  ( -9.534712964251941258, 40.02268628210144641, 1.715153634034234154 ) ) ;
#27063 = CARTESIAN_POINT ( 'NONE',  ( -9.000000000000024869, 215.5000000000000000, 6.735557395310435121E-16 ) ) ;
#27064 = EDGE_CURVE ( 'NONE', #21163, #31223, #37188, .T. ) ;
#27065 = CARTESIAN_POINT ( 'NONE',  ( 23.99999999999999645, 5.196152422706631135, -0.5999999999999894307 ) ) ;
#27066 = AXIS2_PLACEMENT_3D ( 'NONE', #22441, #13908, #25641 ) ;
#27067 = CARTESIAN_POINT ( 'NONE',  ( 25.24293209539582961, 3.464101615137650025, 167.3392152414693612 ) ) ;
#27068 = CARTESIAN_POINT ( 'NONE',  ( 34.28996860281051795, -5.407089921784861808, 166.0865723713108366 ) ) ;
#27069 = CARTESIAN_POINT ( 'NONE',  ( 30.91941297146709644, -6.928203230275514990, 163.3794090765669011 ) ) ;
#27070 = CARTESIAN_POINT ( 'NONE',  ( 18.00000000000000000, 246.3249999999999886, -5.196152422706630247 ) ) ;
#27071 = CARTESIAN_POINT ( 'NONE',  ( -27.24356964374999279, 196.6906250006145456, 15.72908226750539384 ) ) ;
#27072 = CARTESIAN_POINT ( 'NONE',  ( -10.49813415416004858, 97.62731371789855928, 7.228626920338839135 ) ) ;
#27073 = CARTESIAN_POINT ( 'NONE',  ( -12.53471296425194659, 113.6226862821014549, 2.311890736173176641 ) ) ;
#27074 = ORIENTED_EDGE ( 'NONE', *, *, #8314, .F. ) ;
#27075 = ORIENTED_EDGE ( 'NONE', *, *, #11087, .T. ) ;
#27076 = CARTESIAN_POINT ( 'NONE',  ( -27.24356964375000345, 195.7531250006145456, 0.000000000000000000 ) ) ;
#27077 = CARTESIAN_POINT ( 'NONE',  ( 18.12178482187500350, 240.3718750006145228, 4.985214923628407568 ) ) ;
#27078 = AXIS2_PLACEMENT_3D ( 'NONE', #9749, #12208, #30021 ) ;
#27079 = CARTESIAN_POINT ( 'NONE',  ( 14.25334919248795451, 84.11481371789855643, -6.092822981423661410 ) ) ;
#27080 = CARTESIAN_POINT ( 'NONE',  ( 21.00000000000000000, 6.646953231504538984, -7.115624999385463667 ) ) ;
#27081 = CARTESIAN_POINT ( 'NONE',  ( 15.24356964374999990, 245.3593750006145342, 0.000000000000000000 ) ) ;
#27082 = CARTESIAN_POINT ( 'NONE',  ( 3.796722387233379514, 98.38518628210145778, -8.710071997420127943 ) ) ;
#27083 = CARTESIAN_POINT ( 'NONE',  ( -26.99999999999998934, 194.7500000012290400, 15.58845726811991561 ) ) ;
#27084 = CARTESIAN_POINT ( 'NONE',  ( 7.954856959092311719, 65.42731371789857064, -5.529263428287300108 ) ) ;
#27085 = EDGE_CURVE ( 'NONE', #24290, #17896, #37133, .T. ) ;
#27086 = CARTESIAN_POINT ( 'NONE',  ( 10.31873187879410914, 0.000000000000000000, -7.790624999385542537 ) ) ;
#27087 = EDGE_CURVE ( 'NONE', #36527, #25890, #25996, .T. ) ;
#27088 = CARTESIAN_POINT ( 'NONE',  ( 9.500000000000005329, 121.4898137178985564, -0.1745138560723090149 ) ) ;
#27089 = CARTESIAN_POINT ( 'NONE',  ( 6.000769315822030740E-16, -20.00000000000000000, -4.899999999999999467 ) ) ;
#27090 = CARTESIAN_POINT ( 'NONE',  ( 2.660918448318002838, 22.30231371789854933, 12.46528703574811558 ) ) ;
#27091 = CARTESIAN_POINT ( 'NONE',  ( 37.19073179189800271, 7.347880794884117764E-16, 166.2186317273649934 ) ) ;
#27092 = CARTESIAN_POINT ( 'NONE',  ( 0.1745138560725515708, 88.61018628210146630, -12.50000000000000355 ) ) ;
#27093 = CARTESIAN_POINT ( 'NONE',  ( 10.56230152254411259, -3.464101615137757051, -6.599999998771014731 ) ) ;
#27094 = EDGE_CURVE ( 'NONE', #2407, #31898, #36402, .T. ) ;
#27095 = CARTESIAN_POINT ( 'NONE',  ( 15.24356964374999990, 0.000000000000000000, -0.2531249993854844949 ) ) ;
#27096 = CARTESIAN_POINT ( 'NONE',  ( 34.09877069215784218, -5.407089921784855591, 163.9011702523720544 ) ) ;
#27097 = CARTESIAN_POINT ( 'NONE',  ( 13.44051670066911619, -5.407089921784865361, -3.721874999385532679 ) ) ;
#27098 = CARTESIAN_POINT ( 'NONE',  ( -8.715434833791929847, 4.660186282101435928, -8.962234695871762469 ) ) ;
#27099 = DIRECTION ( 'NONE',  ( -2.057406622567553763E-16, 0.000000000000000000, 1.000000000000000000 ) ) ;
#27100 = CARTESIAN_POINT ( 'NONE',  ( -7.234628195640316228, 199.0075961894323200, -27.00000000000000000 ) ) ;
#27101 = CARTESIAN_POINT ( 'NONE',  ( 5.233372021372432847, 110.7476862821014691, 8.152565276336710909 ) ) ;
#27102 = CARTESIAN_POINT ( 'NONE',  ( 18.00000000000000355, 248.3312500012290513, 5.196152422706632912 ) ) ;
#27103 = CARTESIAN_POINT ( 'NONE',  ( -12.53471296425194836, 132.0226862821014606, 2.311890736173176641 ) ) ;
#27104 = CARTESIAN_POINT ( 'NONE',  ( 27.24356964375000700, 195.5468750006145342, 15.72908226750537075 ) ) ;
#27105 = CARTESIAN_POINT ( 'NONE',  ( 21.00000000000000000, 249.0718750006145399, 6.646953231504538984 ) ) ;
#27106 = ORIENTED_EDGE ( 'NONE', *, *, #4027, .F. ) ;
#27107 = CARTESIAN_POINT ( 'NONE',  ( 37.49302179100722299, 3.604726614523238837, 166.8791739800475113 ) ) ;
#27108 = CARTESIAN_POINT ( 'NONE',  ( 26.75643035624999655, 7.049594010296217766E-16, -3.065624999385479832 ) ) ;
#27109 = CARTESIAN_POINT ( 'NONE',  ( -27.24356964374999279, 199.4468750006145399, 15.72908226750539384 ) ) ;
#27110 = CARTESIAN_POINT ( 'NONE',  ( 19.95811783012822005, 240.0005236131589754, -5.908847734042844912 ) ) ;
#27111 = DIRECTION ( 'NONE',  ( -0.000000000000000000, 1.000000000000000000, -0.000000000000000000 ) ) ;
#27112 = CARTESIAN_POINT ( 'NONE',  ( 27.00000000000052580, 3.464101615137448409, -3.281249998770952025 ) ) ;
#27113 = CARTESIAN_POINT ( 'NONE',  ( 22.80587116629410360, -3.604726614523235284, -0.4031249993855248182 ) ) ;
#27114 = CARTESIAN_POINT ( 'NONE',  ( 6.594114490232462877, 28.33981371789855430, -6.840914352311949109 ) ) ;
#27115 = CARTESIAN_POINT ( 'NONE',  ( 27.24356964375000700, 196.4468750006145399, 15.72908226750537075 ) ) ;
#27117 = ORIENTED_EDGE ( 'NONE', *, *, #17824, .F. ) ;
#27116 = EDGE_LOOP ( 'NONE', ( #25853, #15841, #15212, #63 ) ) ;
#27118 = CARTESIAN_POINT ( 'NONE',  ( 26.75643035624999655, 245.9218750006145342, -7.049594010296217766E-16 ) ) ;
#27119 = CARTESIAN_POINT ( 'NONE',  ( -8.715434833792127023, 23.73981371789854578, 8.962234695871568846 ) ) ;
#27120 = CARTESIAN_POINT ( 'NONE',  ( 18.12178482187500350, -4.985214923628407568, -1.415624999385467486 ) ) ;
#27121 = CARTESIAN_POINT ( 'NONE',  ( 8.632099005475788900, 129.2523137178985451, -13.23911966647199812 ) ) ;
#27122 = CARTESIAN_POINT ( 'NONE',  ( 26.99999999999999645, 7.347880794884117764E-16, -10.06874999877094368 ) ) ;
#27123 = ORIENTED_EDGE ( 'NONE', *, *, #33667, .F. ) ;
#27124 = CARTESIAN_POINT ( 'NONE',  ( 19.68408634441911431, -5.407089921784861808, -5.896874999385542715 ) ) ;
#27125 = ORIENTED_EDGE ( 'NONE', *, *, #21473, .F. ) ;
#27126 = CARTESIAN_POINT ( 'NONE',  ( 13.62178482187501416, 195.9031250006145513, 23.59362340125806767 ) ) ;
#27127 = CARTESIAN_POINT ( 'NONE',  ( -8.962234695871760692, 140.3601862821014379, 8.715434833791933400 ) ) ;
#27128 = CARTESIAN_POINT ( 'NONE',  ( 30.98069435314010178, -7.209453229046482114, 164.0798584742748574 ) ) ;
#27129 = CARTESIAN_POINT ( 'NONE',  ( -53.16294563604516554, 216.1378603801729241, -6.307003348498026796 ) ) ;
#27130 = CARTESIAN_POINT ( 'NONE',  ( 15.24356964374999990, 246.1093750006145342, -3.323476615752268604 ) ) ;
#27131 = CARTESIAN_POINT ( 'NONE',  ( 20.99999999999999289, 240.4374999999999716, -5.999999999999997335 ) ) ;
#27132 = CARTESIAN_POINT ( 'NONE',  ( -42.07961230271182984, 211.3212981617417938, 4.469044688360757966 ) ) ;
#27133 = CARTESIAN_POINT ( 'NONE',  ( 6.932735513423970097, 129.1476862821014890, 10.69584247140445044 ) ) ;
#27134 = CARTESIAN_POINT ( 'NONE',  ( 37.45053336641773711, 7.646167579472015790E-16, 166.3935290647278009 ) ) ;
#27135 = ORIENTED_EDGE ( 'NONE', *, *, #1487, .T. ) ;
#27136 = CARTESIAN_POINT ( 'NONE',  ( 34.30346624845981296, -5.196152422706635576, 167.6381752909151999 ) ) ;
#27137 = CARTESIAN_POINT ( 'NONE',  ( 2.908627838312458636, 9.077313717898549683, -15.53471296425188442 ) ) ;
#27138 = CARTESIAN_POINT ( 'NONE',  ( -47.62872103062157692, 201.4690446883607819, 2.162041339862843525 ) ) ;
#27139 = CARTESIAN_POINT ( 'NONE',  ( -6.840914352312096547, 131.1601862821014777, 6.594114490232313663 ) ) ;
#27140 = CARTESIAN_POINT ( 'NONE',  ( -14.50000000000000533, 237.0000000000000000, 2.500000000000000000 ) ) ;
#27141 = CARTESIAN_POINT ( 'NONE',  ( -11.61527771782819940, 30.53518628210144570, 4.622313124798574258 ) ) ;
#27143 = EDGE_CURVE ( 'NONE', #21628, #9483, #22155, .T. ) ;
#27142 = CARTESIAN_POINT ( 'NONE',  ( 16.56230152254411436, 6.928203230275514990, -6.862500000000055778 ) ) ;
#27144 = UNCERTAINTY_MEASURE_WITH_UNIT (LENGTH_MEASURE( 1.000000000000000082E-05 ), #6853, 'distance_accuracy_value', 'NONE');
#27145 = CIRCLE ( 'NONE', #23492, 3.500000000000002665 ) ;
#27146 = ORIENTED_EDGE ( 'NONE', *, *, #9642, .T. ) ;
#27147 = FILL_AREA_STYLE ('',( #18446 ) ) ;
#27148 = CARTESIAN_POINT ( 'NONE',  ( -15.50000000000000533, 123.1101862821014663, -0.1745138560725808530 ) ) ;
#27149 = DIRECTION ( 'NONE',  ( -0.000000000000000000, -0.000000000000000000, -1.000000000000000000 ) ) ;
#27150 = CARTESIAN_POINT ( 'NONE',  ( -6.840914352311947333, 136.4398137178985735, -6.594114490232462877 ) ) ;
#27151 = CARTESIAN_POINT ( 'NONE',  ( 13.62178482187499640, 199.6531250006145228, -23.59362340125807123 ) ) ;
#27152 = CARTESIAN_POINT ( 'NONE',  ( 7.234628195640309123, 195.9299038117966916, -27.00000000000000711 ) ) ;
#27153 = CARTESIAN_POINT ( 'NONE',  ( -13.62178482187498396, 199.4843750006145626, 23.59362340125808188 ) ) ;
#27154 = CARTESIAN_POINT ( 'NONE',  ( 36.98155800919708014, -3.464101615137448409, 163.8277644507203661 ) ) ;
#27155 = CARTESIAN_POINT ( 'NONE',  ( 15.08037007377155803, 0.2408480140671711567, -8.000000000000021316 ) ) ;
#27156 = CARTESIAN_POINT ( 'NONE',  ( 33.72823834632531259, 5.196152422706637353, 161.0632902835097013 ) ) ;
#27157 = CARTESIAN_POINT ( 'NONE',  ( 3.796722387233182339, 77.21481371789855075, 8.710071997420207879 ) ) ;
#27158 = VERTEX_POINT ( 'NONE', #12549 ) ;
#27159 = CARTESIAN_POINT ( 'NONE',  ( 26.99999999999999645, 244.4312500012290457, -7.347880794884117764E-16 ) ) ;
#27160 = CARTESIAN_POINT ( 'NONE',  ( 6.932735513424201024, 74.05231371789855643, -10.69584247140429412 ) ) ;
#27161 = CARTESIAN_POINT ( 'NONE',  ( 22.80587116629411781, 3.604726614523243278, -4.434374999385503280 ) ) ;
#27162 = CARTESIAN_POINT ( 'NONE',  ( -27.24356964374999990, 199.7656250006145342, -15.72908226750537786 ) ) ;
#27163 = CARTESIAN_POINT ( 'NONE',  ( 26.75643035624999655, 7.049594010296217766E-16, -4.978124999385491023 ) ) ;
#27164 = CARTESIAN_POINT ( 'NONE',  ( -4.944772684328424539, 54.21481371789854364, -11.48171059495408031 ) ) ;
#27165 = EDGE_LOOP ( 'NONE', ( #2338, #10188, #2591, #11488, #8797, #18043, #35032, #30755, #27209, #20405, #561, #23670 ) ) ;
#27166 = CARTESIAN_POINT ( 'NONE',  ( 25.02068495149662297, 0.000000000000000000, 164.7989187625597367 ) ) ;
#27167 = CARTESIAN_POINT ( 'NONE',  ( 18.12178482187500350, 244.8718750006145228, 4.985214923628407568 ) ) ;
#27168 = CARTESIAN_POINT ( 'NONE',  ( 7.228626920339068285, 15.87268628210144961, -10.49813415415989581 ) ) ;
#27169 = CARTESIAN_POINT ( 'NONE',  ( -41.09002896937850124, 204.4285982733020433, 3.350049139982171020 ) ) ;
#27170 = CARTESIAN_POINT ( 'NONE',  ( -60.68377896937848703, 208.3738570449995109, 6.530955311639247363 ) ) ;
#27171 =( LENGTH_UNIT ( ) NAMED_UNIT ( * ) SI_UNIT ( .MILLI., .METRE. ) );
#27172 = CARTESIAN_POINT ( 'NONE',  ( 24.62521576877915308, 3.464101615137752166, 160.2786853199683890 ) ) ;
#27173 = CARTESIAN_POINT ( 'NONE',  ( -4.944772684328424539, 81.81481371789855928, -11.48171059495408031 ) ) ;
#27174 = CARTESIAN_POINT ( 'NONE',  ( -49.40997103062157692, 213.8393509191290889, 2.350049139982164359 ) ) ;
#27175 = CARTESIAN_POINT ( 'NONE',  ( -52.18080436395490551, 203.5000000000000000, -0.1155267958017335561 ) ) ;
#27176 = CARTESIAN_POINT ( 'NONE',  ( 20.99999999999999645, -6.646953231504538984, -7.790624999385473259 ) ) ;
#27177 = CARTESIAN_POINT ( 'NONE',  ( 19.56230152254410370, 5.196152422706631135, -0.9374999987709908833 ) ) ;
#27178 = CARTESIAN_POINT ( 'NONE',  ( -5.770363421894122880, 50.76481371789856212, 14.38691631536194393 ) ) ;
#27179 = CARTESIAN_POINT ( 'NONE',  ( -50.59002896937850835, 202.6965474657332038, 4.350049139982197666 ) ) ;
#27180 = CARTESIAN_POINT ( 'NONE',  ( 1.069080835302379631E-14, 199.6625000000000227, 27.00000000000000000 ) ) ;
#27181 = CARTESIAN_POINT ( 'NONE',  ( 4.944772684328679446, 89.18518628210145494, -11.48171059495397373 ) ) ;
#27182 = CARTESIAN_POINT ( 'NONE',  ( -8.927990412390661490, 20.47268628210143859, 13.04141134922759804 ) ) ;
#27183 = DIRECTION ( 'NONE',  ( -1.000000000000000000, -6.123233995736766036E-17, 0.000000000000000000 ) ) ;
#27184 = CARTESIAN_POINT ( 'NONE',  ( 20.99999999999999645, 185.0294372515228645, 5.999999999999999112 ) ) ;
#27185 = ORIENTED_EDGE ( 'NONE', *, *, #18939, .F. ) ;
#27186 = CARTESIAN_POINT ( 'NONE',  ( 13.04141134922759804, 45.77268628210144641, 8.927990412390657937 ) ) ;
#27187 = CARTESIAN_POINT ( 'NONE',  ( -13.62178482187498396, 198.5281250006145228, 23.59362340125808188 ) ) ;
#27188 = DIRECTION ( 'NONE',  ( -0.000000000000000000, -0.000000000000000000, 1.000000000000000000 ) ) ;
#27189 = LINE ( 'NONE', #6922, #116 ) ;
#27190 = LINE ( 'NONE', #1214, #6298 ) ;
#27191 = CARTESIAN_POINT ( 'NONE',  ( 0.000000000000000000, 148.0000000000000000, 0.000000000000000000 ) ) ;
#27192 = CARTESIAN_POINT ( 'NONE',  ( 4.622313124798573369, 28.23518628210144854, 11.61527771782819940 ) ) ;
#27193 = CARTESIAN_POINT ( 'NONE',  ( 18.12178482187499640, 249.3343750006145285, -4.985214923628404904 ) ) ;
#27194 = CARTESIAN_POINT ( 'NONE',  ( 3.796722387233182339, 132.4148137178985678, 8.710071997420207879 ) ) ;
#27195 = CARTESIAN_POINT ( 'NONE',  ( 18.12178482187499640, 244.3843750006145115, -4.985214923628404904 ) ) ;
#27196 = ORIENTED_EDGE ( 'NONE', *, *, #2732, .F. ) ;
#27197 = CARTESIAN_POINT ( 'NONE',  ( -42.59364919042334208, 252.0388376121882175, 5.000000000000000000 ) ) ;
#27198 = CARTESIAN_POINT ( 'NONE',  ( 11.48171059495408208, 130.1148137178985564, -4.944772684328420986 ) ) ;
#27199 = CARTESIAN_POINT ( 'NONE',  ( 10.31873187879410914, 0.000000000000000000, -5.990624999385518734 ) ) ;
#27200 = CARTESIAN_POINT ( 'NONE',  ( 24.87037277869651319, 3.604726614523236616, 165.8754910134502722 ) ) ;
#27201 =( BOUNDED_SURFACE ( )  B_SPLINE_SURFACE ( 1, 2, ( 
 ( #19144, #28211, #19705, #14000, #22726, #30694, #34273, #19888, #5451, #31430, #17034, #28572, #24807, #33527, #4711, #19335, #16291, #13439, #24989, #10589, #30874, #16478, #28024, #141, #8865, #28949, #17222, #325, #20626, #20442, #26290, #14187, #28760, #11890, #35194, #23458, #35012, #31985, #34822, #14743, #20066, #32168, #2986, #6013, #2799, #12076, #6206, #25739, #34456, #509, #17597, #14555, #14371, #29512, #11521, #20252, #26108, #23651, #20815, #34635, #29128, #3170, #11704, #23279, #31611, #8681, #9242, #17778, #25927, #37471, #9055, #23091, #29321, #3360, #32357, #31792, #14930, #5829, #17408, #26476, #6396, #17969, #8498, #37291, #11339, #22911, #5637, #30805, #13368, #13751, #22282, #19265, #36476, #36849, #5201, #24923, #8058, #33835, #10517, #11080, #1985, #13556, #31179, #10336, #19073, #28139, #25110, #19446, #24739, #25297, #16777, #10893, #27585, #22654, #5381, #34201, #7873, #33456, #30996, #21907, #4827, #27772, #22096, #19633, #30625, #36289, #36667, #16595, #16408, #1614, #8246, #13934, #10705, #27954, #4642, #13184, #33646, #7685, #5015, #37033, #19820, #2169, #22465, #34012, #28322, #2360, #7497, #25482, #31356, #16221, #1801, #17151, #18039, #28687, #9314, #768, #26927, #5566, #32425, #23021, #20179, #17334, #31727, #2727, #11268, #15378, #35259, #34569, #8609, #37222, #14301, #8428, #22838, #28878, #25854, #11452, #32615, #6470, #19997, #14484, #28504, #21264, #37402, #5756, #34386, #2912, #26038, #31541, #2547, #16961, #66, #20885, #26734, #25666, #29583, #18229, #3621, #15187, #957, #12337, #23910, #35452, #11632, #9502, #23720, #21078, #6653, #29769, #3800, #12532, #24096, #35642, #9687, #32803, #14114, #1146, #18981, #13281, #25020, #7598, #21820, #7410, #21633, #30539, #29963, #15756, #24649, #33184, #19173, #4557, #15946, #10434, #7228, #30343, #1521, #18801, #9870, #16132, #24835, #13094, #27684, #6840, #21452, #1709, #27865, #36388, #22007, #36199, #27500, #33560, #12716, #30722, #4368, #10243, #32991, #4743, #16317, #18418, #27122, #33372, #1897, #22197, #3991, #13468, #36577, #15565, #10618, #36018, #24285 ),
 ( #35830, #7044, #18611, #30155, #4184, #27307, #1337, #12907, #24472, #10057, #2271, #4924, #20093, #36946, #19544, #19915, #28416, #25396, #5115, #5479, #11367, #31092, #14215, #2456, #16694, #17247, #8162, #19736, #37317, #16505, #25214, #34301, #31274, #25580, #30903, #31456, #22938, #17062, #33745, #28788, #11547, #2825, #14029, #2088, #37132, #28053, #10992, #33929, #28242, #25765, #36765, #13662, #5300, #22752, #22563, #7784, #14396, #22380, #34484, #11178, #8344, #8527, #25953, #31639, #34110, #37496, #16880, #28600, #19363, #2637, #10807, #5666, #13848, #7970, #14582, #9270, #11919, #168, #26692, #23121, #17997, #35220, #11733, #20281, #3759, #32008, #21032, #917, #34664, #31821, #23486, #26885, #35037, #5856, #20841, #26317, #32383, #34851, #6610, #17433, #12101, #23305, #15333, #17807, #9082, #20652, #28972, #6423, #3012, #32198, #6233, #23866, #29540, #29349, #721, #3388, #14958, #26504, #354, #26134, #3579, #15141, #535, #12294, #8708, #8891, #35406, #18184, #9455, #32569, #23675, #29726, #20469, #6038, #17625, #29154, #3196, #14772, #10389, #18941, #24053, #32760, #36344, #33144, #1290, #15525, #27825, #9829, #18570, #12861, #21965, #19129, #32946, #7188, #15904, #10013, #27265, #18371, #7000, #33511, #4515, #24241, #12673, #13055, #35787, #4325, #33329, #7555, #1105, #27450, #30112, #15714, #24428, #35977, #21407, #6797, #30678, #30299, #4142, #21594, #29918, #18757, #3949, #27080, #1480, #24610, #36159, #27641, #10205, #21779, #7369, #35599, #16278, #30493, #16089, #1670, #13244, #24793, #4697, #9644, #12486, #21221, #5257, #11136, #10575, #31228, #2596, #28375, #2411, #11321, #34255, #37088, #16834, #4884, #19689, #36722, #34068, #8298, #25536, #8117, #25722, #10762, #13984, #16464, #28194, #22713, #33699, #19870, #31414, #20048, #14167, #5433, #17014, #16651, #28555, #24972, #22334, #37274, #22890, #34439, #8479, #22522, #31594, #7738, #5618, #2224, #17202, #28008, #1855, #13424, #36531, #22152, #19322, #30859, #13805, #2040, #13619, #33886, #7928, #25353, #25168, #19502, #31049, #5070, #36900, #10948, #5996, #34618, #23260 ) ),
 .UNSPECIFIED., .F., .F., .F. ) 
 B_SPLINE_SURFACE_WITH_KNOTS ( ( 2, 2 ),
 ( 3, 2, 2, 2, 2, 2, 2, 2, 2, 2, 2, 2, 2, 2, 2, 2, 2, 2, 2, 2, 2, 2, 2, 2, 2, 2, 2, 2, 2, 2, 2, 2, 2, 2, 2, 2, 2, 2, 2, 2, 2, 2, 2, 2, 2, 2, 2, 2, 2, 2, 2, 2, 2, 2, 2, 2, 2, 2, 2, 2, 2, 2, 2, 2, 2, 2, 2, 2, 2, 2, 2, 2, 2, 2, 2, 2, 2, 2, 2, 2, 2, 2, 2, 2, 2, 2, 2, 2, 2, 2, 2, 2, 2, 2, 2, 2, 2, 2, 2, 2, 2, 2, 2, 2, 2, 2, 2, 2, 2, 2, 2, 2, 2, 2, 2, 2, 2, 2, 2, 2, 2, 2, 2, 2, 2, 2, 2, 2, 2, 2, 2, 2, 2, 2, 3 ),
 ( 0.000000000000000000, 1.000000000000000000 ),
 ( 0.000000000000000000, 0.007246376811594202987, 0.01449275362318840597, 0.02173913043478260809, 0.02898550724637681195, 0.03623188405797101580, 0.04347826086956521618, 0.05072463768115942351, 0.05797101449275362389, 0.06521739130434782428, 0.07246376811594203160, 0.07971014492753622505, 0.08695652173913043237, 0.09420289855072463969, 0.1014492753623188470, 0.1086956521739130405, 0.1159420289855072478, 0.1231884057971014551, 0.1304347826086956486, 0.1376811594202898559, 0.1449275362318840632, 0.1521739130434782705, 0.1594202898550724501, 0.1666666666666666574, 0.1739130434782608647, 0.1811594202898550721, 0.1884057971014492794, 0.1956521739130434867, 0.2028985507246376940, 0.2101449275362318736, 0.2173913043478260809, 0.2246376811594202882, 0.2318840579710144956, 0.2391304347826087029, 0.2463768115942029102, 0.2536231884057971175, 0.2608695652173912971, 0.2681159420289855322, 0.2753623188405797118, 0.2826086956521738913, 0.2898550724637681264, 0.2971014492753623060, 0.3043478260869565410, 0.3115942028985507206, 0.3188405797101449002, 0.3260869565217391353, 0.3333333333333333148, 0.3405797101449275499, 0.3478260869565217295, 0.3550724637681159646, 0.3623188405797101441, 0.3695652173913043237, 0.3768115942028985588, 0.3840579710144927383, 0.3913043478260869734, 0.3985507246376811530, 0.4057971014492753881, 0.4130434782608695676, 0.4202898550724637472, 0.4275362318840579823, 0.4347826086956521618, 0.4420289855072463969, 0.4492753623188405765, 0.4565217391304347561, 0.4637681159420289911, 0.4710144927536231707, 0.4782608695652174058, 0.4855072463768115854, 0.4927536231884058204, 0.5000000000000000000, 0.5072463768115942351, 0.5144927536231883591, 0.5217391304347825942, 0.5289855072463768293, 0.5362318840579710644, 0.5434782608695651884, 0.5507246376811594235, 0.5579710144927536586, 0.5652173913043477826, 0.5724637681159420177, 0.5797101449275362528, 0.5869565217391304879, 0.5942028985507246119, 0.6014492753623188470, 0.6086956521739130821, 0.6159420289855072062, 0.6231884057971014412, 0.6304347826086956763, 0.6376811594202898004, 0.6449275362318840354, 0.6521739130434782705, 0.6594202898550725056, 0.6666666666666666297, 0.6739130434782608647, 0.6811594202898550998, 0.6884057971014492239, 0.6956521739130434590, 0.7028985507246376940, 0.7101449275362319291, 0.7173913043478260532, 0.7246376811594202882, 0.7318840579710145233, 0.7391304347826086474, 0.7463768115942028825, 0.7536231884057971175, 0.7608695652173913526, 0.7681159420289854767, 0.7753623188405797118, 0.7826086956521739468, 0.7898550724637680709, 0.7971014492753623060, 0.8043478260869565410, 0.8115942028985507761, 0.8188405797101449002, 0.8260869565217391353, 0.8333333333333333703, 0.8405797101449274944, 0.8478260869565217295, 0.8550724637681159646, 0.8623188405797101996, 0.8695652173913043237, 0.8768115942028985588, 0.8840579710144927938, 0.8913043478260869179, 0.8985507246376811530, 0.9057971014492753881, 0.9130434782608695121, 0.9202898550724637472, 0.9275362318840579823, 0.9347826086956522174, 0.9420289855072463414, 0.9492753623188405765, 0.9565217391304348116, 0.9637681159420289356, 0.9662082966761270653 ),
 .UNSPECIFIED. ) 
 GEOMETRIC_REPRESENTATION_ITEM ( )  RATIONAL_B_SPLINE_SURFACE ( (
 ( 1.000000000000000000, 0.8660254037844387076, 1.000000000000000000, 0.8660254037844387076, 1.000000000000000000, 0.8660254037844387076, 1.000000000000000000, 0.8660254037844387076, 1.000000000000000000, 0.8660254037844387076, 1.000000000000000000, 0.8660254037844387076, 1.000000000000000000, 0.8660254037844387076, 1.000000000000000000, 0.8660254037844387076, 1.000000000000000000, 0.8660254037844387076, 1.000000000000000000, 0.8660254037844387076, 1.000000000000000000, 0.8660254037844387076, 1.000000000000000000, 0.8660254037844387076, 1.000000000000000000, 0.8660254037844387076, 1.000000000000000000, 0.8660254037844387076, 1.000000000000000000, 0.8660254037844387076, 1.000000000000000000, 0.8660254037844387076, 1.000000000000000000, 0.8660254037844387076, 1.000000000000000000, 0.8660254037844387076, 1.000000000000000000, 0.8660254037844387076, 1.000000000000000000, 0.8660254037844387076, 1.000000000000000000, 0.8660254037844387076, 1.000000000000000000, 0.8660254037844387076, 1.000000000000000000, 0.8660254037844387076, 1.000000000000000000, 0.8660254037844387076, 1.000000000000000000, 0.8660254037844387076, 1.000000000000000000, 0.8660254037844387076, 1.000000000000000000, 0.8660254037844387076, 1.000000000000000000, 0.8660254037844387076, 1.000000000000000000, 0.8660254037844387076, 1.000000000000000000, 0.8660254037844387076, 1.000000000000000000, 0.8660254037844387076, 1.000000000000000000, 0.8660254037844387076, 1.000000000000000000, 0.8660254037844387076, 1.000000000000000000, 0.8660254037844387076, 1.000000000000000000, 0.8660254037844387076, 1.000000000000000000, 0.8660254037844387076, 1.000000000000000000, 0.8660254037844387076, 1.000000000000000000, 0.8660254037844387076, 1.000000000000000000, 0.8660254037844387076, 1.000000000000000000, 0.8660254037844387076, 1.000000000000000000, 0.8660254037844387076, 1.000000000000000000, 0.8660254037844387076, 1.000000000000000000, 0.8660254037844387076, 1.000000000000000000, 0.8660254037844387076, 1.000000000000000000, 0.8660254037844387076, 1.000000000000000000, 0.8660254037844387076, 1.000000000000000000, 0.8660254037844387076, 1.000000000000000000, 0.8660254037844387076, 1.000000000000000000, 0.8660254037844387076, 1.000000000000000000, 0.8660254037844387076, 1.000000000000000000, 0.8660254037844387076, 1.000000000000000000, 0.8660254037844387076, 1.000000000000000000, 0.8660254037844387076, 1.000000000000000000, 0.8660254037844387076, 1.000000000000000000, 0.8660254037844387076, 1.000000000000000000, 0.8660254037844387076, 1.000000000000000000, 0.8660254037844387076, 1.000000000000000000, 0.8660254037844387076, 1.000000000000000000, 0.8660254037844387076, 1.000000000000000000, 0.8660254037844387076, 1.000000000000000000, 0.8660254037844387076, 1.000000000000000000, 0.8660254037844387076, 1.000000000000000000, 0.8660254037844387076, 1.000000000000000000, 0.8660254037844387076, 1.000000000000000000, 0.8660254037844387076, 1.000000000000000000, 0.8660254037844387076, 1.000000000000000000, 0.8660254037844387076, 1.000000000000000000, 0.8660254037844387076, 1.000000000000000000, 0.8660254037844387076, 1.000000000000000000, 0.8660254037844387076, 1.000000000000000000, 0.8660254037844387076, 1.000000000000000000, 0.8660254037844387076, 1.000000000000000000, 0.8660254037844387076, 1.000000000000000000, 0.8660254037844387076, 1.000000000000000000, 0.8660254037844387076, 1.000000000000000000, 0.8660254037844387076, 1.000000000000000000, 0.8660254037844387076, 1.000000000000000000, 0.8660254037844387076, 1.000000000000000000, 0.8660254037844387076, 1.000000000000000000, 0.8660254037844387076, 1.000000000000000000, 0.8660254037844387076, 1.000000000000000000, 0.8660254037844387076, 1.000000000000000000, 0.8660254037844387076, 1.000000000000000000, 0.8660254037844387076, 1.000000000000000000, 0.8660254037844387076, 1.000000000000000000, 0.8660254037844387076, 1.000000000000000000, 0.8660254037844387076, 1.000000000000000000, 0.8660254037844387076, 1.000000000000000000, 0.8660254037844387076, 1.000000000000000000, 0.8660254037844387076, 1.000000000000000000, 0.8660254037844387076, 1.000000000000000000, 0.8660254037844387076, 1.000000000000000000, 0.8660254037844387076, 1.000000000000000000, 0.8660254037844387076, 1.000000000000000000, 0.8660254037844387076, 1.000000000000000000, 0.8660254037844387076, 1.000000000000000000, 0.8660254037844387076, 1.000000000000000000, 0.8660254037844387076, 1.000000000000000000, 0.8660254037844387076, 1.000000000000000000, 0.8660254037844387076, 1.000000000000000000, 0.8660254037844387076, 1.000000000000000000, 0.8660254037844387076, 1.000000000000000000, 0.8660254037844387076, 1.000000000000000000, 0.8660254037844387076, 1.000000000000000000, 0.8660254037844387076, 1.000000000000000000, 0.8660254037844387076, 1.000000000000000000, 0.8660254037844387076, 1.000000000000000000, 0.8660254037844387076, 1.000000000000000000, 0.8660254037844387076, 1.000000000000000000, 0.8660254037844387076, 1.000000000000000000, 0.8660254037844387076, 1.000000000000000000, 0.8660254037844387076, 1.000000000000000000, 0.8660254037844387076, 1.000000000000000000, 0.8660254037844387076, 1.000000000000000000, 0.8660254037844387076, 1.000000000000000000, 0.8660254037844387076, 1.000000000000000000, 0.8660254037844387076, 1.000000000000000000, 0.8660254037844387076, 1.000000000000000000, 0.8660254037844387076, 1.000000000000000000, 0.8660254037844387076, 1.000000000000000000, 0.8660254037844387076, 1.000000000000000000, 0.8660254037844387076, 1.000000000000000000, 0.8660254037844387076, 1.000000000000000000, 0.8660254037844387076, 1.000000000000000000, 0.8660254037844387076, 1.000000000000000000, 0.8660254037844387076, 1.000000000000000000, 0.8660254037844387076, 1.000000000000000000, 0.8660254037844387076, 1.000000000000000000, 0.8660254037844387076, 1.000000000000000000, 0.8660254037844387076, 1.000000000000000000, 0.8660254037844387076, 1.000000000000000000, 0.8660254037844387076, 1.000000000000000000, 0.8660254037844387076, 1.000000000000000000, 0.9548847324609573972, 0.9401541411607521326),
 ( 1.000000000000000000, 0.8660254037844387076, 1.000000000000000000, 0.8660254037844387076, 1.000000000000000000, 0.8660254037844387076, 1.000000000000000000, 0.8660254037844387076, 1.000000000000000000, 0.8660254037844387076, 1.000000000000000000, 0.8660254037844387076, 1.000000000000000000, 0.8660254037844387076, 1.000000000000000000, 0.8660254037844387076, 1.000000000000000000, 0.8660254037844387076, 1.000000000000000000, 0.8660254037844387076, 1.000000000000000000, 0.8660254037844387076, 1.000000000000000000, 0.8660254037844387076, 1.000000000000000000, 0.8660254037844387076, 1.000000000000000000, 0.8660254037844387076, 1.000000000000000000, 0.8660254037844387076, 1.000000000000000000, 0.8660254037844387076, 1.000000000000000000, 0.8660254037844387076, 1.000000000000000000, 0.8660254037844387076, 1.000000000000000000, 0.8660254037844387076, 1.000000000000000000, 0.8660254037844387076, 1.000000000000000000, 0.8660254037844387076, 1.000000000000000000, 0.8660254037844387076, 1.000000000000000000, 0.8660254037844387076, 1.000000000000000000, 0.8660254037844387076, 1.000000000000000000, 0.8660254037844387076, 1.000000000000000000, 0.8660254037844387076, 1.000000000000000000, 0.8660254037844387076, 1.000000000000000000, 0.8660254037844387076, 1.000000000000000000, 0.8660254037844387076, 1.000000000000000000, 0.8660254037844387076, 1.000000000000000000, 0.8660254037844387076, 1.000000000000000000, 0.8660254037844387076, 1.000000000000000000, 0.8660254037844387076, 1.000000000000000000, 0.8660254037844387076, 1.000000000000000000, 0.8660254037844387076, 1.000000000000000000, 0.8660254037844387076, 1.000000000000000000, 0.8660254037844387076, 1.000000000000000000, 0.8660254037844387076, 1.000000000000000000, 0.8660254037844387076, 1.000000000000000000, 0.8660254037844387076, 1.000000000000000000, 0.8660254037844387076, 1.000000000000000000, 0.8660254037844387076, 1.000000000000000000, 0.8660254037844387076, 1.000000000000000000, 0.8660254037844387076, 1.000000000000000000, 0.8660254037844387076, 1.000000000000000000, 0.8660254037844387076, 1.000000000000000000, 0.8660254037844387076, 1.000000000000000000, 0.8660254037844387076, 1.000000000000000000, 0.8660254037844387076, 1.000000000000000000, 0.8660254037844387076, 1.000000000000000000, 0.8660254037844387076, 1.000000000000000000, 0.8660254037844387076, 1.000000000000000000, 0.8660254037844387076, 1.000000000000000000, 0.8660254037844387076, 1.000000000000000000, 0.8660254037844387076, 1.000000000000000000, 0.8660254037844387076, 1.000000000000000000, 0.8660254037844387076, 1.000000000000000000, 0.8660254037844387076, 1.000000000000000000, 0.8660254037844387076, 1.000000000000000000, 0.8660254037844387076, 1.000000000000000000, 0.8660254037844387076, 1.000000000000000000, 0.8660254037844387076, 1.000000000000000000, 0.8660254037844387076, 1.000000000000000000, 0.8660254037844387076, 1.000000000000000000, 0.8660254037844387076, 1.000000000000000000, 0.8660254037844387076, 1.000000000000000000, 0.8660254037844387076, 1.000000000000000000, 0.8660254037844387076, 1.000000000000000000, 0.8660254037844387076, 1.000000000000000000, 0.8660254037844387076, 1.000000000000000000, 0.8660254037844387076, 1.000000000000000000, 0.8660254037844387076, 1.000000000000000000, 0.8660254037844387076, 1.000000000000000000, 0.8660254037844387076, 1.000000000000000000, 0.8660254037844387076, 1.000000000000000000, 0.8660254037844387076, 1.000000000000000000, 0.8660254037844387076, 1.000000000000000000, 0.8660254037844387076, 1.000000000000000000, 0.8660254037844387076, 1.000000000000000000, 0.8660254037844387076, 1.000000000000000000, 0.8660254037844387076, 1.000000000000000000, 0.8660254037844387076, 1.000000000000000000, 0.8660254037844387076, 1.000000000000000000, 0.8660254037844387076, 1.000000000000000000, 0.8660254037844387076, 1.000000000000000000, 0.8660254037844387076, 1.000000000000000000, 0.8660254037844387076, 1.000000000000000000, 0.8660254037844387076, 1.000000000000000000, 0.8660254037844387076, 1.000000000000000000, 0.8660254037844387076, 1.000000000000000000, 0.8660254037844387076, 1.000000000000000000, 0.8660254037844387076, 1.000000000000000000, 0.8660254037844387076, 1.000000000000000000, 0.8660254037844387076, 1.000000000000000000, 0.8660254037844387076, 1.000000000000000000, 0.8660254037844387076, 1.000000000000000000, 0.8660254037844387076, 1.000000000000000000, 0.8660254037844387076, 1.000000000000000000, 0.8660254037844387076, 1.000000000000000000, 0.8660254037844387076, 1.000000000000000000, 0.8660254037844387076, 1.000000000000000000, 0.8660254037844387076, 1.000000000000000000, 0.8660254037844387076, 1.000000000000000000, 0.8660254037844387076, 1.000000000000000000, 0.8660254037844387076, 1.000000000000000000, 0.8660254037844387076, 1.000000000000000000, 0.8660254037844387076, 1.000000000000000000, 0.8660254037844387076, 1.000000000000000000, 0.8660254037844387076, 1.000000000000000000, 0.8660254037844387076, 1.000000000000000000, 0.8660254037844387076, 1.000000000000000000, 0.8660254037844387076, 1.000000000000000000, 0.8660254037844387076, 1.000000000000000000, 0.8660254037844387076, 1.000000000000000000, 0.8660254037844387076, 1.000000000000000000, 0.8660254037844387076, 1.000000000000000000, 0.8660254037844387076, 1.000000000000000000, 0.8660254037844387076, 1.000000000000000000, 0.8660254037844387076, 1.000000000000000000, 0.8660254037844387076, 1.000000000000000000, 0.8660254037844387076, 1.000000000000000000, 0.8660254037844387076, 1.000000000000000000, 0.8660254037844387076, 1.000000000000000000, 0.8660254037844387076, 1.000000000000000000, 0.8660254037844387076, 1.000000000000000000, 0.8660254037844387076, 1.000000000000000000, 0.8660254037844387076, 1.000000000000000000, 0.8660254037844387076, 1.000000000000000000, 0.8660254037844387076, 1.000000000000000000, 0.8660254037844387076, 1.000000000000000000, 0.8660254037844387076, 1.000000000000000000, 0.8660254037844387076, 1.000000000000000000, 0.8660254037844387076, 1.000000000000000000, 0.9548847324609573972, 0.9401541411607521326) ) ) 
 REPRESENTATION_ITEM ( '' )  SURFACE ( )  );
#27202 = FACE_OUTER_BOUND ( 'NONE', #34887, .T. ) ;
#27203 = CARTESIAN_POINT ( 'NONE',  ( 13.49999999999999645, 198.0500000000000114, -23.38268590217984766 ) ) ;
#27204 = EDGE_CURVE ( 'NONE', #19175, #21723, #35408, .T. ) ;
#27205 = ORIENTED_EDGE ( 'NONE', *, *, #23044, .F. ) ;
#27206 = CARTESIAN_POINT ( 'NONE',  ( -8.962234695871760692, 48.36018628210145209, 8.715434833791933400 ) ) ;
#27207 = ORIENTED_EDGE ( 'NONE', *, *, #34894, .T. ) ;
#27208 = B_SPLINE_CURVE_WITH_KNOTS ( 'NONE', 3,
 ( #7085, #4220, #35869, #15798, #36058, #27348, #12949, #21306, #24510, #9911, #6887, #24877, #36242, #18839, #15422, #30194, #21671, #26968, #15989, #9542, #32655, #4406, #7449, #12573 ),
 .UNSPECIFIED., .F., .F.,
 ( 4, 2, 2, 2, 2, 2, 2, 2, 2, 2, 2, 4 ),
 ( 0.01193646315038279955, 0.01204987972134695558, 0.01216329629231111160, 0.01239012943423942539, 0.01284379571809604950, 0.01375112828580929251, 0.01556579342123577854, 0.01647312598894901808, 0.01738045855666225936, 0.01919512369208874192, 0.02282445396294170009, 0.02645378423379465826 ),
 .UNSPECIFIED. ) ;
#27209 = ORIENTED_EDGE ( 'NONE', *, *, #17535, .F. ) ;
#27210 = LINE ( 'NONE', #669, #14597 ) ;
#27211 = CARTESIAN_POINT ( 'NONE',  ( 26.75643035624999655, 3.323476615752271268, -0.3281249993854667424 ) ) ;
#27212 = DIRECTION ( 'NONE',  ( 0.000000000000000000, 0.000000000000000000, 1.000000000000000000 ) ) ;
#27213 = CARTESIAN_POINT ( 'NONE',  ( -27.00000000000000355, 198.3125000012290400, 0.000000000000000000 ) ) ;
#27214 = CARTESIAN_POINT ( 'NONE',  ( 15.24356964374999990, 0.000000000000000000, -8.690624999385471838 ) ) ;
#27215 = CARTESIAN_POINT ( 'NONE',  ( 12.53471296425194836, 72.22268628210143504, -2.311890736173178418 ) ) ;
#27216 = CARTESIAN_POINT ( 'NONE',  ( -14.38691631536193860, 16.26481371789853370, -5.770363421894132649 ) ) ;
#27217 = CARTESIAN_POINT ( 'NONE',  ( 22.56230152254410370, 0.000000000000000000, -10.00000000000000000 ) ) ;
#27218 = CARTESIAN_POINT ( 'NONE',  ( 7.405590309535792670, 215.0979036339245170, 3.170162721592201471 ) ) ;
#27219 = CARTESIAN_POINT ( 'NONE',  ( -56.52752896937850124, 212.3500491399821613, 3.839350919129088435 ) ) ;
#27220 = CARTESIAN_POINT ( 'NONE',  ( 10.56230152254410548, 0.000000000000000000, -4.050000000000054001 ) ) ;
#27221 = CARTESIAN_POINT ( 'NONE',  ( 25.29849388150476130, -3.464101615137757051, 167.9742893627271769 ) ) ;
#27222 = CARTESIAN_POINT ( 'NONE',  ( 6.594114490232462877, 9.939813717898537959, -6.840914352311949109 ) ) ;
#27223 = CARTESIAN_POINT ( 'NONE',  ( -42.28497103062156270, 204.4285982733020148, -3.350049139982115509 ) ) ;
#27224 = CARTESIAN_POINT ( 'NONE',  ( -64.05580436395490551, 218.5000000000000000, 0.1155267958017064944 ) ) ;
#27225 =( BOUNDED_CURVE ( )  B_SPLINE_CURVE ( 2, ( #18854, #30402, #36443, #10671, #1581, #30961, #22250 ),
 .UNSPECIFIED., .F., .F. ) 
 B_SPLINE_CURVE_WITH_KNOTS ( ( 3, 2, 2, 3 ),
 ( 0.6739130434782596435, 0.6811594202898539896, 0.6884057971014481137, 0.6956521739130424598 ),
 .UNSPECIFIED. ) 
 CURVE ( )  GEOMETRIC_REPRESENTATION_ITEM ( )  RATIONAL_B_SPLINE_CURVE ( ( 1.000000000000022649, 0.8660254037844161701, 1.000000000000000000, 0.8660254037844387076, 1.000000000000000000, 0.8660254037844571373, 0.9999999999999815703 ) ) 
 REPRESENTATION_ITEM ( '' )  );
#27226 = ITEM_DEFINED_TRANSFORMATION ( 'NONE', 'NONE', #28692,  #17215 ) ;
#27227 = CARTESIAN_POINT ( 'NONE',  ( 22.60769515458672174, 246.9825961894323427, 6.000000000000004441 ) ) ;
#27228 = CARTESIAN_POINT ( 'NONE',  ( 27.24356964375000345, 199.1281250006145171, -3.336375036156643733E-15 ) ) ;
#27229 = CARTESIAN_POINT ( 'NONE',  ( 13.04141134922778988, 120.6273137178985451, -8.927990412390371944 ) ) ;
#27230 = CARTESIAN_POINT ( 'NONE',  ( -47.22544563604515844, 214.8429017333602360, 4.673758765035156415 ) ) ;
#27231 = EDGE_CURVE ( 'NONE', #15520, #35499, #9458, .T. ) ;
#27232 = VERTEX_POINT ( 'NONE', #26753 ) ;
#27233 = CARTESIAN_POINT ( 'NONE',  ( 6.932735513423970097, 18.74768628210143717, 10.69584247140445044 ) ) ;
#27234 = CARTESIAN_POINT ( 'NONE',  ( 2.999999999999997335, 244.5000000000000000, -2.499999999999999556 ) ) ;
#27235 = CARTESIAN_POINT ( 'NONE',  ( 26.99999999999999645, 7.347880794884117764E-16, -4.275000000000001243 ) ) ;
#27236 = CARTESIAN_POINT ( 'NONE',  ( 31.13757469008587719, -7.209453229046482114, 165.8730089308399442 ) ) ;
#27237 = VECTOR ( 'NONE', #24993, 1000.000000000000000 ) ;
#27238 = CARTESIAN_POINT ( 'NONE',  ( 5.770363421893814682, 111.0351862821014635, 14.38691631536207183 ) ) ;
#27239 = CARTESIAN_POINT ( 'NONE',  ( -49.60788769728822700, 216.4690446883607535, 1.857196546604031662 ) ) ;
#27240 = CARTESIAN_POINT ( 'NONE',  ( 19.68408634441910721, -5.407089921784855591, -4.040624999385538985 ) ) ;
#27241 = CARTESIAN_POINT ( 'NONE',  ( 7.954856959092191815, 36.57268628210144357, 5.529263428287477744 ) ) ;
#27242 = CYLINDRICAL_SURFACE ( 'NONE', #25532, 5.999999999999998224 ) ;
#27243 = CARTESIAN_POINT ( 'NONE',  ( -38.72247103062156981, 205.6499508600178956, 7.303452534266880569 ) ) ;
#27244 = CARTESIAN_POINT ( 'NONE',  ( -3.253724281355068545E-15, 198.9874999999999829, -27.00000000000000355 ) ) ;
#27245 = CARTESIAN_POINT ( 'NONE',  ( 12.50000000000000355, 72.51018628210145778, 0.1745138560725507937 ) ) ;
#27246 = CARTESIAN_POINT ( 'NONE',  ( 26.99999999999999645, 7.347880794884117764E-16, -7.818749998770941012 ) ) ;
#27247 = CARTESIAN_POINT ( 'NONE',  ( 19.56230152254411792, -5.196152422706629359, -7.837499998771035870 ) ) ;
#27249 = ORIENTED_EDGE ( 'NONE', *, *, #2981, .F. ) ;
#27248 = CARTESIAN_POINT ( 'NONE',  ( 6.840914352312096547, 52.96018628210144641, -6.594114490232313663 ) ) ;
#27250 = CARTESIAN_POINT ( 'NONE',  ( 15.02283181144952628, 7.347880794884122694E-16, 50.52293445648592751 ) ) ;
#27251 = ORIENTED_EDGE ( 'NONE', *, *, #6200, .T. ) ;
#27252 = CARTESIAN_POINT ( 'NONE',  ( 18.00000000000000000, 5.196152422706630247, -0.9750000000000036415 ) ) ;
#27253 = CARTESIAN_POINT ( 'NONE',  ( 22.56230152254411792, 7.347880794884125653E-16, -6.525000000000058975 ) ) ;
#27254 = CARTESIAN_POINT ( 'NONE',  ( 37.05016167317072728, -3.604726614523238837, 161.8172596703688271 ) ) ;
#27255 = CARTESIAN_POINT ( 'NONE',  ( 27.80990028412949755, -5.196152422706638241, 162.2586561612075116 ) ) ;
#27256 = CARTESIAN_POINT ( 'NONE',  ( 26.99999999999999645, 245.7249999999999943, -7.347880794884117764E-16 ) ) ;
#27257 = CARTESIAN_POINT ( 'NONE',  ( 13.62178482187501416, 197.2531250006145456, 23.59362340125806767 ) ) ;
#27258 = CARTESIAN_POINT ( 'NONE',  ( -4.622313124798826500, 105.9648137178985650, 11.61527771782809637 ) ) ;
#27259 = CARTESIAN_POINT ( 'NONE',  ( -11.48171059495397373, 105.2851862821014493, -4.944772684328680334 ) ) ;
#27260 = ORIENTED_EDGE ( 'NONE', *, *, #18977, .T. ) ;
#27261 = ORIENTED_EDGE ( 'NONE', *, *, #15030, .T. ) ;
#27262 = CARTESIAN_POINT ( 'NONE',  ( 5.727106289114498080E-15, 199.3250000012290570, 31.17691453623979214 ) ) ;
#27263 = CARTESIAN_POINT ( 'NONE',  ( 15.24356964374999990, 240.7093750006145285, -3.323476615752268604 ) ) ;
#27264 = CARTESIAN_POINT ( 'NONE',  ( 6.092822981423662299, 68.01481371789854791, 14.25334919248795096 ) ) ;
#27265 = CARTESIAN_POINT ( 'NONE',  ( 15.24356964374999990, 0.000000000000000000, -6.103124999385478588 ) ) ;
#27266 = CARTESIAN_POINT ( 'NONE',  ( 26.75643035624999655, 244.2343750006145342, -7.049594010296217766E-16 ) ) ;
#27267 = CARTESIAN_POINT ( 'NONE',  ( -2.064181346179269738, 93.49768628210142651, 9.465287035748067623 ) ) ;
#27268 =( BOUNDED_CURVE ( )  B_SPLINE_CURVE ( 2, ( #13401, #7715, #13219, #33675, #36138, #18919, #24770, #30656, #5046 ),
 .UNSPECIFIED., .F., .F. ) 
 B_SPLINE_CURVE_WITH_KNOTS ( ( 3, 2, 2, 2, 3 ),
 ( 0.3369565217391304324, 0.3405797101449275499, 0.3478260869565217295, 0.3550724637681159646, 0.3586956521739130266 ),
 .UNSPECIFIED. ) 
 CURVE ( )  GEOMETRIC_REPRESENTATION_ITEM ( )  RATIONAL_B_SPLINE_CURVE ( ( 0.9330127018922194093, 0.9330127018922194093, 1.000000000000000000, 0.8660254037844387076, 1.000000000000000000, 0.8660254037844387076, 1.000000000000000000, 0.9330127018922198534, 0.9330127018922191873 ) ) 
 REPRESENTATION_ITEM ( '' )  );
#27269 = CARTESIAN_POINT ( 'NONE',  ( 6.594114490232462877, 65.13981371789854791, -6.840914352311949109 ) ) ;
#27270 = CARTESIAN_POINT ( 'NONE',  ( 19.68408634441910721, 5.407089921784857367, -7.040624999385541649 ) ) ;
#27271 = CARTESIAN_POINT ( 'NONE',  ( 5.233372021372610483, 110.8523137178985252, -8.152565276336593669 ) ) ;
#27272 = CARTESIAN_POINT ( 'NONE',  ( 27.00000000000000355, 197.9750000000000227, -3.306546357697854128E-15 ) ) ;
#27273 = CARTESIAN_POINT ( 'NONE',  ( 12.53471296425189330, 38.97731371789855359, 2.311890736173451977 ) ) ;
#27274 = CARTESIAN_POINT ( 'NONE',  ( 12.50000000000000355, 81.71018628210144641, 0.1745138560725507937 ) ) ;
#27275 = CARTESIAN_POINT ( 'NONE',  ( 10.56230152254411436, 3.464101615137752166, -6.674999998771008691 ) ) ;
#27276 = FACE_OUTER_BOUND ( 'NONE', #10464, .T. ) ;
#27277 = CARTESIAN_POINT ( 'NONE',  ( 37.25770128558855987, 3.604726614523238837, 164.1894482951998100 ) ) ;
#27278 = CARTESIAN_POINT ( 'NONE',  ( 13.44051670066911264, -5.407089921784865361, -3.271874999385554261 ) ) ;
#27279 = CARTESIAN_POINT ( 'NONE',  ( -3.253724281355068545E-15, 197.6374999999999602, -27.00000000000000000 ) ) ;
#27280 = PLANE ( 'NONE',  #12181 ) ;
#27281 = DIRECTION ( 'NONE',  ( 0.08715574274765150453, 0.000000000000000000, 0.9961946980917461003 ) ) ;
#27282 = CARTESIAN_POINT ( 'NONE',  ( -8.843639120294326972, 104.1351862821014720, 3.474262827703335166 ) ) ;
#27283 = CARTESIAN_POINT ( 'NONE',  ( 26.99999999999999645, 7.347880794884117764E-16, -4.218749998770948473 ) ) ;
#27284 = CARTESIAN_POINT ( 'NONE',  ( 10.69584247140445221, 136.0476862821014379, -6.932735513423970097 ) ) ;
#27285 = CARTESIAN_POINT ( 'NONE',  ( -6.439089545781193635, 143.0000000000000284, 10.42254124200965748 ) ) ;
#27286 = CARTESIAN_POINT ( 'NONE',  ( 26.75643035624999655, 249.6343750006145399, -7.049594010296217766E-16 ) ) ;
#27288 = ORIENTED_EDGE ( 'NONE', *, *, #24015, .F. ) ;
#27287 = VECTOR ( 'NONE', #20288, 1000.000000000000000 ) ;
#27289 = CARTESIAN_POINT ( 'NONE',  ( 34.34716455898865206, 5.407089921784857367, 166.7403251419335390 ) ) ;
#27290 = CARTESIAN_POINT ( 'NONE',  ( 18.12178482187499640, 4.985214923628404904, -2.915624999385468819 ) ) ;
#27291 = CARTESIAN_POINT ( 'NONE',  ( 10.56230152254411081, 0.000000000000000000, -5.287499998771011178 ) ) ;
#27292 = CARTESIAN_POINT ( 'NONE',  ( 25.18083362879568199, -3.464101615137894719, 166.6294265203033262 ) ) ;
#27293 = CARTESIAN_POINT ( 'NONE',  ( 37.37702719191401002, 7.347880794884125653E-16, 168.3479978933117422 ) ) ;
#27294 = CARTESIAN_POINT ( 'NONE',  ( 26.99999999999999645, 7.347880794884117764E-16, -3.318749998770964549 ) ) ;
#27295 = CARTESIAN_POINT ( 'NONE',  ( 21.00000000000000000, 243.8968750006145001, -6.646953231504538984 ) ) ;
#27296 = CARTESIAN_POINT ( 'NONE',  ( 19.68408634441910721, -5.407089921784855591, -3.140624999385555061 ) ) ;
#27297 = CARTESIAN_POINT ( 'NONE',  ( -6.840914352311947333, 26.03981371789855714, -6.594114490232462877 ) ) ;
#27298 = CARTESIAN_POINT ( 'NONE',  ( 27.24356964375000345, 196.0343750006145456, -3.336375036156643733E-15 ) ) ;
#27300 = VERTEX_POINT ( 'NONE', #784 ) ;
#27299 = ORIENTED_EDGE ( 'NONE', *, *, #34611, .F. ) ;
#27301 = CARTESIAN_POINT ( 'NONE',  ( 18.12178482187499640, 246.9718750006145171, -4.985214923628404904 ) ) ;
#27302 = CARTESIAN_POINT ( 'NONE',  ( -7.228626920338836470, 26.32731371789855146, -10.49813415416005213 ) ) ;
#27303 = EDGE_CURVE ( 'NONE', #15380, #1047, #12353, .T. ) ;
#27304 = CARTESIAN_POINT ( 'NONE',  ( 26.75643035624999655, -3.323476615752267715, -1.753124999385447857 ) ) ;
#27305 = CARTESIAN_POINT ( 'NONE',  ( -11.08355503943118592, 127.2398137178985422, -10.83675517735179383 ) ) ;
#27306 = EDGE_CURVE ( 'NONE', #36429, #10880, #9293, .T. ) ;
#27307 = CARTESIAN_POINT ( 'NONE',  ( 26.75643035624999655, 3.323476615752271712, -0.4406249993854897129 ) ) ;
#27308 = ORIENTED_EDGE ( 'NONE', *, *, #4065, .T. ) ;
#27309 = CARTESIAN_POINT ( 'NONE',  ( 13.44051670066911441, -5.407089921784865361, -7.321874999385524774 ) ) ;
#27310 = ORIENTED_EDGE ( 'NONE', *, *, #24057, .T. ) ;
#27311 = CARTESIAN_POINT ( 'NONE',  ( 27.24356964374999635, 196.9156250006145399, -15.72908226750539029 ) ) ;
#27312 = CARTESIAN_POINT ( 'NONE',  ( 4.944772684328679446, 135.1851862821014549, -11.48171059495397373 ) ) ;
#27313 = CARTESIAN_POINT ( 'NONE',  ( 27.94596069312478903, -5.407089921784865361, 165.2111578762278157 ) ) ;
#27314 = EDGE_CURVE ( 'NONE', #21721, #36429, #1761, .T. ) ;
#27315 = AXIS2_PLACEMENT_3D ( 'NONE', #33274, #30437, #4456 ) ;
#27316 = VECTOR ( 'NONE', #14230, 1000.000000000000000 ) ;
#27317 = CARTESIAN_POINT ( 'NONE',  ( -53.36086230271183695, 214.1499508600178387, -7.418979330068641964 ) ) ;
#27318 = CARTESIAN_POINT ( 'NONE',  ( 23.87821517812500005, 247.6468750006145285, 4.985214923628404016 ) ) ;
#27319 = FACE_BOUND ( 'NONE', #12618, .T. ) ;
#27320 = CARTESIAN_POINT ( 'NONE',  ( -40.10044563604517265, 206.6211998817775566, -3.209657149897419348 ) ) ;
#27321 = CARTESIAN_POINT ( 'NONE',  ( 15.00000000000000000, 245.9124999999999943, -3.464101615137752610 ) ) ;
#27322 = CARTESIAN_POINT ( 'NONE',  ( 31.12286715849720409, 7.209453229046475009, 165.7049010755369807 ) ) ;
#27323 = ORIENTED_EDGE ( 'NONE', *, *, #36921, .T. ) ;
#27324 = CARTESIAN_POINT ( 'NONE',  ( 1.069080835302379631E-14, 198.3124999999999716, 27.00000000000000000 ) ) ;
#27325 = CARTESIAN_POINT ( 'NONE',  ( 5.770363421893814682, 129.4351862821014549, 14.38691631536207183 ) ) ;
#27326 = CARTESIAN_POINT ( 'NONE',  ( -52.97247103062156270, 205.6499508600178956, 7.303452534266880569 ) ) ;
#27327 = ADVANCED_BREP_SHAPE_REPRESENTATION ( '', ( #20661, #17215 ), #27435 ) ;
#27328 = CARTESIAN_POINT ( 'NONE',  ( 5.529263428287477744, 117.0726862821014294, -7.954856959092191815 ) ) ;
#27329 = CARTESIAN_POINT ( 'NONE',  ( 18.00000000000000000, 246.3812500012290343, -5.196152422706630247 ) ) ;
#27330 = CARTESIAN_POINT ( 'NONE',  ( 6.932735513423970097, 18.74768628210143717, 10.69584247140445044 ) ) ;
#27331 = CARTESIAN_POINT ( 'NONE',  ( 19.56230152254412502, -5.196152422706635576, -7.950000000000068567 ) ) ;
#27332 = EDGE_LOOP ( 'NONE', ( #12228, #7129, #8656, #10638 ) ) ;
#27333 = CARTESIAN_POINT ( 'NONE',  ( -15.53471296425195369, 113.6226862821014549, 2.908627838312118019 ) ) ;
#27334 = LINE ( 'NONE', #1365, #20587 ) ;
#27335 = CARTESIAN_POINT ( 'NONE',  ( 8.710071997420127943, 8.685186282101437172, 3.796722387233375073 ) ) ;
#27336 = VECTOR ( 'NONE', #20350, 1000.000000000000000 ) ;
#27337 = CARTESIAN_POINT ( 'NONE',  ( -27.24356964374999990, 198.4156250006145399, -15.72908226750537786 ) ) ;
#27338 = DIRECTION ( 'NONE',  ( -0.000000000000000000, 1.000000000000000000, -0.000000000000000000 ) ) ;
#27339 = CARTESIAN_POINT ( 'NONE',  ( 27.24356964374999635, 199.6718750006145058, -15.72908226750539029 ) ) ;
#27340 = CARTESIAN_POINT ( 'NONE',  ( 10.56230152254363119, 3.464101615137481716, -5.437500000000037303 ) ) ;
#27341 = CARTESIAN_POINT ( 'NONE',  ( 22.56230152254410370, 0.000000000000000000, -10.00000000000000000 ) ) ;
#27342 = CARTESIAN_POINT ( 'NONE',  ( 6.594114490232462877, 74.33981371789855075, -6.840914352311949109 ) ) ;
#27343 = ORIENTED_EDGE ( 'NONE', *, *, #30568, .F. ) ;
#27344 = VECTOR ( 'NONE', #6773, 1000.000000000000000 ) ;
#27345 = CARTESIAN_POINT ( 'NONE',  ( 15.00000000000000000, 244.2062500012290513, 0.000000000000000000 ) ) ;
#27346 = CARTESIAN_POINT ( 'NONE',  ( 0.1745138560722779009, 77.78981371789855359, 12.50000000000000355 ) ) ;
#27347 = CARTESIAN_POINT ( 'NONE',  ( 16.56230152254411436, 7.209453229046482114, -4.809374999385505944 ) ) ;
#27348 = CARTESIAN_POINT ( 'NONE',  ( -6.693455383991767427, 142.9999999999999147, 10.84641480984770467 ) ) ;
#27349 = CARTESIAN_POINT ( 'NONE',  ( 23.87821517812500005, -4.985214923628404016, -4.153124999385471305 ) ) ;
#27350 = CARTESIAN_POINT ( 'NONE',  ( 8.715434833792128799, 55.93981371789855217, -8.962234695871567070 ) ) ;
#27351 = ORIENTED_EDGE ( 'NONE', *, *, #34661, .F. ) ;
#27352 = CARTESIAN_POINT ( 'NONE',  ( 15.24356964374999990, 0.000000000000000000, -6.890624999385474680 ) ) ;
#27353 = CARTESIAN_POINT ( 'NONE',  ( 21.00000000000000000, 243.5593750006145228, 6.646953231504538984 ) ) ;
#27354 = CARTESIAN_POINT ( 'NONE',  ( -7.228626920339069173, 29.67268628210144499, 10.49813415415989581 ) ) ;
#27355 = CARTESIAN_POINT ( 'NONE',  ( -35.35044563604516554, 205.1570982666397072, -4.673758765035155527 ) ) ;
#27356 = CARTESIAN_POINT ( 'NONE',  ( -50.78794563604515133, 205.3262412349647832, 4.842901733360250205 ) ) ;
#27357 = VECTOR ( 'NONE', #23095, 1000.000000000000000 ) ;
#27358 = CARTESIAN_POINT ( 'NONE',  ( 27.64975160693779443, 5.196152422706630247, 160.4281484046883293 ) ) ;
#27359 = CARTESIAN_POINT ( 'NONE',  ( 10.49813415416005213, 83.82731371789856212, -7.228626920338837358 ) ) ;
#27360 = CARTESIAN_POINT ( 'NONE',  ( -41.29538769728824121, 211.3212981617418222, -4.469044688360751749 ) ) ;
#27361 = CARTESIAN_POINT ( 'NONE',  ( -62.07663769728823411, 204.3130714775002730, 3.149950860017883603 ) ) ;
#27362 = CARTESIAN_POINT ( 'NONE',  ( 7.234628195640269155, 195.7450961906613713, 27.00000000000003197 ) ) ;
#27363 = CARTESIAN_POINT ( 'NONE',  ( 18.00000000000000000, 5.196152422706630247, -2.324999999999993960 ) ) ;
#27364 = CARTESIAN_POINT ( 'NONE',  ( -15.50000000000000533, 61.68981371789855928, 0.1745138560722471477 ) ) ;
#27365 = CARTESIAN_POINT ( 'NONE',  ( -47.62127896937850124, 218.5309553116392465, 2.162041339862725842 ) ) ;
#27366 = CARTESIAN_POINT ( 'NONE',  ( 21.00000000000000355, 0.000000000000000000, 50.00000000000001421 ) ) ;
#27367 = CARTESIAN_POINT ( 'NONE',  ( -11.48171059495397373, 77.68518628210145494, -4.944772684328680334 ) ) ;
#27368 = CARTESIAN_POINT ( 'NONE',  ( 5.770363421893814682, 19.03518628210144570, 14.38691631536207183 ) ) ;
#27369 = CARTESIAN_POINT ( 'NONE',  ( 10.56230152254410903, 0.000000000000000000, -0.4500000000000614619 ) ) ;
#27370 = CARTESIAN_POINT ( 'NONE',  ( -27.87471972953270338, 210.0000000000000284, -8.000000000000000000 ) ) ;
#27371 = ORIENTED_EDGE ( 'NONE', *, *, #26140, .F. ) ;
#27372 = CARTESIAN_POINT ( 'NONE',  ( -14.38691631536207183, 39.73518628210145209, 5.770363421893814682 ) ) ;
#27373 = CARTESIAN_POINT ( 'NONE',  ( 27.24356964375000700, 196.8406250006145228, 15.72908226750537075 ) ) ;
#27374 = LINE ( 'NONE', #36086, #36200 ) ;
#27375 = CARTESIAN_POINT ( 'NONE',  ( 30.84097280299421229, -6.928203230275514990, 162.4828338482843151 ) ) ;
#27376 = CARTESIAN_POINT ( 'NONE',  ( -38.92038769728823411, 208.1428034533959703, 6.469044688360770401 ) ) ;
#27377 = CARTESIAN_POINT ( 'NONE',  ( 28.34590810202754696, 5.196152422706636465, 168.3852535544717739 ) ) ;
#27378 = CARTESIAN_POINT ( 'NONE',  ( -0.1745138560725500443, 28.81018628210144072, 12.50000000000000355 ) ) ;
#27379 = CARTESIAN_POINT ( 'NONE',  ( 15.24356964375000167, 248.9968750006145513, 3.323476615752272600 ) ) ;
#27380 = CARTESIAN_POINT ( 'NONE',  ( -9.500000000000005329, 135.2898137178985394, 0.1745138560723101806 ) ) ;
#27381 = CARTESIAN_POINT ( 'NONE',  ( 26.75643035624999655, 245.1343750006145115, -7.049594010296217766E-16 ) ) ;
#27382 = ORIENTED_EDGE ( 'NONE', *, *, #35289, .T. ) ;
#27383 = CARTESIAN_POINT ( 'NONE',  ( 20.99999999999999645, -6.928203230275506996, -4.387499999999998401 ) ) ;
#27384 = CARTESIAN_POINT ( 'NONE',  ( -7.228626920338836470, 127.5273137178985792, -10.49813415416005213 ) ) ;
#27385 = CARTESIAN_POINT ( 'NONE',  ( 16.56230152254411081, 7.209453229046475009, -7.903124999385497063 ) ) ;
#27386 = CARTESIAN_POINT ( 'NONE',  ( 37.29038468911893034, -3.604726614523235284, 164.5630213069841830 ) ) ;
#27387 = DIRECTION ( 'NONE',  ( 0.000000000000000000, 0.000000000000000000, -1.000000000000000000 ) ) ;
#27388 = CARTESIAN_POINT ( 'NONE',  ( -13.49999999999998401, 196.4750000000000227, 23.38268590217985476 ) ) ;
#27389 = EDGE_LOOP ( 'NONE', ( #33373, #7734, #5612, #1568 ) ) ;
#27390 = CARTESIAN_POINT ( 'NONE',  ( -10.49813415415989404, 31.97268628210143859, -7.228626920339069173 ) ) ;
#27391 = EDGE_LOOP ( 'NONE', ( #23143, #35844, #29815, #33496, #6995 ) ) ;
#27392 = ORIENTED_EDGE ( 'NONE', *, *, #37182, .F. ) ;
#27393 = CARTESIAN_POINT ( 'NONE',  ( -6.000000000000000888, -20.00000000000000000, -19.99999999999999289 ) ) ;
#27394 = LINE ( 'NONE', #30626, #10451 ) ;
#27395 = LINE ( 'NONE', #27956, #13678 ) ;
#27396 = FACE_OUTER_BOUND ( 'NONE', #32447, .T. ) ;
#27397 = CARTESIAN_POINT ( 'NONE',  ( 21.00000000000000000, 6.646953231504538984, -7.903124999385464200 ) ) ;
#27398 = CARTESIAN_POINT ( 'NONE',  ( 12.50000000000000355, 81.71018628210144641, 0.1745138560725507937 ) ) ;
#27399 = CARTESIAN_POINT ( 'NONE',  ( 0.1745138560725837118, 134.6101862821014947, -15.50000000000000533 ) ) ;
#27400 = CARTESIAN_POINT ( 'NONE',  ( 19.56230152254411436, -5.196152422706629359, -3.787499998771037824 ) ) ;
#27401 = CARTESIAN_POINT ( 'NONE',  ( 10.56230152254562604, 3.464101615138625689, -4.874999998771045284 ) ) ;
#27402 = CARTESIAN_POINT ( 'NONE',  ( -50.59002896937850835, 206.1606490808709111, 2.350049139982143931 ) ) ;
#27403 = CARTESIAN_POINT ( 'NONE',  ( -5.732297079746171420, 222.9518338469886203, 2.500000000000000000 ) ) ;
#27404 = CARTESIAN_POINT ( 'NONE',  ( 31.32141883499775403, -6.928203230275506996, 167.9743571227394341 ) ) ;
#27405 = CARTESIAN_POINT ( 'NONE',  ( 0.1745138560722779009, 142.1898137178985735, 12.50000000000000355 ) ) ;
#27406 = CARTESIAN_POINT ( 'NONE',  ( -41.88913769728823411, 206.8500491399821044, -5.686928522499717253 ) ) ;
#27407 = CARTESIAN_POINT ( 'NONE',  ( -53.36830436395490551, 209.8844732041983150, 8.500000000000003553 ) ) ;
#27408 = PRODUCT_CONTEXT ( 'NONE', #34708, 'mechanical' ) ;
#27409 = CARTESIAN_POINT ( 'NONE',  ( 10.56230152254410903, 7.347880794884117764E-16, -10.00000000000000000 ) ) ;
#27410 = CARTESIAN_POINT ( 'NONE',  ( 5.778771075727756162E-15, 199.0156250006145342, 31.45816453501075927 ) ) ;
#27411 = CARTESIAN_POINT ( 'NONE',  ( -10.83675517735179028, 115.7398137178985564, 11.08355503943118947 ) ) ;
#27412 = CARTESIAN_POINT ( 'NONE',  ( -45.44419563604516554, 203.5000000000000000, 0.1155267958017914542 ) ) ;
#27413 = ORIENTED_EDGE ( 'NONE', *, *, #10539, .T. ) ;
#27414 = DIRECTION ( 'NONE',  ( 0.08715574274765150453, 0.000000000000000000, 0.9961946980917461003 ) ) ;
#27415 = VECTOR ( 'NONE', #33457, 1000.000000000000000 ) ;
#27416 = EDGE_CURVE ( 'NONE', #30158, #16958, #35470, .T. ) ;
#27417 = FACE_OUTER_BOUND ( 'NONE', #24852, .T. ) ;
#27418 = CARTESIAN_POINT ( 'NONE',  ( 24.86873860851999041, 0.000000000000000000, 165.8568123628610920 ) ) ;
#27419 = CARTESIAN_POINT ( 'NONE',  ( -8.927990412390661490, 103.2726862821014322, 13.04141134922759804 ) ) ;
#27420 = CARTESIAN_POINT ( 'NONE',  ( -59.89955436395489841, 214.8429017333601792, -4.673758765035197271 ) ) ;
#27421 = CARTESIAN_POINT ( 'NONE',  ( 22.80587116629410716, 3.604726614523238837, -3.028124999385537475 ) ) ;
#27422 =( BOUNDED_CURVE ( )  B_SPLINE_CURVE ( 2, ( #16895, #2475, #17265, #9100, #28805, #25597, #3030, #8542, #14232 ),
 .UNSPECIFIED., .F., .T. ) 
 B_SPLINE_CURVE_WITH_KNOTS ( ( 3, 2, 2, 2, 3 ),
 ( 0.4891304347826087029, 0.4927536231884058204, 0.5000000000000000000, 0.5072463768115942351, 0.5108695652173913526 ),
 .UNSPECIFIED. ) 
 CURVE ( )  GEOMETRIC_REPRESENTATION_ITEM ( )  RATIONAL_B_SPLINE_CURVE ( ( 0.9330127018922194093, 0.9330127018922194093, 1.000000000000000000, 0.8660254037844387076, 1.000000000000000000, 0.8660254037844387076, 1.000000000000000000, 0.9330127018922182991, 0.9330127018922192983 ) ) 
 REPRESENTATION_ITEM ( '' )  );
#27423 = CARTESIAN_POINT ( 'NONE',  ( -5.529263428287477744, 48.07268628210143646, 7.954856959092191815 ) ) ;
#27424 = CARTESIAN_POINT ( 'NONE',  ( 19.39230484541326760, 240.6986538117967314, 5.999999999999999112 ) ) ;
#27425 = CARTESIAN_POINT ( 'NONE',  ( -33.37872103062156981, 201.4690446883607819, 2.162041339862843525 ) ) ;
#27426 = CYLINDRICAL_SURFACE ( 'NONE', #31055, 24.80000000000000426 ) ;
#27427 = CARTESIAN_POINT ( 'NONE',  ( 8.715434833791931624, 73.66018628210144925, 8.962234695871760692 ) ) ;
#27428 = CARTESIAN_POINT ( 'NONE',  ( -13.50000000000000533, 199.4750000000000227, -23.38268590217984411 ) ) ;
#27429 = DIRECTION ( 'NONE',  ( 0.000000000000000000, 0.000000000000000000, 1.000000000000000000 ) ) ;
#27431 = ORIENTED_EDGE ( 'NONE', *, *, #26389, .F. ) ;
#27430 = CARTESIAN_POINT ( 'NONE',  ( -1.715153634034234598, 51.52268628210144641, -9.534712964251941258 ) ) ;
#27432 = CARTESIAN_POINT ( 'NONE',  ( 2.999999999999997335, 244.5000000000000000, 5.000000000000000000 ) ) ;
#27433 = ORIENTED_EDGE ( 'NONE', *, *, #11457, .T. ) ;
#27434 = CARTESIAN_POINT ( 'NONE',  ( 26.99999999999999645, 3.464101615137755275, -1.537500000000004086 ) ) ;
#27435 =( GEOMETRIC_REPRESENTATION_CONTEXT ( 3 ) GLOBAL_UNCERTAINTY_ASSIGNED_CONTEXT ( ( #1362 ) ) GLOBAL_UNIT_ASSIGNED_CONTEXT ( ( #30394, #33235, #19035 ) ) REPRESENTATION_CONTEXT ( 'NONE', 'WORKASPACE' ) );
#27436 = CARTESIAN_POINT ( 'NONE',  ( -60.88913769728823411, 206.8500491399821044, -5.686928522499717253 ) ) ;
#27437 = CARTESIAN_POINT ( 'NONE',  ( 37.01747826964035681, 3.604726614523243278, 161.4436866585844541 ) ) ;
#27438 = CARTESIAN_POINT ( 'NONE',  ( 36.71355410024750654, 3.464101615137759271, 160.7644657540882918 ) ) ;
#27439 = CARTESIAN_POINT ( 'NONE',  ( 18.00000000000000355, 246.0250000000000057, 5.196152422706632912 ) ) ;
#27440 = CARTESIAN_POINT ( 'NONE',  ( 22.56230152254410370, 7.347880794884117764E-16, -4.162499998770996967 ) ) ;
#27441 = EDGE_CURVE ( 'NONE', #37335, #32501, #314, .T. ) ;
#27442 = CARTESIAN_POINT ( 'NONE',  ( 4.622313124798831829, 82.96481371789856496, -11.61527771782809282 ) ) ;
#27443 = CARTESIAN_POINT ( 'NONE',  ( -2.311890736173176641, 97.52268628210144641, -12.53471296425194659 ) ) ;
#27444 = VERTEX_POINT ( 'NONE', #18998 ) ;
#27445 = ORIENTED_EDGE ( 'NONE', *, *, #28150, .T. ) ;
#27446 = CARTESIAN_POINT ( 'NONE',  ( 27.00000000000000355, 199.4375000012290400, -3.306546357697854128E-15 ) ) ;
#27447 = DIRECTION ( 'NONE',  ( 0.08715574274765150453, 0.000000000000000000, 0.9961946980917461003 ) ) ;
#27448 = EDGE_CURVE ( 'NONE', #8594, #36641, #30920, .T. ) ;
#27449 = CARTESIAN_POINT ( 'NONE',  ( -3.257655550456946880, 63.70231371789854791, -15.46528703574811736 ) ) ;
#27450 = CARTESIAN_POINT ( 'NONE',  ( 15.24356964374999990, 3.323476615752268604, -6.590624999385473970 ) ) ;
#27451 = EDGE_CURVE ( 'NONE', #13180, #22009, #30652, .T. ) ;
#27452 = CARTESIAN_POINT ( 'NONE',  ( 18.12178482187499640, 246.1843750006145228, -4.985214923628404904 ) ) ;
#27453 =( BOUNDED_SURFACE ( )  B_SPLINE_SURFACE ( 3, 2, ( 
 ( #26330, #9284, #3593, #11747, #366, #181, #9471, #35048, #9096, #20858, #20665, #13023, #32211, #6437, #18010, #34864, #6249, #15157, #8904, #17827, #26706, #737, #7338, #35421, #24579, #12308, #36131, #23882, #21046, #32584, #18200, #6624, #10172, #33298, #18911, #31381, #2191, #4663, #24942, #24760, #13210, #13955, #37057, #36310, #16059, #16801, #34037, #16246, #13772, #5037, #25134, #19469, #4851, #21932, #31015, #22118, #10914, #27607, #36689, #5224, #1822, #10727, #30828, #1639, #10359, #19289, #33479, #27795, #7522, #13391, #34222, #25319, #25504, #19095, #11104, #36499, #30647, #36869, #8081, #16430, #16617, #22490, #33666, #10542, #19656, #7707, #27977, #2007, #13581, #22678, #8266, #22302, #33854, #28344, #31198, #7895, #2380, #28160, #19839, #8816, #31748, #11291, #20390, #11472, #274, #5401, #14502, #5777, #14321, #20759, #458, #11650, #34775, #14687, #17725, #2748, #16981, #17356, #25875, #23042, #28898, #34588, #2933, #26058, #86, #20198, #23226, #31931, #5963, #17542, #17171, #29077, #3120, #37423, #9191, #32114, #26236, #22860, #9002, #8630, #11838, #23408, #28524, #2566, #6150, #14136, #29266, #25692, #34957, #28713, #20572, #3306, #8447, #37241, #14877, #34409, #26424, #12027, #20016, #23596, #31561, #35138, #5585, #32866, #6914, #36078, #18485, #29647, #3684, #15817, #21139, #9564, #15064, #32677, #15628, #21514, #32485, #18292, #35702, #17915, #23785, #10122, #27181, #15252, #35324, #29834, #643, #26804, #6344, #6719, #835, #12403, #3870, #23975, #15443, #26992, #1020, #12593, #24158, #21327, #9752, #30025, #6532, #4057, #1206, #35519, #32303, #33059, #12778, #12213, #35890, #24348, #9933, #7105, #29459, #3493, #18674, #26614, #30216, #9378, #4242, #18106, #27367, #1397, #20952, #12972, #24529, #13155, #19417, #28111, #27558, #22438, #16010, #33618, #31151, #22255, #33806, #25454, #7844, #19047, #30599, #5170, #10488, #36447, #4429, #22067, #4983, #10864, #21876, #7658, #25082, #7284, #24710, #37007, #16566, #4614, #36262, #19235, #1585, #33985, #7469, #30778, #4801, #18858, #10306, #24897, #33245, #33428, #16194, #27744, #2334, #30966, #19602, #21694, #16748, #1773, #13340, #2142, #13722, #16379, #10676, #25271, #27925, #30406, #36823, #1956, #13526, #36637, #8028, #28296, #13905, #31329, #11050, #11793, #29028, #11236, #34725, #39, #20151, #14454, #37373, #16935, #26010, #17123, #5914, #22625, #31698, #11425, #19970, #26379, #6098, #17307, #2882, #20342, #23361, #8769, #34912, #34173, #8217, #34542, #31513, #34357, #11604, #8402, #14274, #8581, #19792, #28848, #5725, #23179, #31884, #17493, #3072, #29219, #37193, #5357, #14642, #26192, #229, #5537, #8957, #14087, #25825, #20528, #28477, #32070, #28660, #2518, #25638, #17682, #3261, #14834, #22808, #2698, #22992, #6867, #9712, #35096, #29415, #33015, #3825, #9145, #15588, #7065, #18442, #23931, #32822, #15403, #978, #20712, #32636, #789, #12166, #12554, #21287, #11979, #23740, #6297, #15017, #26568, #18635, #35473, #9524, #29983, #1168, #597, #27141, #3640, #35278, #30175, #4015, #29604, #17870, #32255, #9336, #20905, #413, #9892, #12740, #21476, #24308, #35851, #15210, #4203, #15780, #23552, #21096, #3447, #32445, #12360, #26759, #6489, #18061, #6676, #18249, #29793, #26948, #24120, #35663, #10084, #31111, #1545, #25232, #1732, #10450, #4388, #4941, #27330, #4579, #22027, #30365, #22398, #22215, #36781, #15968, #33580, #19003, #7618, #13300, #24859, #21653, #10636, #16155, #24671, #27520, #1360, #10826, #16523, #33947, #30925, #13684, #30561, #19560, #28071, #5131, #36407, #12931, #7988, #19194, #27704, #13117, #2105, #24493, #33207, #33393, #36040, #18821, #36223, #7247, #10266, #21841, #7433, #30742, #4763, #16337, #27885, #1916, #13484, #25040, #36596, #33766 ),
 ( #7806, #19382, #37154, #2476, #17266, #14049, #19933, #2656, #13866, #34502, #11383, #25783, #14233, #5684, #23140, #34871, #5320, #25415, #20300, #37333, #22956, #25598, #37500, #19753, #31473, #8543, #36968, #20109, #11195, #11011, #16712, #17452, #34682, #31842, #8727, #5874, #28990, #3031, #25970, #22584, #8179, #11753, #31657, #34129, #14603, #23321, #26154, #28806, #11567, #2843, #14415, #31292, #187, #17080, #28435, #8912, #20487, #5497, #32025, #28259, #16896, #2291, #22769, #34317, #8363, #28619, #32592, #15164, #9478, #32404, #11938, #21054, #12122, #936, #6056, #23507, #9665, #23696, #12315, #26713, #9849, #29176, #32781, #21426, #6816, #17643, #20865, #29368, #744, #6444, #9101, #3218, #21242, #35054, #3779, #12510, #20670, #18392, #372, #18017, #15543, #6631, #18206, #14790, #29747, #3407, #14976, #27101, #29562, #3599, #26336, #23889, #26908, #29942, #6256, #35430, #15353, #32217, #17833, #26525, #24074, #555, #35240, #35619, #9291, #3969, #1125, #12690, #24263, #35806, #27282, #36177, #7020, #7207, #1312, #33161, #13638, #4716, #30877, #10781, #4900, #30319, #10031, #30697, #24994, #10223, #21986, #16294, #1498, #32968, #19148, #21611, #7758, #18958, #21797, #25188, #16482, #15732, #18588, #33718, #13444, #18779, #27842, #33531, #4533, #36363, #33350, #12880, #10411, #13073, #1873, #30130, #16109, #7386, #4343, #4162, #28028, #1685, #24812, #36551, #19339, #15923, #24447, #30513, #27473, #24629, #27660, #13260, #7573, #10592, #22172, #2061, #36741, #35995, #28575, #25742, #34087, #37294, #11156, #19709, #26111, #11525, #31614, #31433, #22729, #31248, #143, #17411, #2614, #14190, #5641, #34638, #5277, #33904, #34276, #16856, #2431, #8319, #14003, #19891, #5455, #17037, #37108, #11342, #22914, #34460, #8503, #8138, #20069, #17225, #28393, #22354, #23094, #28763, #28215, #25930, #25555, #2802, #14374, #7945, #19521, #8683, #31067, #20255, #5090, #37474, #31795, #5833, #28952, #25371, #16669, #2989, #13824, #14559, #2245, #36919, #10966, #22540, #23653, #21197, #12271, #23843, #15499, #35383, #9059, #20630, #32736, #512, #26480, #31987, #12079, #32544, #891, #11894, #35196, #15118, #34825, #3173, #27054, #6586, #32173, #14747, #9245, #17600, #12462, #35016, #20818, #32360, #8868, #6016, #14933, #23282, #23462, #29133, #6210, #29895, #21010, #9620, #11707, #6772, #17782, #26293, #9432, #3736, #6399, #699, #18161, #29325, #20445, #29702, #329, #24031, #17972, #29515, #3925, #18347, #3363, #3556, #35576, #15309, #26669, #26861, #27615, #10178, #4490, #27423, #6975, #16067, #7160, #33486, #1080, #18544, #1830, #32923, #13029, #10552, #1646, #13218, #4859, #24768, #35950, #9989, #22127, #1456, #15879, #21383, #24585, #21941, #27803, #1264, #36137, #36319, #24215, #30084, #16438, #7531, #21570, #4117, #21754, #15690, #13400, #24402, #33305, #7345, #35760, #27241, #4300, #12650, #12835, #33115, #18733, #19296, #10366, #36507, #9805, #33674, #30275, #18918, #19104, #30655, #30469, #4670, #16253, #24949, #7714, #30835, #16627, #3267, #13961, #16809, #9150, #11985, #10736, #27985, #29225, #8961, #28169, #14144, #16990, #37063, #31388, #28350, #33861, #5408, #34044, #23367, #2015, #11110, #2387, #36876, #6305, #23557, #34230, #19846, #37249, #14839, #25327, #13592, #25510, #10922, #8090, #22686, #19664, #8273, #28530, #2573, #5233, #25697, #11798, #34917, #20533, #2199, #32075, #6104, #22497, #32261, #17687, #26385, #7903, #419, #31205, #35101, #20717, #25142, #36696, #22309, #19477, #31023, #5045, #13779, #3646, #984, #6683, #20912, #33213, #33022, #9342, #15594, #24314, #15216, #6495, #17876, #27335, #7073, #1366, #21482, #4209, #21104, #10090, #18641, #29421, #15410, #3455, #36046, #29799, #18255, #32451, #30183, #15024, #12172, #23937 ),
 ( #18069, #12937, #12746, #15787, #29611, #12560, #9529, #24126, #3832, #26954, #23746, #1173, #32642, #4022, #24500, #26574, #603, #35669, #797, #26765, #18449, #12367, #9718, #21293, #35284, #32829, #6874, #29991, #27150, #35857, #9898, #21660, #35480, #4394, #25048, #36413, #10456, #10272, #16343, #13123, #4585, #24865, #15975, #33585, #7438, #30372, #7253, #33772, #36601, #10642, #13490, #22219, #7812, #19388, #27892, #27526, #24677, #4948, #7624, #1551, #30931, #16530, #28077, #22034, #18827, #36231, #21847, #30567, #33399, #1922, #19200, #19010, #16161, #27710, #4770, #1739, #30747, #13306, #21785, #1113, #27088, #21601, #4331, #29732, #18765, #6803, #3766, #33337, #35984, #32768, #9464, #23875, #3957, #12494, #18948, #36166, #9836, #32955, #12868, #15911, #924, #15148, #15531, #24060, #21227, #12679, #18378, #29929, #24249, #35793, #21413, #7008, #30119, #18577, #4150, #15341, #15721, #27271, #35607, #7376, #30307, #24435, #21039, #7195, #1298, #10020, #33150, #3586, #26698, #27459, #729, #1488, #12300, #13061, #26894, #24618, #10212, #6617, #35413, #32576, #18192, #9651, #36907, #36351, #31236, #24800, #4890, #2420, #31056, #5077, #34264, #16657, #27831, #1861, #13993, #19328, #7745, #13251, #30867, #13813, #19696, #30686, #16470, #33892, #16097, #21974, #8308, #25360, #13430, #33519, #28015, #10398, #5266, #16284, #2047, #13626, #27649, #7562, #33705, #4522, #4704, #19137, #24979, #11143, #2233, #28383, #30501, #25544, #36539, #10582, #28204, #22528, #25177, #19509, #10955, #22161, #1676, #34075, #36729, #16844, #10768, #22341, #22720, #37096, #7934, #8125, #20301, #29353, #6428, #171, #358, #23679, #11738, #34667, #726, #3393, #23308, #14399, #28790, #5859, #17628, #32011, #35040, #14962, #26696, #8712, #17249, #12106, #29158, #3201, #31824, #26509, #11550, #34854, #14777, #2827, #11922, #3016, #25956, #8529, #9275, #540, #35226, #20847, #32388, #18002, #29545, #17814, #5669, #37498, #3583, #23489, #23123, #15146, #12298, #23872, #6042, #20095, #9087, #20656, #20284, #26321, #8894, #17437, #32203, #31641, #28975, #14585, #26138, #20472, #6238, #16094, #32952, #18762, #33333, #27084, #27269, #13059, #1110, #24058, #27647, #30305, #12677, #3764, #18189, #32765, #35603, #35411, #7374, #24616, #18945, #1485, #21783, #24247, #1674, #36163, #13248, #7005, #9461, #21037, #9833, #35791, #12491, #10209, #32574, #29730, #3954, #6614, #26891, #21225, #15338, #922, #9649, #30499, #21411, #18575, #6801, #4520, #18376, #30117, #4146, #29925, #15529, #4329, #15719, #1295, #12866, #24432, #35982, #10018, #21599, #33148, #15909, #7192, #27457, #37093, #36349, #21971, #10766, #7742, #10579, #25358, #22159, #28012, #22338, #33516, #5075, #19507, #8123, #13990, #24976, #33890, #28201, #10393, #16281, #2601, #19694, #33703, #27829, #7932, #30683, #25541, #19326, #31053, #2045, #7560, #19135, #13624, #4702, #36537, #1859, #30863, #5439, #34072, #22718, #24798, #34261, #4888, #13428, #22526, #16841, #25174, #13811, #31234, #16468, #36727, #10952, #16655, #11141, #2230, #36903, #17021, #8305, #5264, #28381, #19877, #31419, #2417, #28560, #17207, #23265, #17582, #2972, #20055, #29115, #20237, #9041, #14173, #34809, #14542, #23078, #29498, #9226, #20428, #6002, #23445, #26463, #11509, #25727, #26097, #34624, #31780, #127, #5815, #11692, #8854, #31972, #28937, #3159, #14729, #26278, #310, #25914, #11876, #34998, #8668, #17955, #3346, #20613, #31600, #17765, #17397, #32153, #6193, #37280, #11327, #14914, #22897, #497, #34445, #29306, #37459, #12063, #23637, #28746, #8484, #35180, #5623, #20800, #32342, #2786, #6380, #14360, #15481, #13013, #4100, #15671, #7325, #27222, #874, #12446, #24567, #29876, #18331, #23823, #3909, #9973, #12817, #683, #32527, #36121 ),
 ( #15860, #27036, #1059, #21736, #10161, #35365, #3537, #4283, #27405, #6757, #9416, #6570, #12633, #6959, #24198, #20992, #18527, #9604, #35931, #15102, #35743, #9789, #24014, #18900, #33287, #21366, #32905, #24386, #1437, #35560, #26652, #30065, #21178, #32717, #1247, #21553, #33100, #7143, #18717, #30256, #12253, #18144, #29686, #3720, #15292, #26844, #19277, #27786, #34212, #19647, #2180, #36300, #34026, #10532, #36680, #1997, #8257, #16049, #31189, #30452, #5212, #4470, #7697, #16235, #13570, #30817, #33469, #27596, #8071, #21919, #28149, #36860, #10347, #16789, #24751, #4841, #2371, #31007, #5027, #1627, #16607, #1813, #13381, #13945, #16420, #27967, #13199, #25123, #13762, #28334, #30636, #10718, #33845, #7511, #19085, #4653, #25308, #24934, #36488, #22292, #22108, #25494, #33657, #7884, #19458, #10905, #22479, #37046, #11094, #22668, #23217, #16972, #34947, #26414, #265, #5766, #14677, #34766, #20380, #2557, #14492, #20189, #31552, #31922, #20563, #32105, #5576, #6139, #34399, #8437, #449, #17346, #3111, #17716, #11463, #11641, #8993, #23032, #20006, #12016, #26227, #34579, #25682, #14126, #17162, #28702, #19830, #29255, #3296, #14868, #23399, #23587, #8620, #35129, #31369, #5392, #28889, #28514, #37232, #31738, #2923, #2739, #11280, #22850, #14311, #25864, #37413, #26049, #76, #8808, #5953, #17532, #29066, #11828, #29825, #23776, #24340, #9180, #23966, #3861, #12204, #4233, #4047, #7097, #35314, #15435, #827, #26984, #21130, #6710, #3485, #30017, #35509, #32854, #21506, #20749, #6334, #32668, #29638, #32477, #9745, #6524, #12394, #18281, #17906, #1010, #12584, #24150, #35693, #21317, #15619, #27359, #9369, #29450, #12770, #6904, #18476, #18098, #27173, #20944, #9555, #1197, #15055, #35880, #3674, #26604, #32294, #9922, #33050, #18665, #30206, #15809, #1389, #12962, #24520, #634, #15244, #26795, #8018, #2134, #22428, #1765, #28793, #13713, #14402, #33610, #36070, #17254, #10478, #24889, #13147, #25262, #10114, #30397, #4605, #21685, #27548, #21868, #18850, #2830, #10296, #33977, #22057, #19226, #24701, #36813, #33237, #13331, #30769, #1575, #31645, #30957, #19593, #36253, #4792, #27734, #16370, #7649, #27915, #4420, #19407, #36439, #22246, #10855, #7276, #16001, #1945, #19038, #33421, #36627, #7459, #13516, #25073, #30590, #10667, #33796, #7833, #4975, #16556, #28102, #16184, #5673, #34670, #29549, #9090, #20659, #11742, #9279, #28979, #29162, #32206, #8716, #29356, #20475, #20287, #25959, #26700, #6431, #3588, #32391, #18005, #15150, #731, #35229, #23126, #17440, #21041, #3396, #31828, #12302, #32578, #23877, #11926, #20851, #14965, #26513, #5862, #6242, #26325, #174, #543, #35415, #9466, #23311, #6619, #3019, #14590, #18194, #23494, #29734, #3768, #17631, #17820, #32920, #3205, #26142, #11554, #34857, #14781, #8898, #32014, #6045, #361, #35043, #12109, #23683, #21603, #27273, #12870, #9653, #36168, #30121, #1489, #27651, #26896, #12496, #1300, #35795, #1115, #15913, #12681, #18579, #24437, #24062, #33152, #10022, #35986, #7197, #4333, #21787, #33521, #3959, #35609, #18950, #18767, #30309, #24251, #10214, #18380, #4152, #27461, #21229, #13063, #9838, #32770, #15342, #16099, #33339, #30503, #7378, #4524, #1678, #13253, #24620, #6805, #29931, #10400, #24802, #15533, #36353, #21976, #7564, #19139, #30688, #926, #27090, #21415, #32957, #15723, #7010, #16846, #5444, #17026, #28017, #28566, #19330, #30869, #22902, #2235, #25546, #2605, #33894, #34077, #19882, #7936, #4892, #34450, #37098, #19511, #10584, #24981, #2049, #16472, #4706, #14177, #31424, #25733, #8310, #37284, #31058, #8491, #11332, #20060, #13815, #16286, #27833, #16659, #5080, #13628, #1863, #13432, #36541, #10770, #22163, #33707, #25179, #7747, #36731, #22343, #28206, #25362 ),
 ( #36909, #10957, #22530, #8127, #19698, #31238, #5268, #28385, #2422, #13995, #11146, #22722, #34266, #12260, #3353, #29504, #9423, #3545, #28942, #8673, #29313, #23644, #8859, #20619, #14921, #133, #31604, #17771, #20244, #6387, #17589, #20435, #23830, #15108, #14364, #5630, #32349, #17962, #34816, #25919, #34629, #3164, #35004, #31978, #37464, #9047, #11697, #26470, #17213, #14736, #6007, #2978, #28753, #26659, #318, #23451, #503, #689, #14548, #2791, #29121, #26102, #23271, #26285, #11883, #32159, #6198, #12069, #35187, #9232, #20807, #35371, #11514, #5821, #23084, #31786, #17402, #24756, #10168, #30264, #26851, #24575, #1068, #27229, #30071, #36306, #6575, #21743, #20998, #33292, #32535, #35749, #6762, #4106, #9794, #24020, #18151, #36126, #12451, #18723, #27411, #880, #7333, #15298, #32911, #30459, #21560, #33105, #29692, #7150, #18336, #29884, #4476, #21372, #6965, #3725, #18533, #4290, #18906, #21185, #15678, #24391, #35565, #9611, #32725, #15868, #16055, #3915, #27603, #15488, #1254, #27042, #12823, #35938, #12639, #24204, #1634, #9979, #1443, #13019, #13206, #11100, #4658, #22298, #19836, #10910, #22487, #14132, #34033, #7702, #19285, #31377, #36685, #25129, #30642, #10723, #31194, #37052, #10537, #33850, #13767, #33474, #1818, #25688, #5219, #30824, #13387, #7891, #16242, #22673, #33662, #19465, #31012, #7518, #27791, #13576, #21927, #22114, #24939, #4847, #28520, #19652, #8263, #10354, #5397, #16426, #36494, #8077, #2376, #5033, #36865, #16795, #27972, #19090, #28341, #2003, #34218, #16613, #28155, #2562, #16977, #2186, #25314, #13951, #25500, #2929, #31557, #2743, #8812, #3116, #26054, #5581, #14683, #5772, #32110, #37237, #20386, #82, #8626, #15061, #32300, #5959, #29072, #8998, #12023, #34584, #11287, #11646, #20194, #17352, #23222, #28894, #34771, #31927, #17538, #14497, #26232, #270, #11833, #23404, #11468, #34953, #20568, #31744, #3490, #26420, #6144, #17167, #3302, #17721, #29262, #14872, #22855, #34405, #454, #23592, #23038, #35134, #9186, #20754, #6340, #17910, #14317, #25870, #29455, #8443, #20011, #28708, #37418, #18482, #4238, #29830, #15249, #18855, #21511, #18288, #32482, #9375, #23972, #26800, #26611, #36075, #15814, #10119, #30213, #12968, #3867, #30403, #27364, #4425, #24155, #640, #7281, #1016, #15440, #3681, #1394, #12209, #20949, #32673, #23782, #18103, #12399, #6529, #35320, #832, #24526, #12589, #9750, #35515, #21691, #29643, #26988, #21323, #9560, #33241, #33055, #21136, #6716, #32863, #35698, #6910, #30022, #4052, #15625, #9930, #27178, #12775, #1202, #24345, #35886, #7102, #18671, #1770, #16562, #13336, #19231, #1951, #13152, #33803, #10672, #25078, #13521, #4980, #22434, #34169, #4610, #24707, #19598, #36633, #22251, #24895, #36819, #19044, #30774, #7840, #36259, #19412, #10484, #10302, #16007, #16745, #33981, #31148, #8024, #5167, #28292, #2331, #25267, #21873, #7465, #11046, #30962, #33425, #13902, #22622, #25450, #28108, #10861, #2139, #13719, #30595, #37003, #8214, #4797, #16191, #27741, #19789, #31326, #16375, #36444, #27554, #22064, #1582, #33615, #7654, #27920, #14271, #20708, #409, #11601, #34720, #14637, #17678, #2695, #16932, #5722, #25822, #22989, #28844, #34539, #31693, #2878, #36, #20147, #23175, #31881, #8765, #20339, #17119, #5911, #17303, #37369, #9142, #32067, #26188, #11233, #8953, #8578, #17490, #14451, #5354, #28474, #6095, #2513, #29215, #14084, #26007, #28657, #29025, #3069, #8399, #25634, #20525, #34354, #225, #11789, #22805, #3256, #37190, #23357, #14831, #34909, #26375, #19967, #11974, #11422, #23547, #35093, #31509, #5532, #15012, #32632, #15583, #21470, #32441, #18244, #35659, #17867, #23735, #10079, #27137, #29599, #35274, #29788, #592, #33011, #18056, #3819, #9520, #29412 ),
 ( #24303, #21092, #21282, #4009, #785, #32251, #18437, #20900, #7060, #15396, #6670, #12925, #15776, #26564, #6291, #3443, #12162, #35468, #9329, #6485, #3636, #15205, #24488, #1164, #30171, #26754, #4199, #12354, #23927, #29979, #35846, #26944, #32818, #12736, #973, #12550, #9888, #24116, #18631, #9706, #6862, #36035, #27325, #1353, #21649, #22395, #33944, #24857, #15963, #24667, #30739, #25037, #10449, #27516, #36594, #27700, #16521, #33203, #4760, #22025, #30557, #36964, #16710, #27883, #13482, #30923, #7986, #19000, #7243, #33578, #4575, #1730, #7615, #13298, #19190, #16335, #1913, #36405, #10634, #22212, #33762, #7803, #33390, #19379, #4938, #16151, #25411, #10823, #28069, #1541, #25229, #2103, #13682, #36779, #18817, #30361, #19558, #4385, #31110, #13111, #5129, #7430, #28257, #2287, #36218, #10262, #13863, #21838, #8723, #17448, #16893, #11749, #5317, #22952, #20483, #11563, #23136, #14787, #34678, #8360, #19931, #32021, #37329, #25779, #31289, #11379, #31836, #183, #11191, #34497, #14411, #34126, #2472, #26332, #5869, #31469, #14045, #8539, #28432, #23317, #34314, #20105, #31653, #11007, #29171, #5680, #17261, #25594, #14599, #22581, #37150, #17075, #8176, #22766, #5493, #28614, #19751, #2651, #8906, #28802, #2838, #14228, #26150, #25966, #6932, #20295, #28986, #6052, #3027, #17639, #34866, #3215, #29556, #6626, #12310, #35423, #32213, #21237, #15159, #24069, #13211, #11932, #35050, #23884, #20860, #23691, #931, #35236, #3595, #9473, #9098, #18202, #32587, #21048, #29742, #26903, #6812, #19097, #26521, #20667, #4482, #3775, #15349, #9286, #32776, #3404, #26708, #12505, #6251, #35615, #32399, #17829, #368, #1640, #18387, #16060, #29937, #27608, #24761, #36311, #9660, #29364, #14972, #33480, #10360, #551, #21933, #7523, #30648, #4664, #16247, #23503, #12117, #6439, #18012, #739, #2008, #2382, #28525, #2567, #13582, #14137, #4852, #16431, #8448, #25321, #11105, #25693, #19470, #19657, #5402, #31016, #27978, #20017, #22679, #5038, #33668, #10543, #25135, #36690, #27796, #37242, #16983, #11292, #31382, #22861, #16618, #31563, #34410, #5586, #36870, #10729, #31199, #28161, #22303, #1823, #13392, #37058, #7708, #24943, #7896, #34038, #10915, #36500, #22119, #19290, #30829, #33855, #2192, #13773, #22491, #8082, #5225, #16802, #28345, #13956, #25505, #34223, #8267, #19840, #3121, #87, #2934, #17726, #14503, #20391, #14688, #14322, #34958, #11839, #26237, #275, #6151, #23597, #35325, #5778, #25876, #20760, #23409, #9003, #26059, #459, #20199, #31932, #20573, #37424, #32115, #11651, #11473, #17172, #17916, #35139, #32304, #9192, #6345, #29460, #3494, #26425, #23043, #8632, #12214, #29267, #34589, #15066, #23786, #26615, #3307, #12028, #14878, #644, #31749, #9379, #17543, #28899, #20953, #32486, #28714, #23227, #2749, #17357, #34776, #8817, #5964, #29078, #4430, #35703, #35892, #21695, #9753, #32678, #36263, #1398, #21329, #12404, #26805, #3871, #6721, #6533, #16011, #33246, #27560, #10123, #30407, #32867, #10307, #7285, #21877, #4058, #18107, #24711, #18486, #6915, #21140, #18859, #29649, #836, #12594, #3685, #35520, #12974, #15818, #15253, #9565, #1586, #9934, #23976, #13156, #18293, #24530, #30026, #36079, #21515, #7106, #29835, #1207, #15629, #15444, #18675, #26993, #1021, #24159, #27182, #12779, #24349, #33060, #30217, #27368, #4243, #16380, #4984, #31152, #1957, #36448, #22627, #22439, #27926, #27745, #4616, #33619, #10489, #33429, #25456, #16749, #37008, #5171, #2335, #13527, #34174, #28297, #7470, #33808, #19048, #8218, #7845, #10677, #22068, #13906, #30600, #7659, #25083, #16195, #19237, #36638, #30779, #1774, #22256, #13341, #28112, #25272, #19418, #24898, #4802, #11051, #30967, #33986, #16567, #2143, #13723, #36824, #10866, #8029 ),
 ( #19604, #30349, #33565, #15952, #27127, #1152, #13285, #18618, #7050, #12539, #30160, #13099, #18987, #29968, #15763, #33190, #15383, #21270, #7602, #24654, #12723, #32808, #27312, #35648, #30544, #15571, #1342, #4189, #26933, #24103, #32998, #3807, #36205, #1526, #4561, #10063, #963, #9694, #12913, #24292, #35836, #4373, #9877, #24477, #36023, #6848, #21638, #7233, #18807, #27505, #10249, #21825, #10438, #18424, #3997, #33377, #7416, #16136, #21458, #27688, #1715, #24841, #36392, #22011, #29777, #13667, #27870, #19177, #19919, #37136, #34303, #25583, #11181, #22754, #8347, #28419, #16322, #10622, #14217, #22567, #1902, #31458, #25767, #5481, #5118, #14033, #34114, #19739, #13472, #13852, #19548, #30908, #31277, #17065, #28603, #4928, #2640, #33749, #7789, #37319, #16697, #2459, #11369, #10811, #10996, #22941, #22383, #19367, #34487, #30726, #33933, #25024, #36581, #16510, #28057, #4749, #22201, #2092, #25217, #36768, #7974, #31096, #28245, #2275, #25399, #36949, #8165, #5305, #16883, #20791, #22751, #18137, #17946, #674, #29491, #15095, #22937, #26645, #490, #8526, #15474, #866, #20985, #17061, #15283, #29299, #3529, #32335, #27028, #34300, #12437, #11177, #24006, #8343, #26456, #34483, #6373, #12056, #14214, #19914, #35358, #37316, #35552, #35172, #23629, #29868, #32710, #31455, #5478, #9597, #21170, #14906, #28599, #25764, #12245, #23816, #9220, #2635, #9409, #17758, #6562, #11366, #32518, #29679, #20092, #31638, #6750, #3713, #26837, #18324, #3902, #6185, #3337, #1429, #21546, #18709, #24562, #30249, #16412, #10154, #12626, #7503, #7318, #27590, #18892, #4463, #12810, #16041, #27398, #35924, #4832, #27776, #10341, #6950, #4646, #4276, #30442, #21729, #1052, #24190, #1806, #35736, #13373, #9782, #15851, #24379, #33279, #13006, #4092, #21358, #1619, #32898, #13189, #18519, #30058, #24928, #15664, #36112, #10523, #24744, #36293, #27215, #21912, #9966, #33092, #22101, #33461, #19078, #1239, #30630, #16226, #36481, #7137, #33650, #7689, #19270, #30810, #5760, #11275, #25302, #31001, #25487, #33840, #17155, #13756, #37038, #5206, #13562, #22286, #31183, #1990, #2174, #7877, #28144, #8613, #37227, #25858, #27959, #37406, #36854, #5021, #25673, #20001, #16782, #16966, #22844, #34018, #25115, #22661, #28327, #10898, #2552, #28694, #2731, #22470, #14306, #16601, #8063, #20183, #11085, #34390, #11456, #19640, #19825, #5570, #2365, #13938, #31732, #8432, #34207, #19451, #10710, #8251, #31362, #36673, #23025, #34573, #5386, #31545, #28509, #14119, #9550, #20938, #32663, #14863, #17339, #35503, #29250, #3291, #2917, #35125, #15238, #11636, #23394, #28882, #8802, #3103, #70, #21124, #29060, #26788, #26410, #444, #31916, #32472, #14487, #32101, #12009, #20373, #12390, #12196, #820, #5946, #23581, #8985, #9175, #20743, #32285, #23210, #628, #26597, #18092, #6329, #26043, #34759, #17900, #258, #14672, #29445, #26222, #20557, #3480, #17526, #15049, #23769, #35309, #9363, #6517, #29632, #11823, #34940, #6132, #3668, #23959, #17709, #30012, #27543, #9741, #9918, #27354, #26978, #10108, #1191, #15430, #6704, #7455, #24695, #21863, #13140, #36248, #10291, #33416, #15996, #3853, #35688, #1758, #21679, #1005, #19030, #13325, #30585, #30200, #1570, #33232, #7270, #12579, #18276, #21501, #1384, #21312, #24884, #4601, #16180, #32848, #12956, #35875, #24516, #18661, #4227, #24146, #27729, #36431, #10474, #36065, #6895, #18470, #15804, #27168, #4042, #18846, #15613, #33044, #30391, #12766, #4413, #22051, #29818, #24334, #7092, #2498, #14258, #22242, #4788, #37179, #16734, #28281, #19405, #16921, #36620, #36807, #2320, #16361, #36992, #28095, #27911, #33604, #34341, #14072, #11220, #25621, #22792, #8386, #19956, #5343, #30765, #25066, #28645, #11035, #1940, #31498, #2682 ) ),
 .UNSPECIFIED., .T., .F., .F. ) 
 B_SPLINE_SURFACE_WITH_KNOTS ( ( 4, 3, 4 ),
 ( 3, 2, 2, 2, 2, 2, 2, 2, 2, 2, 2, 2, 2, 2, 2, 2, 2, 2, 2, 2, 2, 2, 2, 2, 2, 2, 2, 2, 2, 2, 2, 2, 2, 2, 2, 2, 2, 2, 2, 2, 2, 2, 2, 2, 2, 2, 2, 2, 2, 2, 2, 2, 2, 2, 2, 2, 2, 2, 2, 2, 2, 2, 2, 2, 2, 2, 2, 2, 2, 2, 2, 2, 2, 2, 2, 2, 2, 2, 2, 2, 2, 2, 2, 2, 2, 2, 2, 2, 2, 2, 2, 2, 2, 2, 2, 2, 2, 2, 2, 2, 2, 2, 2, 2, 2, 2, 2, 2, 2, 2, 2, 2, 2, 2, 2, 2, 2, 2, 2, 2, 2, 2, 2, 2, 2, 2, 2, 2, 2, 2, 2, 2, 2, 2, 2, 2, 2, 2, 2, 2, 2, 2, 2, 2, 2, 2, 2, 2, 2, 2, 2, 2, 2, 2, 2, 2, 2, 2, 2, 2, 2, 2, 2, 2, 2, 2, 2, 2, 2, 2, 2, 2, 2, 2, 2, 2, 2, 2, 2, 2, 2, 2, 2, 2, 2, 2, 2, 2, 2, 2, 2, 2, 2, 2, 2, 2, 2, 2, 2, 2, 2, 2, 2, 2, 2, 2, 2, 2, 2, 2, 2, 2, 2, 2, 2, 2, 2, 2, 2, 2, 2, 2, 2, 2, 2, 2, 2, 2, 2, 2, 2, 2, 2, 2, 2, 2, 2, 2, 2, 2, 3 ),
 ( 0.000000000000000000, 0.5000000000000000000, 1.000000000000000000 ),
 ( 0.000000000000000000, 0.004166666666666666609, 0.008333333333333333218, 0.01250000000000000069, 0.01666666666666666644, 0.02083333333333333218, 0.02500000000000000139, 0.02916666666666666713, 0.03333333333333333287, 0.03749999999999999861, 0.04166666666666666435, 0.04583333333333333010, 0.05000000000000000278, 0.05416666666666666852, 0.05833333333333333426, 0.06250000000000000000, 0.06666666666666666574, 0.07083333333333333148, 0.07499999999999999722, 0.07916666666666666297, 0.08333333333333332871, 0.08749999999999999445, 0.09166666666666666019, 0.09583333333333333981, 0.1000000000000000056, 0.1041666666666666713, 0.1083333333333333370, 0.1125000000000000028, 0.1166666666666666685, 0.1208333333333333343, 0.1250000000000000000, 0.1291666666666666796, 0.1333333333333333315, 0.1375000000000000111, 0.1416666666666666630, 0.1458333333333333426, 0.1499999999999999944, 0.1541666666666666741, 0.1583333333333333259, 0.1625000000000000056, 0.1666666666666666574, 0.1708333333333333370, 0.1749999999999999889, 0.1791666666666666685, 0.1833333333333333204, 0.1875000000000000000, 0.1916666666666666796, 0.1958333333333333315, 0.2000000000000000111, 0.2041666666666666630, 0.2083333333333333426, 0.2124999999999999944, 0.2166666666666666741, 0.2208333333333333259, 0.2250000000000000056, 0.2291666666666666574, 0.2333333333333333370, 0.2374999999999999889, 0.2416666666666666685, 0.2458333333333333204, 0.2500000000000000000, 0.2541666666666666519, 0.2583333333333333592, 0.2625000000000000111, 0.2666666666666666630, 0.2708333333333333148, 0.2750000000000000222, 0.2791666666666666741, 0.2833333333333333259, 0.2874999999999999778, 0.2916666666666666852, 0.2958333333333333370, 0.2999999999999999889, 0.3041666666666666408, 0.3083333333333333481, 0.3125000000000000000, 0.3166666666666666519, 0.3208333333333333592, 0.3250000000000000111, 0.3291666666666666630, 0.3333333333333333148, 0.3375000000000000222, 0.3416666666666666741, 0.3458333333333333259, 0.3499999999999999778, 0.3541666666666666852, 0.3583333333333333370, 0.3624999999999999889, 0.3666666666666666408, 0.3708333333333333481, 0.3750000000000000000, 0.3791666666666666519, 0.3833333333333333592, 0.3875000000000000111, 0.3916666666666666630, 0.3958333333333333148, 0.4000000000000000222, 0.4041666666666666741, 0.4083333333333333259, 0.4124999999999999778, 0.4166666666666666852, 0.4208333333333333370, 0.4249999999999999889, 0.4291666666666666408, 0.4333333333333333481, 0.4375000000000000000, 0.4416666666666666519, 0.4458333333333333592, 0.4500000000000000111, 0.4541666666666666630, 0.4583333333333333148, 0.4625000000000000222, 0.4666666666666666741, 0.4708333333333333259, 0.4749999999999999778, 0.4791666666666666852, 0.4833333333333333370, 0.4874999999999999889, 0.4916666666666666408, 0.4958333333333333481, 0.5000000000000000000, 0.5041666666666666519, 0.5083333333333333037, 0.5124999999999999556, 0.5166666666666667185, 0.5208333333333333703, 0.5250000000000000222, 0.5291666666666666741, 0.5333333333333333259, 0.5374999999999999778, 0.5416666666666666297, 0.5458333333333332815, 0.5500000000000000444, 0.5541666666666666963, 0.5583333333333333481, 0.5625000000000000000, 0.5666666666666666519, 0.5708333333333333037, 0.5749999999999999556, 0.5791666666666667185, 0.5833333333333333703, 0.5875000000000000222, 0.5916666666666666741, 0.5958333333333333259, 0.5999999999999999778, 0.6041666666666666297, 0.6083333333333332815, 0.6125000000000000444, 0.6166666666666666963, 0.6208333333333333481, 0.6250000000000000000, 0.6291666666666666519, 0.6333333333333333037, 0.6374999999999999556, 0.6416666666666667185, 0.6458333333333333703, 0.6500000000000000222, 0.6541666666666666741, 0.6583333333333333259, 0.6624999999999999778, 0.6666666666666666297, 0.6708333333333332815, 0.6750000000000000444, 0.6791666666666666963, 0.6833333333333333481, 0.6875000000000000000, 0.6916666666666666519, 0.6958333333333333037, 0.6999999999999999556, 0.7041666666666667185, 0.7083333333333333703, 0.7125000000000000222, 0.7166666666666666741, 0.7208333333333333259, 0.7249999999999999778, 0.7291666666666666297, 0.7333333333333332815, 0.7375000000000000444, 0.7416666666666666963, 0.7458333333333333481, 0.7500000000000000000, 0.7541666666666666519, 0.7583333333333333037, 0.7624999999999999556, 0.7666666666666667185, 0.7708333333333333703, 0.7750000000000000222, 0.7791666666666666741, 0.7833333333333333259, 0.7874999999999999778, 0.7916666666666666297, 0.7958333333333332815, 0.8000000000000000444, 0.8041666666666666963, 0.8083333333333333481, 0.8125000000000000000, 0.8166666666666666519, 0.8208333333333333037, 0.8249999999999999556, 0.8291666666666667185, 0.8333333333333333703, 0.8375000000000000222, 0.8416666666666666741, 0.8458333333333333259, 0.8499999999999999778, 0.8541666666666666297, 0.8583333333333332815, 0.8625000000000000444, 0.8666666666666666963, 0.8708333333333333481, 0.8750000000000000000, 0.8791666666666666519, 0.8833333333333333037, 0.8874999999999999556, 0.8916666666666667185, 0.8958333333333333703, 0.9000000000000000222, 0.9041666666666666741, 0.9083333333333333259, 0.9124999999999999778, 0.9166666666666666297, 0.9208333333333332815, 0.9250000000000000444, 0.9291666666666666963, 0.9333333333333333481, 0.9375000000000000000, 0.9416666666666666519, 0.9458333333333333037, 0.9499999999999999556, 0.9541666666666667185, 0.9583333333333333703, 0.9625000000000000222, 0.9666666666666666741, 0.9708333333333333259, 0.9749999999999999778, 0.9791666666666666297, 0.9833333333333332815, 0.9875000000000000444, 0.9916666666666666963, 0.9958333333333333481, 1.000000000000000000 ),
 .UNSPECIFIED. ) 
 GEOMETRIC_REPRESENTATION_ITEM ( )  RATIONAL_B_SPLINE_SURFACE ( (
 ( 1.000000000000000000, 0.9807852804032304306, 1.000000000000000000, 0.9807852804032304306, 1.000000000000000000, 0.9807852804032304306, 1.000000000000000000, 0.9807852804032304306, 1.000000000000000000, 0.9807852804032304306, 1.000000000000000000, 0.9807852804032304306, 1.000000000000000000, 0.9807852804032304306, 1.000000000000000000, 0.9807852804032304306, 1.000000000000000000, 0.9807852804032304306, 1.000000000000000000, 0.9807852804032304306, 1.000000000000000000, 0.9807852804032304306, 1.000000000000000000, 0.9807852804032304306, 1.000000000000000000, 0.9807852804032304306, 1.000000000000000000, 0.9807852804032304306, 1.000000000000000000, 0.9807852804032304306, 1.000000000000000000, 0.9807852804032304306, 1.000000000000000000, 0.9807852804032304306, 1.000000000000000000, 0.9807852804032304306, 1.000000000000000000, 0.9807852804032304306, 1.000000000000000000, 0.9807852804032304306, 1.000000000000000000, 0.9807852804032304306, 1.000000000000000000, 0.9807852804032304306, 1.000000000000000000, 0.9807852804032304306, 1.000000000000000000, 0.9807852804032304306, 1.000000000000000000, 0.9807852804032304306, 1.000000000000000000, 0.9807852804032304306, 1.000000000000000000, 0.9807852804032304306, 1.000000000000000000, 0.9807852804032304306, 1.000000000000000000, 0.9807852804032304306, 1.000000000000000000, 0.9807852804032304306, 1.000000000000000000, 0.9807852804032304306, 1.000000000000000000, 0.9807852804032304306, 1.000000000000000000, 0.9807852804032304306, 1.000000000000000000, 0.9807852804032304306, 1.000000000000000000, 0.9807852804032304306, 1.000000000000000000, 0.9807852804032304306, 1.000000000000000000, 0.9807852804032304306, 1.000000000000000000, 0.9807852804032304306, 1.000000000000000000, 0.9807852804032304306, 1.000000000000000000, 0.9807852804032304306, 1.000000000000000000, 0.9807852804032304306, 1.000000000000000000, 0.9807852804032304306, 1.000000000000000000, 0.9807852804032304306, 1.000000000000000000, 0.9807852804032304306, 1.000000000000000000, 0.9807852804032304306, 1.000000000000000000, 0.9807852804032304306, 1.000000000000000000, 0.9807852804032304306, 1.000000000000000000, 0.9807852804032304306, 1.000000000000000000, 0.9807852804032304306, 1.000000000000000000, 0.9807852804032304306, 1.000000000000000000, 0.9807852804032304306, 1.000000000000000000, 0.9807852804032304306, 1.000000000000000000, 0.9807852804032304306, 1.000000000000000000, 0.9807852804032304306, 1.000000000000000000, 0.9807852804032304306, 1.000000000000000000, 0.9807852804032304306, 1.000000000000000000, 0.9807852804032304306, 1.000000000000000000, 0.9807852804032304306, 1.000000000000000000, 0.9807852804032304306, 1.000000000000000000, 0.9807852804032304306, 1.000000000000000000, 0.9807852804032304306, 1.000000000000000000, 0.9807852804032304306, 1.000000000000000000, 0.9807852804032304306, 1.000000000000000000, 0.9807852804032304306, 1.000000000000000000, 0.9807852804032304306, 1.000000000000000000, 0.9807852804032304306, 1.000000000000000000, 0.9807852804032304306, 1.000000000000000000, 0.9807852804032304306, 1.000000000000000000, 0.9807852804032304306, 1.000000000000000000, 0.9807852804032304306, 1.000000000000000000, 0.9807852804032304306, 1.000000000000000000, 0.9807852804032304306, 1.000000000000000000, 0.9807852804032304306, 1.000000000000000000, 0.9807852804032304306, 1.000000000000000000, 0.9807852804032304306, 1.000000000000000000, 0.9807852804032304306, 1.000000000000000000, 0.9807852804032304306, 1.000000000000000000, 0.9807852804032304306, 1.000000000000000000, 0.9807852804032304306, 1.000000000000000000, 0.9807852804032304306, 1.000000000000000000, 0.9807852804032304306, 1.000000000000000000, 0.9807852804032304306, 1.000000000000000000, 0.9807852804032304306, 1.000000000000000000, 0.9807852804032304306, 1.000000000000000000, 0.9807852804032304306, 1.000000000000000000, 0.9807852804032304306, 1.000000000000000000, 0.9807852804032304306, 1.000000000000000000, 0.9807852804032304306, 1.000000000000000000, 0.9807852804032304306, 1.000000000000000000, 0.9807852804032304306, 1.000000000000000000, 0.9807852804032304306, 1.000000000000000000, 0.9807852804032304306, 1.000000000000000000, 0.9807852804032304306, 1.000000000000000000, 0.9807852804032304306, 1.000000000000000000, 0.9807852804032304306, 1.000000000000000000, 0.9807852804032304306, 1.000000000000000000, 0.9807852804032304306, 1.000000000000000000, 0.9807852804032304306, 1.000000000000000000, 0.9807852804032304306, 1.000000000000000000, 0.9807852804032304306, 1.000000000000000000, 0.9807852804032304306, 1.000000000000000000, 0.9807852804032304306, 1.000000000000000000, 0.9807852804032304306, 1.000000000000000000, 0.9807852804032304306, 1.000000000000000000, 0.9807852804032304306, 1.000000000000000000, 0.9807852804032304306, 1.000000000000000000, 0.9807852804032304306, 1.000000000000000000, 0.9807852804032304306, 1.000000000000000000, 0.9807852804032304306, 1.000000000000000000, 0.9807852804032304306, 1.000000000000000000, 0.9807852804032304306, 1.000000000000000000, 0.9807852804032304306, 1.000000000000000000, 0.9807852804032304306, 1.000000000000000000, 0.9807852804032304306, 1.000000000000000000, 0.9807852804032304306, 1.000000000000000000, 0.9807852804032304306, 1.000000000000000000, 0.9807852804032304306, 1.000000000000000000, 0.9807852804032304306, 1.000000000000000000, 0.9807852804032304306, 1.000000000000000000, 0.9807852804032304306, 1.000000000000000000, 0.9807852804032304306, 1.000000000000000000, 0.9807852804032304306, 1.000000000000000000, 0.9807852804032304306, 1.000000000000000000, 0.9807852804032304306, 1.000000000000000000, 0.9807852804032304306, 1.000000000000000000, 0.9807852804032304306, 1.000000000000000000, 0.9807852804032304306, 1.000000000000000000, 0.9807852804032304306, 1.000000000000000000, 0.9807852804032304306, 1.000000000000000000, 0.9807852804032304306, 1.000000000000000000, 0.9807852804032304306, 1.000000000000000000, 0.9807852804032304306, 1.000000000000000000, 0.9807852804032304306, 1.000000000000000000, 0.9807852804032304306, 1.000000000000000000, 0.9807852804032304306, 1.000000000000000000, 0.9807852804032304306, 1.000000000000000000, 0.9807852804032304306, 1.000000000000000000, 0.9807852804032304306, 1.000000000000000000, 0.9807852804032304306, 1.000000000000000000, 0.9807852804032304306, 1.000000000000000000, 0.9807852804032304306, 1.000000000000000000, 0.9807852804032304306, 1.000000000000000000, 0.9807852804032304306, 1.000000000000000000, 0.9807852804032304306, 1.000000000000000000, 0.9807852804032304306, 1.000000000000000000, 0.9807852804032304306, 1.000000000000000000, 0.9807852804032304306, 1.000000000000000000, 0.9807852804032304306, 1.000000000000000000, 0.9807852804032304306, 1.000000000000000000, 0.9807852804032304306, 1.000000000000000000, 0.9807852804032304306, 1.000000000000000000, 0.9807852804032304306, 1.000000000000000000, 0.9807852804032304306, 1.000000000000000000, 0.9807852804032304306, 1.000000000000000000, 0.9807852804032304306, 1.000000000000000000, 0.9807852804032304306, 1.000000000000000000, 0.9807852804032304306, 1.000000000000000000, 0.9807852804032304306, 1.000000000000000000, 0.9807852804032304306, 1.000000000000000000, 0.9807852804032304306, 1.000000000000000000, 0.9807852804032304306, 1.000000000000000000, 0.9807852804032304306, 1.000000000000000000, 0.9807852804032304306, 1.000000000000000000, 0.9807852804032304306, 1.000000000000000000, 0.9807852804032304306, 1.000000000000000000, 0.9807852804032304306, 1.000000000000000000, 0.9807852804032304306, 1.000000000000000000, 0.9807852804032304306, 1.000000000000000000, 0.9807852804032304306, 1.000000000000000000, 0.9807852804032304306, 1.000000000000000000, 0.9807852804032304306, 1.000000000000000000, 0.9807852804032304306, 1.000000000000000000, 0.9807852804032304306, 1.000000000000000000, 0.9807852804032304306, 1.000000000000000000, 0.9807852804032304306, 1.000000000000000000, 0.9807852804032304306, 1.000000000000000000, 0.9807852804032304306, 1.000000000000000000, 0.9807852804032304306, 1.000000000000000000, 0.9807852804032304306, 1.000000000000000000, 0.9807852804032304306, 1.000000000000000000, 0.9807852804032304306, 1.000000000000000000, 0.9807852804032304306, 1.000000000000000000, 0.9807852804032304306, 1.000000000000000000, 0.9807852804032304306, 1.000000000000000000, 0.9807852804032304306, 1.000000000000000000, 0.9807852804032304306, 1.000000000000000000, 0.9807852804032304306, 1.000000000000000000, 0.9807852804032304306, 1.000000000000000000, 0.9807852804032304306, 1.000000000000000000, 0.9807852804032304306, 1.000000000000000000, 0.9807852804032304306, 1.000000000000000000, 0.9807852804032304306, 1.000000000000000000, 0.9807852804032304306, 1.000000000000000000, 0.9807852804032304306, 1.000000000000000000, 0.9807852804032304306, 1.000000000000000000, 0.9807852804032304306, 1.000000000000000000, 0.9807852804032304306, 1.000000000000000000, 0.9807852804032304306, 1.000000000000000000, 0.9807852804032304306, 1.000000000000000000, 0.9807852804032304306, 1.000000000000000000, 0.9807852804032304306, 1.000000000000000000, 0.9807852804032304306, 1.000000000000000000, 0.9807852804032304306, 1.000000000000000000, 0.9807852804032304306, 1.000000000000000000, 0.9807852804032304306, 1.000000000000000000, 0.9807852804032304306, 1.000000000000000000, 0.9807852804032304306, 1.000000000000000000, 0.9807852804032304306, 1.000000000000000000, 0.9807852804032304306, 1.000000000000000000, 0.9807852804032304306, 1.000000000000000000, 0.9807852804032304306, 1.000000000000000000, 0.9807852804032304306, 1.000000000000000000, 0.9807852804032304306, 1.000000000000000000, 0.9807852804032304306, 1.000000000000000000, 0.9807852804032304306, 1.000000000000000000, 0.9807852804032304306, 1.000000000000000000, 0.9807852804032304306, 1.000000000000000000, 0.9807852804032304306, 1.000000000000000000, 0.9807852804032304306, 1.000000000000000000, 0.9807852804032304306, 1.000000000000000000, 0.9807852804032304306, 1.000000000000000000, 0.9807852804032304306, 1.000000000000000000, 0.9807852804032304306, 1.000000000000000000, 0.9807852804032304306, 1.000000000000000000, 0.9807852804032304306, 1.000000000000000000, 0.9807852804032304306, 1.000000000000000000, 0.9807852804032304306, 1.000000000000000000, 0.9807852804032304306, 1.000000000000000000, 0.9807852804032304306, 1.000000000000000000, 0.9807852804032304306, 1.000000000000000000, 0.9807852804032304306, 1.000000000000000000, 0.9807852804032304306, 1.000000000000000000, 0.9807852804032304306, 1.000000000000000000, 0.9807852804032304306, 1.000000000000000000, 0.9807852804032304306, 1.000000000000000000, 0.9807852804032304306, 1.000000000000000000, 0.9807852804032304306, 1.000000000000000000, 0.9807852804032304306, 1.000000000000000000, 0.9807852804032304306, 1.000000000000000000, 0.9807852804032304306, 1.000000000000000000),
 ( 0.3333333333333333703, 0.3269284268010768657, 0.3333333333333333703, 0.3269284268010768657, 0.3333333333333333703, 0.3269284268010768657, 0.3333333333333333703, 0.3269284268010768657, 0.3333333333333333703, 0.3269284268010768657, 0.3333333333333333703, 0.3269284268010768657, 0.3333333333333333703, 0.3269284268010768657, 0.3333333333333333703, 0.3269284268010768657, 0.3333333333333333703, 0.3269284268010768657, 0.3333333333333333703, 0.3269284268010768657, 0.3333333333333333703, 0.3269284268010768657, 0.3333333333333333703, 0.3269284268010768657, 0.3333333333333333703, 0.3269284268010768657, 0.3333333333333333703, 0.3269284268010768657, 0.3333333333333333703, 0.3269284268010768657, 0.3333333333333333703, 0.3269284268010768657, 0.3333333333333333703, 0.3269284268010768657, 0.3333333333333333703, 0.3269284268010768657, 0.3333333333333333703, 0.3269284268010768657, 0.3333333333333333703, 0.3269284268010768657, 0.3333333333333333703, 0.3269284268010768657, 0.3333333333333333703, 0.3269284268010768657, 0.3333333333333333703, 0.3269284268010768657, 0.3333333333333333703, 0.3269284268010768657, 0.3333333333333333703, 0.3269284268010768657, 0.3333333333333333703, 0.3269284268010768657, 0.3333333333333333703, 0.3269284268010768657, 0.3333333333333333703, 0.3269284268010768657, 0.3333333333333333703, 0.3269284268010768657, 0.3333333333333333703, 0.3269284268010768657, 0.3333333333333333703, 0.3269284268010768657, 0.3333333333333333703, 0.3269284268010768657, 0.3333333333333333703, 0.3269284268010768657, 0.3333333333333333703, 0.3269284268010768657, 0.3333333333333333703, 0.3269284268010768657, 0.3333333333333333703, 0.3269284268010768657, 0.3333333333333333703, 0.3269284268010768657, 0.3333333333333333703, 0.3269284268010768657, 0.3333333333333333703, 0.3269284268010768657, 0.3333333333333333703, 0.3269284268010768657, 0.3333333333333333703, 0.3269284268010768657, 0.3333333333333333703, 0.3269284268010768657, 0.3333333333333333703, 0.3269284268010768657, 0.3333333333333333703, 0.3269284268010768657, 0.3333333333333333703, 0.3269284268010768657, 0.3333333333333333703, 0.3269284268010768657, 0.3333333333333333703, 0.3269284268010768657, 0.3333333333333333703, 0.3269284268010768657, 0.3333333333333333703, 0.3269284268010768657, 0.3333333333333333703, 0.3269284268010768657, 0.3333333333333333703, 0.3269284268010768657, 0.3333333333333333703, 0.3269284268010768657, 0.3333333333333333703, 0.3269284268010768657, 0.3333333333333333703, 0.3269284268010768657, 0.3333333333333333703, 0.3269284268010768657, 0.3333333333333333703, 0.3269284268010768657, 0.3333333333333333703, 0.3269284268010768657, 0.3333333333333333703, 0.3269284268010768657, 0.3333333333333333703, 0.3269284268010768657, 0.3333333333333333703, 0.3269284268010768657, 0.3333333333333333703, 0.3269284268010768657, 0.3333333333333333703, 0.3269284268010768657, 0.3333333333333333703, 0.3269284268010768657, 0.3333333333333333703, 0.3269284268010768657, 0.3333333333333333703, 0.3269284268010768657, 0.3333333333333333703, 0.3269284268010768657, 0.3333333333333333703, 0.3269284268010768657, 0.3333333333333333703, 0.3269284268010768657, 0.3333333333333333703, 0.3269284268010768657, 0.3333333333333333703, 0.3269284268010768657, 0.3333333333333333703, 0.3269284268010768657, 0.3333333333333333703, 0.3269284268010768657, 0.3333333333333333703, 0.3269284268010768657, 0.3333333333333333703, 0.3269284268010768657, 0.3333333333333333703, 0.3269284268010768657, 0.3333333333333333703, 0.3269284268010768657, 0.3333333333333333703, 0.3269284268010768657, 0.3333333333333333703, 0.3269284268010768657, 0.3333333333333333703, 0.3269284268010768657, 0.3333333333333333703, 0.3269284268010768657, 0.3333333333333333703, 0.3269284268010768657, 0.3333333333333333703, 0.3269284268010768657, 0.3333333333333333703, 0.3269284268010768657, 0.3333333333333333703, 0.3269284268010768657, 0.3333333333333333703, 0.3269284268010768657, 0.3333333333333333703, 0.3269284268010768657, 0.3333333333333333703, 0.3269284268010768657, 0.3333333333333333703, 0.3269284268010768657, 0.3333333333333333703, 0.3269284268010768657, 0.3333333333333333703, 0.3269284268010768657, 0.3333333333333333703, 0.3269284268010768657, 0.3333333333333333703, 0.3269284268010768657, 0.3333333333333333703, 0.3269284268010768657, 0.3333333333333333703, 0.3269284268010768657, 0.3333333333333333703, 0.3269284268010768657, 0.3333333333333333703, 0.3269284268010768657, 0.3333333333333333703, 0.3269284268010768657, 0.3333333333333333703, 0.3269284268010768657, 0.3333333333333333703, 0.3269284268010768657, 0.3333333333333333703, 0.3269284268010768657, 0.3333333333333333703, 0.3269284268010768657, 0.3333333333333333703, 0.3269284268010768657, 0.3333333333333333703, 0.3269284268010768657, 0.3333333333333333703, 0.3269284268010768657, 0.3333333333333333703, 0.3269284268010768657, 0.3333333333333333703, 0.3269284268010768657, 0.3333333333333333703, 0.3269284268010768657, 0.3333333333333333703, 0.3269284268010768657, 0.3333333333333333703, 0.3269284268010768657, 0.3333333333333333703, 0.3269284268010768657, 0.3333333333333333703, 0.3269284268010768657, 0.3333333333333333703, 0.3269284268010768657, 0.3333333333333333703, 0.3269284268010768657, 0.3333333333333333703, 0.3269284268010768657, 0.3333333333333333703, 0.3269284268010768657, 0.3333333333333333703, 0.3269284268010768657, 0.3333333333333333703, 0.3269284268010768657, 0.3333333333333333703, 0.3269284268010768657, 0.3333333333333333703, 0.3269284268010768657, 0.3333333333333333703, 0.3269284268010768657, 0.3333333333333333703, 0.3269284268010768657, 0.3333333333333333703, 0.3269284268010768657, 0.3333333333333333703, 0.3269284268010768657, 0.3333333333333333703, 0.3269284268010768657, 0.3333333333333333703, 0.3269284268010768657, 0.3333333333333333703, 0.3269284268010768657, 0.3333333333333333703, 0.3269284268010768657, 0.3333333333333333703, 0.3269284268010768657, 0.3333333333333333703, 0.3269284268010768657, 0.3333333333333333703, 0.3269284268010768657, 0.3333333333333333703, 0.3269284268010768657, 0.3333333333333333703, 0.3269284268010768657, 0.3333333333333333703, 0.3269284268010768657, 0.3333333333333333703, 0.3269284268010768657, 0.3333333333333333703, 0.3269284268010768657, 0.3333333333333333703, 0.3269284268010768657, 0.3333333333333333703, 0.3269284268010768657, 0.3333333333333333703, 0.3269284268010768657, 0.3333333333333333703, 0.3269284268010768657, 0.3333333333333333703, 0.3269284268010768657, 0.3333333333333333703, 0.3269284268010768657, 0.3333333333333333703, 0.3269284268010768657, 0.3333333333333333703, 0.3269284268010768657, 0.3333333333333333703, 0.3269284268010768657, 0.3333333333333333703, 0.3269284268010768657, 0.3333333333333333703, 0.3269284268010768657, 0.3333333333333333703, 0.3269284268010768657, 0.3333333333333333703, 0.3269284268010768657, 0.3333333333333333703, 0.3269284268010768657, 0.3333333333333333703, 0.3269284268010768657, 0.3333333333333333703, 0.3269284268010768657, 0.3333333333333333703, 0.3269284268010768657, 0.3333333333333333703, 0.3269284268010768657, 0.3333333333333333703, 0.3269284268010768657, 0.3333333333333333703, 0.3269284268010768657, 0.3333333333333333703, 0.3269284268010768657, 0.3333333333333333703, 0.3269284268010768657, 0.3333333333333333703, 0.3269284268010768657, 0.3333333333333333703, 0.3269284268010768657, 0.3333333333333333703, 0.3269284268010768657, 0.3333333333333333703, 0.3269284268010768657, 0.3333333333333333703, 0.3269284268010768657, 0.3333333333333333703, 0.3269284268010768657, 0.3333333333333333703, 0.3269284268010768657, 0.3333333333333333703, 0.3269284268010768657, 0.3333333333333333703, 0.3269284268010768657, 0.3333333333333333703, 0.3269284268010768657, 0.3333333333333333703, 0.3269284268010768657, 0.3333333333333333703, 0.3269284268010768657, 0.3333333333333333703, 0.3269284268010768657, 0.3333333333333333703, 0.3269284268010768657, 0.3333333333333333703, 0.3269284268010768657, 0.3333333333333333703, 0.3269284268010768657, 0.3333333333333333703, 0.3269284268010768657, 0.3333333333333333703, 0.3269284268010768657, 0.3333333333333333703, 0.3269284268010768657, 0.3333333333333333703, 0.3269284268010768657, 0.3333333333333333703, 0.3269284268010768657, 0.3333333333333333703, 0.3269284268010768657, 0.3333333333333333703, 0.3269284268010768657, 0.3333333333333333703, 0.3269284268010768657, 0.3333333333333333703, 0.3269284268010768657, 0.3333333333333333703, 0.3269284268010768657, 0.3333333333333333703, 0.3269284268010768657, 0.3333333333333333703, 0.3269284268010768657, 0.3333333333333333703, 0.3269284268010768657, 0.3333333333333333703, 0.3269284268010768657, 0.3333333333333333703, 0.3269284268010768657, 0.3333333333333333703, 0.3269284268010768657, 0.3333333333333333703, 0.3269284268010768657, 0.3333333333333333703, 0.3269284268010768657, 0.3333333333333333703, 0.3269284268010768657, 0.3333333333333333703, 0.3269284268010768657, 0.3333333333333333703, 0.3269284268010768657, 0.3333333333333333703, 0.3269284268010768657, 0.3333333333333333703, 0.3269284268010768657, 0.3333333333333333703, 0.3269284268010768657, 0.3333333333333333703, 0.3269284268010768657, 0.3333333333333333703, 0.3269284268010768657, 0.3333333333333333703, 0.3269284268010768657, 0.3333333333333333703, 0.3269284268010768657, 0.3333333333333333703, 0.3269284268010768657, 0.3333333333333333703, 0.3269284268010768657, 0.3333333333333333703, 0.3269284268010768657, 0.3333333333333333703, 0.3269284268010768657, 0.3333333333333333703, 0.3269284268010768657, 0.3333333333333333703, 0.3269284268010768657, 0.3333333333333333703, 0.3269284268010768657, 0.3333333333333333703, 0.3269284268010768657, 0.3333333333333333703, 0.3269284268010768657, 0.3333333333333333703, 0.3269284268010768657, 0.3333333333333333703, 0.3269284268010768657, 0.3333333333333333703, 0.3269284268010768657, 0.3333333333333333703, 0.3269284268010768657, 0.3333333333333333703, 0.3269284268010768657, 0.3333333333333333703, 0.3269284268010768657, 0.3333333333333333703, 0.3269284268010768657, 0.3333333333333333703, 0.3269284268010768657, 0.3333333333333333703, 0.3269284268010768657, 0.3333333333333333703, 0.3269284268010768657, 0.3333333333333333703, 0.3269284268010768657, 0.3333333333333333703, 0.3269284268010768657, 0.3333333333333333703, 0.3269284268010768657, 0.3333333333333333703, 0.3269284268010768657, 0.3333333333333333703, 0.3269284268010768657, 0.3333333333333333703, 0.3269284268010768657, 0.3333333333333333703, 0.3269284268010768657, 0.3333333333333333703, 0.3269284268010768657, 0.3333333333333333703, 0.3269284268010768657, 0.3333333333333333703, 0.3269284268010768657, 0.3333333333333333703, 0.3269284268010768657, 0.3333333333333333703, 0.3269284268010768657, 0.3333333333333333703, 0.3269284268010768657, 0.3333333333333333703, 0.3269284268010768657, 0.3333333333333333703, 0.3269284268010768657, 0.3333333333333333703, 0.3269284268010768657, 0.3333333333333333703, 0.3269284268010768657, 0.3333333333333333703, 0.3269284268010768657, 0.3333333333333333703, 0.3269284268010768657, 0.3333333333333333703, 0.3269284268010768657, 0.3333333333333333703),
 ( 0.3333333333333333703, 0.3269284268010768657, 0.3333333333333333703, 0.3269284268010768657, 0.3333333333333333703, 0.3269284268010768657, 0.3333333333333333703, 0.3269284268010768657, 0.3333333333333333703, 0.3269284268010768657, 0.3333333333333333703, 0.3269284268010768657, 0.3333333333333333703, 0.3269284268010768657, 0.3333333333333333703, 0.3269284268010768657, 0.3333333333333333703, 0.3269284268010768657, 0.3333333333333333703, 0.3269284268010768657, 0.3333333333333333703, 0.3269284268010768657, 0.3333333333333333703, 0.3269284268010768657, 0.3333333333333333703, 0.3269284268010768657, 0.3333333333333333703, 0.3269284268010768657, 0.3333333333333333703, 0.3269284268010768657, 0.3333333333333333703, 0.3269284268010768657, 0.3333333333333333703, 0.3269284268010768657, 0.3333333333333333703, 0.3269284268010768657, 0.3333333333333333703, 0.3269284268010768657, 0.3333333333333333703, 0.3269284268010768657, 0.3333333333333333703, 0.3269284268010768657, 0.3333333333333333703, 0.3269284268010768657, 0.3333333333333333703, 0.3269284268010768657, 0.3333333333333333703, 0.3269284268010768657, 0.3333333333333333703, 0.3269284268010768657, 0.3333333333333333703, 0.3269284268010768657, 0.3333333333333333703, 0.3269284268010768657, 0.3333333333333333703, 0.3269284268010768657, 0.3333333333333333703, 0.3269284268010768657, 0.3333333333333333703, 0.3269284268010768657, 0.3333333333333333703, 0.3269284268010768657, 0.3333333333333333703, 0.3269284268010768657, 0.3333333333333333703, 0.3269284268010768657, 0.3333333333333333703, 0.3269284268010768657, 0.3333333333333333703, 0.3269284268010768657, 0.3333333333333333703, 0.3269284268010768657, 0.3333333333333333703, 0.3269284268010768657, 0.3333333333333333703, 0.3269284268010768657, 0.3333333333333333703, 0.3269284268010768657, 0.3333333333333333703, 0.3269284268010768657, 0.3333333333333333703, 0.3269284268010768657, 0.3333333333333333703, 0.3269284268010768657, 0.3333333333333333703, 0.3269284268010768657, 0.3333333333333333703, 0.3269284268010768657, 0.3333333333333333703, 0.3269284268010768657, 0.3333333333333333703, 0.3269284268010768657, 0.3333333333333333703, 0.3269284268010768657, 0.3333333333333333703, 0.3269284268010768657, 0.3333333333333333703, 0.3269284268010768657, 0.3333333333333333703, 0.3269284268010768657, 0.3333333333333333703, 0.3269284268010768657, 0.3333333333333333703, 0.3269284268010768657, 0.3333333333333333703, 0.3269284268010768657, 0.3333333333333333703, 0.3269284268010768657, 0.3333333333333333703, 0.3269284268010768657, 0.3333333333333333703, 0.3269284268010768657, 0.3333333333333333703, 0.3269284268010768657, 0.3333333333333333703, 0.3269284268010768657, 0.3333333333333333703, 0.3269284268010768657, 0.3333333333333333703, 0.3269284268010768657, 0.3333333333333333703, 0.3269284268010768657, 0.3333333333333333703, 0.3269284268010768657, 0.3333333333333333703, 0.3269284268010768657, 0.3333333333333333703, 0.3269284268010768657, 0.3333333333333333703, 0.3269284268010768657, 0.3333333333333333703, 0.3269284268010768657, 0.3333333333333333703, 0.3269284268010768657, 0.3333333333333333703, 0.3269284268010768657, 0.3333333333333333703, 0.3269284268010768657, 0.3333333333333333703, 0.3269284268010768657, 0.3333333333333333703, 0.3269284268010768657, 0.3333333333333333703, 0.3269284268010768657, 0.3333333333333333703, 0.3269284268010768657, 0.3333333333333333703, 0.3269284268010768657, 0.3333333333333333703, 0.3269284268010768657, 0.3333333333333333703, 0.3269284268010768657, 0.3333333333333333703, 0.3269284268010768657, 0.3333333333333333703, 0.3269284268010768657, 0.3333333333333333703, 0.3269284268010768657, 0.3333333333333333703, 0.3269284268010768657, 0.3333333333333333703, 0.3269284268010768657, 0.3333333333333333703, 0.3269284268010768657, 0.3333333333333333703, 0.3269284268010768657, 0.3333333333333333703, 0.3269284268010768657, 0.3333333333333333703, 0.3269284268010768657, 0.3333333333333333703, 0.3269284268010768657, 0.3333333333333333703, 0.3269284268010768657, 0.3333333333333333703, 0.3269284268010768657, 0.3333333333333333703, 0.3269284268010768657, 0.3333333333333333703, 0.3269284268010768657, 0.3333333333333333703, 0.3269284268010768657, 0.3333333333333333703, 0.3269284268010768657, 0.3333333333333333703, 0.3269284268010768657, 0.3333333333333333703, 0.3269284268010768657, 0.3333333333333333703, 0.3269284268010768657, 0.3333333333333333703, 0.3269284268010768657, 0.3333333333333333703, 0.3269284268010768657, 0.3333333333333333703, 0.3269284268010768657, 0.3333333333333333703, 0.3269284268010768657, 0.3333333333333333703, 0.3269284268010768657, 0.3333333333333333703, 0.3269284268010768657, 0.3333333333333333703, 0.3269284268010768657, 0.3333333333333333703, 0.3269284268010768657, 0.3333333333333333703, 0.3269284268010768657, 0.3333333333333333703, 0.3269284268010768657, 0.3333333333333333703, 0.3269284268010768657, 0.3333333333333333703, 0.3269284268010768657, 0.3333333333333333703, 0.3269284268010768657, 0.3333333333333333703, 0.3269284268010768657, 0.3333333333333333703, 0.3269284268010768657, 0.3333333333333333703, 0.3269284268010768657, 0.3333333333333333703, 0.3269284268010768657, 0.3333333333333333703, 0.3269284268010768657, 0.3333333333333333703, 0.3269284268010768657, 0.3333333333333333703, 0.3269284268010768657, 0.3333333333333333703, 0.3269284268010768657, 0.3333333333333333703, 0.3269284268010768657, 0.3333333333333333703, 0.3269284268010768657, 0.3333333333333333703, 0.3269284268010768657, 0.3333333333333333703, 0.3269284268010768657, 0.3333333333333333703, 0.3269284268010768657, 0.3333333333333333703, 0.3269284268010768657, 0.3333333333333333703, 0.3269284268010768657, 0.3333333333333333703, 0.3269284268010768657, 0.3333333333333333703, 0.3269284268010768657, 0.3333333333333333703, 0.3269284268010768657, 0.3333333333333333703, 0.3269284268010768657, 0.3333333333333333703, 0.3269284268010768657, 0.3333333333333333703, 0.3269284268010768657, 0.3333333333333333703, 0.3269284268010768657, 0.3333333333333333703, 0.3269284268010768657, 0.3333333333333333703, 0.3269284268010768657, 0.3333333333333333703, 0.3269284268010768657, 0.3333333333333333703, 0.3269284268010768657, 0.3333333333333333703, 0.3269284268010768657, 0.3333333333333333703, 0.3269284268010768657, 0.3333333333333333703, 0.3269284268010768657, 0.3333333333333333703, 0.3269284268010768657, 0.3333333333333333703, 0.3269284268010768657, 0.3333333333333333703, 0.3269284268010768657, 0.3333333333333333703, 0.3269284268010768657, 0.3333333333333333703, 0.3269284268010768657, 0.3333333333333333703, 0.3269284268010768657, 0.3333333333333333703, 0.3269284268010768657, 0.3333333333333333703, 0.3269284268010768657, 0.3333333333333333703, 0.3269284268010768657, 0.3333333333333333703, 0.3269284268010768657, 0.3333333333333333703, 0.3269284268010768657, 0.3333333333333333703, 0.3269284268010768657, 0.3333333333333333703, 0.3269284268010768657, 0.3333333333333333703, 0.3269284268010768657, 0.3333333333333333703, 0.3269284268010768657, 0.3333333333333333703, 0.3269284268010768657, 0.3333333333333333703, 0.3269284268010768657, 0.3333333333333333703, 0.3269284268010768657, 0.3333333333333333703, 0.3269284268010768657, 0.3333333333333333703, 0.3269284268010768657, 0.3333333333333333703, 0.3269284268010768657, 0.3333333333333333703, 0.3269284268010768657, 0.3333333333333333703, 0.3269284268010768657, 0.3333333333333333703, 0.3269284268010768657, 0.3333333333333333703, 0.3269284268010768657, 0.3333333333333333703, 0.3269284268010768657, 0.3333333333333333703, 0.3269284268010768657, 0.3333333333333333703, 0.3269284268010768657, 0.3333333333333333703, 0.3269284268010768657, 0.3333333333333333703, 0.3269284268010768657, 0.3333333333333333703, 0.3269284268010768657, 0.3333333333333333703, 0.3269284268010768657, 0.3333333333333333703, 0.3269284268010768657, 0.3333333333333333703, 0.3269284268010768657, 0.3333333333333333703, 0.3269284268010768657, 0.3333333333333333703, 0.3269284268010768657, 0.3333333333333333703, 0.3269284268010768657, 0.3333333333333333703, 0.3269284268010768657, 0.3333333333333333703, 0.3269284268010768657, 0.3333333333333333703, 0.3269284268010768657, 0.3333333333333333703, 0.3269284268010768657, 0.3333333333333333703, 0.3269284268010768657, 0.3333333333333333703, 0.3269284268010768657, 0.3333333333333333703, 0.3269284268010768657, 0.3333333333333333703, 0.3269284268010768657, 0.3333333333333333703, 0.3269284268010768657, 0.3333333333333333703, 0.3269284268010768657, 0.3333333333333333703, 0.3269284268010768657, 0.3333333333333333703, 0.3269284268010768657, 0.3333333333333333703, 0.3269284268010768657, 0.3333333333333333703, 0.3269284268010768657, 0.3333333333333333703, 0.3269284268010768657, 0.3333333333333333703, 0.3269284268010768657, 0.3333333333333333703, 0.3269284268010768657, 0.3333333333333333703, 0.3269284268010768657, 0.3333333333333333703, 0.3269284268010768657, 0.3333333333333333703, 0.3269284268010768657, 0.3333333333333333703, 0.3269284268010768657, 0.3333333333333333703, 0.3269284268010768657, 0.3333333333333333703, 0.3269284268010768657, 0.3333333333333333703, 0.3269284268010768657, 0.3333333333333333703, 0.3269284268010768657, 0.3333333333333333703, 0.3269284268010768657, 0.3333333333333333703, 0.3269284268010768657, 0.3333333333333333703, 0.3269284268010768657, 0.3333333333333333703, 0.3269284268010768657, 0.3333333333333333703, 0.3269284268010768657, 0.3333333333333333703, 0.3269284268010768657, 0.3333333333333333703, 0.3269284268010768657, 0.3333333333333333703, 0.3269284268010768657, 0.3333333333333333703, 0.3269284268010768657, 0.3333333333333333703, 0.3269284268010768657, 0.3333333333333333703, 0.3269284268010768657, 0.3333333333333333703, 0.3269284268010768657, 0.3333333333333333703, 0.3269284268010768657, 0.3333333333333333703, 0.3269284268010768657, 0.3333333333333333703, 0.3269284268010768657, 0.3333333333333333703, 0.3269284268010768657, 0.3333333333333333703, 0.3269284268010768657, 0.3333333333333333703, 0.3269284268010768657, 0.3333333333333333703, 0.3269284268010768657, 0.3333333333333333703, 0.3269284268010768657, 0.3333333333333333703, 0.3269284268010768657, 0.3333333333333333703, 0.3269284268010768657, 0.3333333333333333703, 0.3269284268010768657, 0.3333333333333333703, 0.3269284268010768657, 0.3333333333333333703, 0.3269284268010768657, 0.3333333333333333703, 0.3269284268010768657, 0.3333333333333333703, 0.3269284268010768657, 0.3333333333333333703, 0.3269284268010768657, 0.3333333333333333703, 0.3269284268010768657, 0.3333333333333333703, 0.3269284268010768657, 0.3333333333333333703, 0.3269284268010768657, 0.3333333333333333703, 0.3269284268010768657, 0.3333333333333333703, 0.3269284268010768657, 0.3333333333333333703, 0.3269284268010768657, 0.3333333333333333703, 0.3269284268010768657, 0.3333333333333333703, 0.3269284268010768657, 0.3333333333333333703, 0.3269284268010768657, 0.3333333333333333703, 0.3269284268010768657, 0.3333333333333333703, 0.3269284268010768657, 0.3333333333333333703, 0.3269284268010768657, 0.3333333333333333703, 0.3269284268010768657, 0.3333333333333333703),
 ( 1.000000000000000000, 0.9807852804032304306, 1.000000000000000000, 0.9807852804032304306, 1.000000000000000000, 0.9807852804032304306, 1.000000000000000000, 0.9807852804032304306, 1.000000000000000000, 0.9807852804032304306, 1.000000000000000000, 0.9807852804032304306, 1.000000000000000000, 0.9807852804032304306, 1.000000000000000000, 0.9807852804032304306, 1.000000000000000000, 0.9807852804032304306, 1.000000000000000000, 0.9807852804032304306, 1.000000000000000000, 0.9807852804032304306, 1.000000000000000000, 0.9807852804032304306, 1.000000000000000000, 0.9807852804032304306, 1.000000000000000000, 0.9807852804032304306, 1.000000000000000000, 0.9807852804032304306, 1.000000000000000000, 0.9807852804032304306, 1.000000000000000000, 0.9807852804032304306, 1.000000000000000000, 0.9807852804032304306, 1.000000000000000000, 0.9807852804032304306, 1.000000000000000000, 0.9807852804032304306, 1.000000000000000000, 0.9807852804032304306, 1.000000000000000000, 0.9807852804032304306, 1.000000000000000000, 0.9807852804032304306, 1.000000000000000000, 0.9807852804032304306, 1.000000000000000000, 0.9807852804032304306, 1.000000000000000000, 0.9807852804032304306, 1.000000000000000000, 0.9807852804032304306, 1.000000000000000000, 0.9807852804032304306, 1.000000000000000000, 0.9807852804032304306, 1.000000000000000000, 0.9807852804032304306, 1.000000000000000000, 0.9807852804032304306, 1.000000000000000000, 0.9807852804032304306, 1.000000000000000000, 0.9807852804032304306, 1.000000000000000000, 0.9807852804032304306, 1.000000000000000000, 0.9807852804032304306, 1.000000000000000000, 0.9807852804032304306, 1.000000000000000000, 0.9807852804032304306, 1.000000000000000000, 0.9807852804032304306, 1.000000000000000000, 0.9807852804032304306, 1.000000000000000000, 0.9807852804032304306, 1.000000000000000000, 0.9807852804032304306, 1.000000000000000000, 0.9807852804032304306, 1.000000000000000000, 0.9807852804032304306, 1.000000000000000000, 0.9807852804032304306, 1.000000000000000000, 0.9807852804032304306, 1.000000000000000000, 0.9807852804032304306, 1.000000000000000000, 0.9807852804032304306, 1.000000000000000000, 0.9807852804032304306, 1.000000000000000000, 0.9807852804032304306, 1.000000000000000000, 0.9807852804032304306, 1.000000000000000000, 0.9807852804032304306, 1.000000000000000000, 0.9807852804032304306, 1.000000000000000000, 0.9807852804032304306, 1.000000000000000000, 0.9807852804032304306, 1.000000000000000000, 0.9807852804032304306, 1.000000000000000000, 0.9807852804032304306, 1.000000000000000000, 0.9807852804032304306, 1.000000000000000000, 0.9807852804032304306, 1.000000000000000000, 0.9807852804032304306, 1.000000000000000000, 0.9807852804032304306, 1.000000000000000000, 0.9807852804032304306, 1.000000000000000000, 0.9807852804032304306, 1.000000000000000000, 0.9807852804032304306, 1.000000000000000000, 0.9807852804032304306, 1.000000000000000000, 0.9807852804032304306, 1.000000000000000000, 0.9807852804032304306, 1.000000000000000000, 0.9807852804032304306, 1.000000000000000000, 0.9807852804032304306, 1.000000000000000000, 0.9807852804032304306, 1.000000000000000000, 0.9807852804032304306, 1.000000000000000000, 0.9807852804032304306, 1.000000000000000000, 0.9807852804032304306, 1.000000000000000000, 0.9807852804032304306, 1.000000000000000000, 0.9807852804032304306, 1.000000000000000000, 0.9807852804032304306, 1.000000000000000000, 0.9807852804032304306, 1.000000000000000000, 0.9807852804032304306, 1.000000000000000000, 0.9807852804032304306, 1.000000000000000000, 0.9807852804032304306, 1.000000000000000000, 0.9807852804032304306, 1.000000000000000000, 0.9807852804032304306, 1.000000000000000000, 0.9807852804032304306, 1.000000000000000000, 0.9807852804032304306, 1.000000000000000000, 0.9807852804032304306, 1.000000000000000000, 0.9807852804032304306, 1.000000000000000000, 0.9807852804032304306, 1.000000000000000000, 0.9807852804032304306, 1.000000000000000000, 0.9807852804032304306, 1.000000000000000000, 0.9807852804032304306, 1.000000000000000000, 0.9807852804032304306, 1.000000000000000000, 0.9807852804032304306, 1.000000000000000000, 0.9807852804032304306, 1.000000000000000000, 0.9807852804032304306, 1.000000000000000000, 0.9807852804032304306, 1.000000000000000000, 0.9807852804032304306, 1.000000000000000000, 0.9807852804032304306, 1.000000000000000000, 0.9807852804032304306, 1.000000000000000000, 0.9807852804032304306, 1.000000000000000000, 0.9807852804032304306, 1.000000000000000000, 0.9807852804032304306, 1.000000000000000000, 0.9807852804032304306, 1.000000000000000000, 0.9807852804032304306, 1.000000000000000000, 0.9807852804032304306, 1.000000000000000000, 0.9807852804032304306, 1.000000000000000000, 0.9807852804032304306, 1.000000000000000000, 0.9807852804032304306, 1.000000000000000000, 0.9807852804032304306, 1.000000000000000000, 0.9807852804032304306, 1.000000000000000000, 0.9807852804032304306, 1.000000000000000000, 0.9807852804032304306, 1.000000000000000000, 0.9807852804032304306, 1.000000000000000000, 0.9807852804032304306, 1.000000000000000000, 0.9807852804032304306, 1.000000000000000000, 0.9807852804032304306, 1.000000000000000000, 0.9807852804032304306, 1.000000000000000000, 0.9807852804032304306, 1.000000000000000000, 0.9807852804032304306, 1.000000000000000000, 0.9807852804032304306, 1.000000000000000000, 0.9807852804032304306, 1.000000000000000000, 0.9807852804032304306, 1.000000000000000000, 0.9807852804032304306, 1.000000000000000000, 0.9807852804032304306, 1.000000000000000000, 0.9807852804032304306, 1.000000000000000000, 0.9807852804032304306, 1.000000000000000000, 0.9807852804032304306, 1.000000000000000000, 0.9807852804032304306, 1.000000000000000000, 0.9807852804032304306, 1.000000000000000000, 0.9807852804032304306, 1.000000000000000000, 0.9807852804032304306, 1.000000000000000000, 0.9807852804032304306, 1.000000000000000000, 0.9807852804032304306, 1.000000000000000000, 0.9807852804032304306, 1.000000000000000000, 0.9807852804032304306, 1.000000000000000000, 0.9807852804032304306, 1.000000000000000000, 0.9807852804032304306, 1.000000000000000000, 0.9807852804032304306, 1.000000000000000000, 0.9807852804032304306, 1.000000000000000000, 0.9807852804032304306, 1.000000000000000000, 0.9807852804032304306, 1.000000000000000000, 0.9807852804032304306, 1.000000000000000000, 0.9807852804032304306, 1.000000000000000000, 0.9807852804032304306, 1.000000000000000000, 0.9807852804032304306, 1.000000000000000000, 0.9807852804032304306, 1.000000000000000000, 0.9807852804032304306, 1.000000000000000000, 0.9807852804032304306, 1.000000000000000000, 0.9807852804032304306, 1.000000000000000000, 0.9807852804032304306, 1.000000000000000000, 0.9807852804032304306, 1.000000000000000000, 0.9807852804032304306, 1.000000000000000000, 0.9807852804032304306, 1.000000000000000000, 0.9807852804032304306, 1.000000000000000000, 0.9807852804032304306, 1.000000000000000000, 0.9807852804032304306, 1.000000000000000000, 0.9807852804032304306, 1.000000000000000000, 0.9807852804032304306, 1.000000000000000000, 0.9807852804032304306, 1.000000000000000000, 0.9807852804032304306, 1.000000000000000000, 0.9807852804032304306, 1.000000000000000000, 0.9807852804032304306, 1.000000000000000000, 0.9807852804032304306, 1.000000000000000000, 0.9807852804032304306, 1.000000000000000000, 0.9807852804032304306, 1.000000000000000000, 0.9807852804032304306, 1.000000000000000000, 0.9807852804032304306, 1.000000000000000000, 0.9807852804032304306, 1.000000000000000000, 0.9807852804032304306, 1.000000000000000000, 0.9807852804032304306, 1.000000000000000000, 0.9807852804032304306, 1.000000000000000000, 0.9807852804032304306, 1.000000000000000000, 0.9807852804032304306, 1.000000000000000000, 0.9807852804032304306, 1.000000000000000000, 0.9807852804032304306, 1.000000000000000000, 0.9807852804032304306, 1.000000000000000000, 0.9807852804032304306, 1.000000000000000000, 0.9807852804032304306, 1.000000000000000000, 0.9807852804032304306, 1.000000000000000000, 0.9807852804032304306, 1.000000000000000000, 0.9807852804032304306, 1.000000000000000000, 0.9807852804032304306, 1.000000000000000000, 0.9807852804032304306, 1.000000000000000000, 0.9807852804032304306, 1.000000000000000000, 0.9807852804032304306, 1.000000000000000000, 0.9807852804032304306, 1.000000000000000000, 0.9807852804032304306, 1.000000000000000000, 0.9807852804032304306, 1.000000000000000000, 0.9807852804032304306, 1.000000000000000000, 0.9807852804032304306, 1.000000000000000000, 0.9807852804032304306, 1.000000000000000000, 0.9807852804032304306, 1.000000000000000000, 0.9807852804032304306, 1.000000000000000000, 0.9807852804032304306, 1.000000000000000000, 0.9807852804032304306, 1.000000000000000000, 0.9807852804032304306, 1.000000000000000000, 0.9807852804032304306, 1.000000000000000000, 0.9807852804032304306, 1.000000000000000000, 0.9807852804032304306, 1.000000000000000000, 0.9807852804032304306, 1.000000000000000000, 0.9807852804032304306, 1.000000000000000000, 0.9807852804032304306, 1.000000000000000000, 0.9807852804032304306, 1.000000000000000000, 0.9807852804032304306, 1.000000000000000000, 0.9807852804032304306, 1.000000000000000000, 0.9807852804032304306, 1.000000000000000000, 0.9807852804032304306, 1.000000000000000000, 0.9807852804032304306, 1.000000000000000000, 0.9807852804032304306, 1.000000000000000000, 0.9807852804032304306, 1.000000000000000000, 0.9807852804032304306, 1.000000000000000000, 0.9807852804032304306, 1.000000000000000000, 0.9807852804032304306, 1.000000000000000000, 0.9807852804032304306, 1.000000000000000000, 0.9807852804032304306, 1.000000000000000000, 0.9807852804032304306, 1.000000000000000000, 0.9807852804032304306, 1.000000000000000000, 0.9807852804032304306, 1.000000000000000000, 0.9807852804032304306, 1.000000000000000000, 0.9807852804032304306, 1.000000000000000000, 0.9807852804032304306, 1.000000000000000000, 0.9807852804032304306, 1.000000000000000000, 0.9807852804032304306, 1.000000000000000000, 0.9807852804032304306, 1.000000000000000000, 0.9807852804032304306, 1.000000000000000000, 0.9807852804032304306, 1.000000000000000000, 0.9807852804032304306, 1.000000000000000000, 0.9807852804032304306, 1.000000000000000000, 0.9807852804032304306, 1.000000000000000000, 0.9807852804032304306, 1.000000000000000000, 0.9807852804032304306, 1.000000000000000000, 0.9807852804032304306, 1.000000000000000000, 0.9807852804032304306, 1.000000000000000000, 0.9807852804032304306, 1.000000000000000000, 0.9807852804032304306, 1.000000000000000000, 0.9807852804032304306, 1.000000000000000000, 0.9807852804032304306, 1.000000000000000000, 0.9807852804032304306, 1.000000000000000000, 0.9807852804032304306, 1.000000000000000000, 0.9807852804032304306, 1.000000000000000000, 0.9807852804032304306, 1.000000000000000000, 0.9807852804032304306, 1.000000000000000000),
 ( 0.3333333333333333703, 0.3269284268010768657, 0.3333333333333333703, 0.3269284268010768657, 0.3333333333333333703, 0.3269284268010768657, 0.3333333333333333703, 0.3269284268010768657, 0.3333333333333333703, 0.3269284268010768657, 0.3333333333333333703, 0.3269284268010768657, 0.3333333333333333703, 0.3269284268010768657, 0.3333333333333333703, 0.3269284268010768657, 0.3333333333333333703, 0.3269284268010768657, 0.3333333333333333703, 0.3269284268010768657, 0.3333333333333333703, 0.3269284268010768657, 0.3333333333333333703, 0.3269284268010768657, 0.3333333333333333703, 0.3269284268010768657, 0.3333333333333333703, 0.3269284268010768657, 0.3333333333333333703, 0.3269284268010768657, 0.3333333333333333703, 0.3269284268010768657, 0.3333333333333333703, 0.3269284268010768657, 0.3333333333333333703, 0.3269284268010768657, 0.3333333333333333703, 0.3269284268010768657, 0.3333333333333333703, 0.3269284268010768657, 0.3333333333333333703, 0.3269284268010768657, 0.3333333333333333703, 0.3269284268010768657, 0.3333333333333333703, 0.3269284268010768657, 0.3333333333333333703, 0.3269284268010768657, 0.3333333333333333703, 0.3269284268010768657, 0.3333333333333333703, 0.3269284268010768657, 0.3333333333333333703, 0.3269284268010768657, 0.3333333333333333703, 0.3269284268010768657, 0.3333333333333333703, 0.3269284268010768657, 0.3333333333333333703, 0.3269284268010768657, 0.3333333333333333703, 0.3269284268010768657, 0.3333333333333333703, 0.3269284268010768657, 0.3333333333333333703, 0.3269284268010768657, 0.3333333333333333703, 0.3269284268010768657, 0.3333333333333333703, 0.3269284268010768657, 0.3333333333333333703, 0.3269284268010768657, 0.3333333333333333703, 0.3269284268010768657, 0.3333333333333333703, 0.3269284268010768657, 0.3333333333333333703, 0.3269284268010768657, 0.3333333333333333703, 0.3269284268010768657, 0.3333333333333333703, 0.3269284268010768657, 0.3333333333333333703, 0.3269284268010768657, 0.3333333333333333703, 0.3269284268010768657, 0.3333333333333333703, 0.3269284268010768657, 0.3333333333333333703, 0.3269284268010768657, 0.3333333333333333703, 0.3269284268010768657, 0.3333333333333333703, 0.3269284268010768657, 0.3333333333333333703, 0.3269284268010768657, 0.3333333333333333703, 0.3269284268010768657, 0.3333333333333333703, 0.3269284268010768657, 0.3333333333333333703, 0.3269284268010768657, 0.3333333333333333703, 0.3269284268010768657, 0.3333333333333333703, 0.3269284268010768657, 0.3333333333333333703, 0.3269284268010768657, 0.3333333333333333703, 0.3269284268010768657, 0.3333333333333333703, 0.3269284268010768657, 0.3333333333333333703, 0.3269284268010768657, 0.3333333333333333703, 0.3269284268010768657, 0.3333333333333333703, 0.3269284268010768657, 0.3333333333333333703, 0.3269284268010768657, 0.3333333333333333703, 0.3269284268010768657, 0.3333333333333333703, 0.3269284268010768657, 0.3333333333333333703, 0.3269284268010768657, 0.3333333333333333703, 0.3269284268010768657, 0.3333333333333333703, 0.3269284268010768657, 0.3333333333333333703, 0.3269284268010768657, 0.3333333333333333703, 0.3269284268010768657, 0.3333333333333333703, 0.3269284268010768657, 0.3333333333333333703, 0.3269284268010768657, 0.3333333333333333703, 0.3269284268010768657, 0.3333333333333333703, 0.3269284268010768657, 0.3333333333333333703, 0.3269284268010768657, 0.3333333333333333703, 0.3269284268010768657, 0.3333333333333333703, 0.3269284268010768657, 0.3333333333333333703, 0.3269284268010768657, 0.3333333333333333703, 0.3269284268010768657, 0.3333333333333333703, 0.3269284268010768657, 0.3333333333333333703, 0.3269284268010768657, 0.3333333333333333703, 0.3269284268010768657, 0.3333333333333333703, 0.3269284268010768657, 0.3333333333333333703, 0.3269284268010768657, 0.3333333333333333703, 0.3269284268010768657, 0.3333333333333333703, 0.3269284268010768657, 0.3333333333333333703, 0.3269284268010768657, 0.3333333333333333703, 0.3269284268010768657, 0.3333333333333333703, 0.3269284268010768657, 0.3333333333333333703, 0.3269284268010768657, 0.3333333333333333703, 0.3269284268010768657, 0.3333333333333333703, 0.3269284268010768657, 0.3333333333333333703, 0.3269284268010768657, 0.3333333333333333703, 0.3269284268010768657, 0.3333333333333333703, 0.3269284268010768657, 0.3333333333333333703, 0.3269284268010768657, 0.3333333333333333703, 0.3269284268010768657, 0.3333333333333333703, 0.3269284268010768657, 0.3333333333333333703, 0.3269284268010768657, 0.3333333333333333703, 0.3269284268010768657, 0.3333333333333333703, 0.3269284268010768657, 0.3333333333333333703, 0.3269284268010768657, 0.3333333333333333703, 0.3269284268010768657, 0.3333333333333333703, 0.3269284268010768657, 0.3333333333333333703, 0.3269284268010768657, 0.3333333333333333703, 0.3269284268010768657, 0.3333333333333333703, 0.3269284268010768657, 0.3333333333333333703, 0.3269284268010768657, 0.3333333333333333703, 0.3269284268010768657, 0.3333333333333333703, 0.3269284268010768657, 0.3333333333333333703, 0.3269284268010768657, 0.3333333333333333703, 0.3269284268010768657, 0.3333333333333333703, 0.3269284268010768657, 0.3333333333333333703, 0.3269284268010768657, 0.3333333333333333703, 0.3269284268010768657, 0.3333333333333333703, 0.3269284268010768657, 0.3333333333333333703, 0.3269284268010768657, 0.3333333333333333703, 0.3269284268010768657, 0.3333333333333333703, 0.3269284268010768657, 0.3333333333333333703, 0.3269284268010768657, 0.3333333333333333703, 0.3269284268010768657, 0.3333333333333333703, 0.3269284268010768657, 0.3333333333333333703, 0.3269284268010768657, 0.3333333333333333703, 0.3269284268010768657, 0.3333333333333333703, 0.3269284268010768657, 0.3333333333333333703, 0.3269284268010768657, 0.3333333333333333703, 0.3269284268010768657, 0.3333333333333333703, 0.3269284268010768657, 0.3333333333333333703, 0.3269284268010768657, 0.3333333333333333703, 0.3269284268010768657, 0.3333333333333333703, 0.3269284268010768657, 0.3333333333333333703, 0.3269284268010768657, 0.3333333333333333703, 0.3269284268010768657, 0.3333333333333333703, 0.3269284268010768657, 0.3333333333333333703, 0.3269284268010768657, 0.3333333333333333703, 0.3269284268010768657, 0.3333333333333333703, 0.3269284268010768657, 0.3333333333333333703, 0.3269284268010768657, 0.3333333333333333703, 0.3269284268010768657, 0.3333333333333333703, 0.3269284268010768657, 0.3333333333333333703, 0.3269284268010768657, 0.3333333333333333703, 0.3269284268010768657, 0.3333333333333333703, 0.3269284268010768657, 0.3333333333333333703, 0.3269284268010768657, 0.3333333333333333703, 0.3269284268010768657, 0.3333333333333333703, 0.3269284268010768657, 0.3333333333333333703, 0.3269284268010768657, 0.3333333333333333703, 0.3269284268010768657, 0.3333333333333333703, 0.3269284268010768657, 0.3333333333333333703, 0.3269284268010768657, 0.3333333333333333703, 0.3269284268010768657, 0.3333333333333333703, 0.3269284268010768657, 0.3333333333333333703, 0.3269284268010768657, 0.3333333333333333703, 0.3269284268010768657, 0.3333333333333333703, 0.3269284268010768657, 0.3333333333333333703, 0.3269284268010768657, 0.3333333333333333703, 0.3269284268010768657, 0.3333333333333333703, 0.3269284268010768657, 0.3333333333333333703, 0.3269284268010768657, 0.3333333333333333703, 0.3269284268010768657, 0.3333333333333333703, 0.3269284268010768657, 0.3333333333333333703, 0.3269284268010768657, 0.3333333333333333703, 0.3269284268010768657, 0.3333333333333333703, 0.3269284268010768657, 0.3333333333333333703, 0.3269284268010768657, 0.3333333333333333703, 0.3269284268010768657, 0.3333333333333333703, 0.3269284268010768657, 0.3333333333333333703, 0.3269284268010768657, 0.3333333333333333703, 0.3269284268010768657, 0.3333333333333333703, 0.3269284268010768657, 0.3333333333333333703, 0.3269284268010768657, 0.3333333333333333703, 0.3269284268010768657, 0.3333333333333333703, 0.3269284268010768657, 0.3333333333333333703, 0.3269284268010768657, 0.3333333333333333703, 0.3269284268010768657, 0.3333333333333333703, 0.3269284268010768657, 0.3333333333333333703, 0.3269284268010768657, 0.3333333333333333703, 0.3269284268010768657, 0.3333333333333333703, 0.3269284268010768657, 0.3333333333333333703, 0.3269284268010768657, 0.3333333333333333703, 0.3269284268010768657, 0.3333333333333333703, 0.3269284268010768657, 0.3333333333333333703, 0.3269284268010768657, 0.3333333333333333703, 0.3269284268010768657, 0.3333333333333333703, 0.3269284268010768657, 0.3333333333333333703, 0.3269284268010768657, 0.3333333333333333703, 0.3269284268010768657, 0.3333333333333333703, 0.3269284268010768657, 0.3333333333333333703, 0.3269284268010768657, 0.3333333333333333703, 0.3269284268010768657, 0.3333333333333333703, 0.3269284268010768657, 0.3333333333333333703, 0.3269284268010768657, 0.3333333333333333703, 0.3269284268010768657, 0.3333333333333333703, 0.3269284268010768657, 0.3333333333333333703, 0.3269284268010768657, 0.3333333333333333703, 0.3269284268010768657, 0.3333333333333333703, 0.3269284268010768657, 0.3333333333333333703, 0.3269284268010768657, 0.3333333333333333703, 0.3269284268010768657, 0.3333333333333333703, 0.3269284268010768657, 0.3333333333333333703, 0.3269284268010768657, 0.3333333333333333703, 0.3269284268010768657, 0.3333333333333333703, 0.3269284268010768657, 0.3333333333333333703, 0.3269284268010768657, 0.3333333333333333703, 0.3269284268010768657, 0.3333333333333333703, 0.3269284268010768657, 0.3333333333333333703, 0.3269284268010768657, 0.3333333333333333703, 0.3269284268010768657, 0.3333333333333333703, 0.3269284268010768657, 0.3333333333333333703, 0.3269284268010768657, 0.3333333333333333703, 0.3269284268010768657, 0.3333333333333333703, 0.3269284268010768657, 0.3333333333333333703, 0.3269284268010768657, 0.3333333333333333703, 0.3269284268010768657, 0.3333333333333333703, 0.3269284268010768657, 0.3333333333333333703, 0.3269284268010768657, 0.3333333333333333703, 0.3269284268010768657, 0.3333333333333333703, 0.3269284268010768657, 0.3333333333333333703, 0.3269284268010768657, 0.3333333333333333703, 0.3269284268010768657, 0.3333333333333333703, 0.3269284268010768657, 0.3333333333333333703, 0.3269284268010768657, 0.3333333333333333703, 0.3269284268010768657, 0.3333333333333333703, 0.3269284268010768657, 0.3333333333333333703, 0.3269284268010768657, 0.3333333333333333703, 0.3269284268010768657, 0.3333333333333333703, 0.3269284268010768657, 0.3333333333333333703, 0.3269284268010768657, 0.3333333333333333703, 0.3269284268010768657, 0.3333333333333333703, 0.3269284268010768657, 0.3333333333333333703, 0.3269284268010768657, 0.3333333333333333703, 0.3269284268010768657, 0.3333333333333333703, 0.3269284268010768657, 0.3333333333333333703, 0.3269284268010768657, 0.3333333333333333703, 0.3269284268010768657, 0.3333333333333333703, 0.3269284268010768657, 0.3333333333333333703, 0.3269284268010768657, 0.3333333333333333703, 0.3269284268010768657, 0.3333333333333333703, 0.3269284268010768657, 0.3333333333333333703, 0.3269284268010768657, 0.3333333333333333703, 0.3269284268010768657, 0.3333333333333333703, 0.3269284268010768657, 0.3333333333333333703, 0.3269284268010768657, 0.3333333333333333703),
 ( 0.3333333333333333703, 0.3269284268010768657, 0.3333333333333333703, 0.3269284268010768657, 0.3333333333333333703, 0.3269284268010768657, 0.3333333333333333703, 0.3269284268010768657, 0.3333333333333333703, 0.3269284268010768657, 0.3333333333333333703, 0.3269284268010768657, 0.3333333333333333703, 0.3269284268010768657, 0.3333333333333333703, 0.3269284268010768657, 0.3333333333333333703, 0.3269284268010768657, 0.3333333333333333703, 0.3269284268010768657, 0.3333333333333333703, 0.3269284268010768657, 0.3333333333333333703, 0.3269284268010768657, 0.3333333333333333703, 0.3269284268010768657, 0.3333333333333333703, 0.3269284268010768657, 0.3333333333333333703, 0.3269284268010768657, 0.3333333333333333703, 0.3269284268010768657, 0.3333333333333333703, 0.3269284268010768657, 0.3333333333333333703, 0.3269284268010768657, 0.3333333333333333703, 0.3269284268010768657, 0.3333333333333333703, 0.3269284268010768657, 0.3333333333333333703, 0.3269284268010768657, 0.3333333333333333703, 0.3269284268010768657, 0.3333333333333333703, 0.3269284268010768657, 0.3333333333333333703, 0.3269284268010768657, 0.3333333333333333703, 0.3269284268010768657, 0.3333333333333333703, 0.3269284268010768657, 0.3333333333333333703, 0.3269284268010768657, 0.3333333333333333703, 0.3269284268010768657, 0.3333333333333333703, 0.3269284268010768657, 0.3333333333333333703, 0.3269284268010768657, 0.3333333333333333703, 0.3269284268010768657, 0.3333333333333333703, 0.3269284268010768657, 0.3333333333333333703, 0.3269284268010768657, 0.3333333333333333703, 0.3269284268010768657, 0.3333333333333333703, 0.3269284268010768657, 0.3333333333333333703, 0.3269284268010768657, 0.3333333333333333703, 0.3269284268010768657, 0.3333333333333333703, 0.3269284268010768657, 0.3333333333333333703, 0.3269284268010768657, 0.3333333333333333703, 0.3269284268010768657, 0.3333333333333333703, 0.3269284268010768657, 0.3333333333333333703, 0.3269284268010768657, 0.3333333333333333703, 0.3269284268010768657, 0.3333333333333333703, 0.3269284268010768657, 0.3333333333333333703, 0.3269284268010768657, 0.3333333333333333703, 0.3269284268010768657, 0.3333333333333333703, 0.3269284268010768657, 0.3333333333333333703, 0.3269284268010768657, 0.3333333333333333703, 0.3269284268010768657, 0.3333333333333333703, 0.3269284268010768657, 0.3333333333333333703, 0.3269284268010768657, 0.3333333333333333703, 0.3269284268010768657, 0.3333333333333333703, 0.3269284268010768657, 0.3333333333333333703, 0.3269284268010768657, 0.3333333333333333703, 0.3269284268010768657, 0.3333333333333333703, 0.3269284268010768657, 0.3333333333333333703, 0.3269284268010768657, 0.3333333333333333703, 0.3269284268010768657, 0.3333333333333333703, 0.3269284268010768657, 0.3333333333333333703, 0.3269284268010768657, 0.3333333333333333703, 0.3269284268010768657, 0.3333333333333333703, 0.3269284268010768657, 0.3333333333333333703, 0.3269284268010768657, 0.3333333333333333703, 0.3269284268010768657, 0.3333333333333333703, 0.3269284268010768657, 0.3333333333333333703, 0.3269284268010768657, 0.3333333333333333703, 0.3269284268010768657, 0.3333333333333333703, 0.3269284268010768657, 0.3333333333333333703, 0.3269284268010768657, 0.3333333333333333703, 0.3269284268010768657, 0.3333333333333333703, 0.3269284268010768657, 0.3333333333333333703, 0.3269284268010768657, 0.3333333333333333703, 0.3269284268010768657, 0.3333333333333333703, 0.3269284268010768657, 0.3333333333333333703, 0.3269284268010768657, 0.3333333333333333703, 0.3269284268010768657, 0.3333333333333333703, 0.3269284268010768657, 0.3333333333333333703, 0.3269284268010768657, 0.3333333333333333703, 0.3269284268010768657, 0.3333333333333333703, 0.3269284268010768657, 0.3333333333333333703, 0.3269284268010768657, 0.3333333333333333703, 0.3269284268010768657, 0.3333333333333333703, 0.3269284268010768657, 0.3333333333333333703, 0.3269284268010768657, 0.3333333333333333703, 0.3269284268010768657, 0.3333333333333333703, 0.3269284268010768657, 0.3333333333333333703, 0.3269284268010768657, 0.3333333333333333703, 0.3269284268010768657, 0.3333333333333333703, 0.3269284268010768657, 0.3333333333333333703, 0.3269284268010768657, 0.3333333333333333703, 0.3269284268010768657, 0.3333333333333333703, 0.3269284268010768657, 0.3333333333333333703, 0.3269284268010768657, 0.3333333333333333703, 0.3269284268010768657, 0.3333333333333333703, 0.3269284268010768657, 0.3333333333333333703, 0.3269284268010768657, 0.3333333333333333703, 0.3269284268010768657, 0.3333333333333333703, 0.3269284268010768657, 0.3333333333333333703, 0.3269284268010768657, 0.3333333333333333703, 0.3269284268010768657, 0.3333333333333333703, 0.3269284268010768657, 0.3333333333333333703, 0.3269284268010768657, 0.3333333333333333703, 0.3269284268010768657, 0.3333333333333333703, 0.3269284268010768657, 0.3333333333333333703, 0.3269284268010768657, 0.3333333333333333703, 0.3269284268010768657, 0.3333333333333333703, 0.3269284268010768657, 0.3333333333333333703, 0.3269284268010768657, 0.3333333333333333703, 0.3269284268010768657, 0.3333333333333333703, 0.3269284268010768657, 0.3333333333333333703, 0.3269284268010768657, 0.3333333333333333703, 0.3269284268010768657, 0.3333333333333333703, 0.3269284268010768657, 0.3333333333333333703, 0.3269284268010768657, 0.3333333333333333703, 0.3269284268010768657, 0.3333333333333333703, 0.3269284268010768657, 0.3333333333333333703, 0.3269284268010768657, 0.3333333333333333703, 0.3269284268010768657, 0.3333333333333333703, 0.3269284268010768657, 0.3333333333333333703, 0.3269284268010768657, 0.3333333333333333703, 0.3269284268010768657, 0.3333333333333333703, 0.3269284268010768657, 0.3333333333333333703, 0.3269284268010768657, 0.3333333333333333703, 0.3269284268010768657, 0.3333333333333333703, 0.3269284268010768657, 0.3333333333333333703, 0.3269284268010768657, 0.3333333333333333703, 0.3269284268010768657, 0.3333333333333333703, 0.3269284268010768657, 0.3333333333333333703, 0.3269284268010768657, 0.3333333333333333703, 0.3269284268010768657, 0.3333333333333333703, 0.3269284268010768657, 0.3333333333333333703, 0.3269284268010768657, 0.3333333333333333703, 0.3269284268010768657, 0.3333333333333333703, 0.3269284268010768657, 0.3333333333333333703, 0.3269284268010768657, 0.3333333333333333703, 0.3269284268010768657, 0.3333333333333333703, 0.3269284268010768657, 0.3333333333333333703, 0.3269284268010768657, 0.3333333333333333703, 0.3269284268010768657, 0.3333333333333333703, 0.3269284268010768657, 0.3333333333333333703, 0.3269284268010768657, 0.3333333333333333703, 0.3269284268010768657, 0.3333333333333333703, 0.3269284268010768657, 0.3333333333333333703, 0.3269284268010768657, 0.3333333333333333703, 0.3269284268010768657, 0.3333333333333333703, 0.3269284268010768657, 0.3333333333333333703, 0.3269284268010768657, 0.3333333333333333703, 0.3269284268010768657, 0.3333333333333333703, 0.3269284268010768657, 0.3333333333333333703, 0.3269284268010768657, 0.3333333333333333703, 0.3269284268010768657, 0.3333333333333333703, 0.3269284268010768657, 0.3333333333333333703, 0.3269284268010768657, 0.3333333333333333703, 0.3269284268010768657, 0.3333333333333333703, 0.3269284268010768657, 0.3333333333333333703, 0.3269284268010768657, 0.3333333333333333703, 0.3269284268010768657, 0.3333333333333333703, 0.3269284268010768657, 0.3333333333333333703, 0.3269284268010768657, 0.3333333333333333703, 0.3269284268010768657, 0.3333333333333333703, 0.3269284268010768657, 0.3333333333333333703, 0.3269284268010768657, 0.3333333333333333703, 0.3269284268010768657, 0.3333333333333333703, 0.3269284268010768657, 0.3333333333333333703, 0.3269284268010768657, 0.3333333333333333703, 0.3269284268010768657, 0.3333333333333333703, 0.3269284268010768657, 0.3333333333333333703, 0.3269284268010768657, 0.3333333333333333703, 0.3269284268010768657, 0.3333333333333333703, 0.3269284268010768657, 0.3333333333333333703, 0.3269284268010768657, 0.3333333333333333703, 0.3269284268010768657, 0.3333333333333333703, 0.3269284268010768657, 0.3333333333333333703, 0.3269284268010768657, 0.3333333333333333703, 0.3269284268010768657, 0.3333333333333333703, 0.3269284268010768657, 0.3333333333333333703, 0.3269284268010768657, 0.3333333333333333703, 0.3269284268010768657, 0.3333333333333333703, 0.3269284268010768657, 0.3333333333333333703, 0.3269284268010768657, 0.3333333333333333703, 0.3269284268010768657, 0.3333333333333333703, 0.3269284268010768657, 0.3333333333333333703, 0.3269284268010768657, 0.3333333333333333703, 0.3269284268010768657, 0.3333333333333333703, 0.3269284268010768657, 0.3333333333333333703, 0.3269284268010768657, 0.3333333333333333703, 0.3269284268010768657, 0.3333333333333333703, 0.3269284268010768657, 0.3333333333333333703, 0.3269284268010768657, 0.3333333333333333703, 0.3269284268010768657, 0.3333333333333333703, 0.3269284268010768657, 0.3333333333333333703, 0.3269284268010768657, 0.3333333333333333703, 0.3269284268010768657, 0.3333333333333333703, 0.3269284268010768657, 0.3333333333333333703, 0.3269284268010768657, 0.3333333333333333703, 0.3269284268010768657, 0.3333333333333333703, 0.3269284268010768657, 0.3333333333333333703, 0.3269284268010768657, 0.3333333333333333703, 0.3269284268010768657, 0.3333333333333333703, 0.3269284268010768657, 0.3333333333333333703, 0.3269284268010768657, 0.3333333333333333703, 0.3269284268010768657, 0.3333333333333333703, 0.3269284268010768657, 0.3333333333333333703, 0.3269284268010768657, 0.3333333333333333703, 0.3269284268010768657, 0.3333333333333333703, 0.3269284268010768657, 0.3333333333333333703, 0.3269284268010768657, 0.3333333333333333703, 0.3269284268010768657, 0.3333333333333333703, 0.3269284268010768657, 0.3333333333333333703, 0.3269284268010768657, 0.3333333333333333703, 0.3269284268010768657, 0.3333333333333333703, 0.3269284268010768657, 0.3333333333333333703, 0.3269284268010768657, 0.3333333333333333703, 0.3269284268010768657, 0.3333333333333333703, 0.3269284268010768657, 0.3333333333333333703, 0.3269284268010768657, 0.3333333333333333703, 0.3269284268010768657, 0.3333333333333333703, 0.3269284268010768657, 0.3333333333333333703, 0.3269284268010768657, 0.3333333333333333703, 0.3269284268010768657, 0.3333333333333333703, 0.3269284268010768657, 0.3333333333333333703, 0.3269284268010768657, 0.3333333333333333703, 0.3269284268010768657, 0.3333333333333333703, 0.3269284268010768657, 0.3333333333333333703, 0.3269284268010768657, 0.3333333333333333703, 0.3269284268010768657, 0.3333333333333333703, 0.3269284268010768657, 0.3333333333333333703, 0.3269284268010768657, 0.3333333333333333703, 0.3269284268010768657, 0.3333333333333333703, 0.3269284268010768657, 0.3333333333333333703, 0.3269284268010768657, 0.3333333333333333703, 0.3269284268010768657, 0.3333333333333333703, 0.3269284268010768657, 0.3333333333333333703, 0.3269284268010768657, 0.3333333333333333703, 0.3269284268010768657, 0.3333333333333333703, 0.3269284268010768657, 0.3333333333333333703, 0.3269284268010768657, 0.3333333333333333703, 0.3269284268010768657, 0.3333333333333333703, 0.3269284268010768657, 0.3333333333333333703, 0.3269284268010768657, 0.3333333333333333703),
 ( 1.000000000000000000, 0.9807852804032304306, 1.000000000000000000, 0.9807852804032304306, 1.000000000000000000, 0.9807852804032304306, 1.000000000000000000, 0.9807852804032304306, 1.000000000000000000, 0.9807852804032304306, 1.000000000000000000, 0.9807852804032304306, 1.000000000000000000, 0.9807852804032304306, 1.000000000000000000, 0.9807852804032304306, 1.000000000000000000, 0.9807852804032304306, 1.000000000000000000, 0.9807852804032304306, 1.000000000000000000, 0.9807852804032304306, 1.000000000000000000, 0.9807852804032304306, 1.000000000000000000, 0.9807852804032304306, 1.000000000000000000, 0.9807852804032304306, 1.000000000000000000, 0.9807852804032304306, 1.000000000000000000, 0.9807852804032304306, 1.000000000000000000, 0.9807852804032304306, 1.000000000000000000, 0.9807852804032304306, 1.000000000000000000, 0.9807852804032304306, 1.000000000000000000, 0.9807852804032304306, 1.000000000000000000, 0.9807852804032304306, 1.000000000000000000, 0.9807852804032304306, 1.000000000000000000, 0.9807852804032304306, 1.000000000000000000, 0.9807852804032304306, 1.000000000000000000, 0.9807852804032304306, 1.000000000000000000, 0.9807852804032304306, 1.000000000000000000, 0.9807852804032304306, 1.000000000000000000, 0.9807852804032304306, 1.000000000000000000, 0.9807852804032304306, 1.000000000000000000, 0.9807852804032304306, 1.000000000000000000, 0.9807852804032304306, 1.000000000000000000, 0.9807852804032304306, 1.000000000000000000, 0.9807852804032304306, 1.000000000000000000, 0.9807852804032304306, 1.000000000000000000, 0.9807852804032304306, 1.000000000000000000, 0.9807852804032304306, 1.000000000000000000, 0.9807852804032304306, 1.000000000000000000, 0.9807852804032304306, 1.000000000000000000, 0.9807852804032304306, 1.000000000000000000, 0.9807852804032304306, 1.000000000000000000, 0.9807852804032304306, 1.000000000000000000, 0.9807852804032304306, 1.000000000000000000, 0.9807852804032304306, 1.000000000000000000, 0.9807852804032304306, 1.000000000000000000, 0.9807852804032304306, 1.000000000000000000, 0.9807852804032304306, 1.000000000000000000, 0.9807852804032304306, 1.000000000000000000, 0.9807852804032304306, 1.000000000000000000, 0.9807852804032304306, 1.000000000000000000, 0.9807852804032304306, 1.000000000000000000, 0.9807852804032304306, 1.000000000000000000, 0.9807852804032304306, 1.000000000000000000, 0.9807852804032304306, 1.000000000000000000, 0.9807852804032304306, 1.000000000000000000, 0.9807852804032304306, 1.000000000000000000, 0.9807852804032304306, 1.000000000000000000, 0.9807852804032304306, 1.000000000000000000, 0.9807852804032304306, 1.000000000000000000, 0.9807852804032304306, 1.000000000000000000, 0.9807852804032304306, 1.000000000000000000, 0.9807852804032304306, 1.000000000000000000, 0.9807852804032304306, 1.000000000000000000, 0.9807852804032304306, 1.000000000000000000, 0.9807852804032304306, 1.000000000000000000, 0.9807852804032304306, 1.000000000000000000, 0.9807852804032304306, 1.000000000000000000, 0.9807852804032304306, 1.000000000000000000, 0.9807852804032304306, 1.000000000000000000, 0.9807852804032304306, 1.000000000000000000, 0.9807852804032304306, 1.000000000000000000, 0.9807852804032304306, 1.000000000000000000, 0.9807852804032304306, 1.000000000000000000, 0.9807852804032304306, 1.000000000000000000, 0.9807852804032304306, 1.000000000000000000, 0.9807852804032304306, 1.000000000000000000, 0.9807852804032304306, 1.000000000000000000, 0.9807852804032304306, 1.000000000000000000, 0.9807852804032304306, 1.000000000000000000, 0.9807852804032304306, 1.000000000000000000, 0.9807852804032304306, 1.000000000000000000, 0.9807852804032304306, 1.000000000000000000, 0.9807852804032304306, 1.000000000000000000, 0.9807852804032304306, 1.000000000000000000, 0.9807852804032304306, 1.000000000000000000, 0.9807852804032304306, 1.000000000000000000, 0.9807852804032304306, 1.000000000000000000, 0.9807852804032304306, 1.000000000000000000, 0.9807852804032304306, 1.000000000000000000, 0.9807852804032304306, 1.000000000000000000, 0.9807852804032304306, 1.000000000000000000, 0.9807852804032304306, 1.000000000000000000, 0.9807852804032304306, 1.000000000000000000, 0.9807852804032304306, 1.000000000000000000, 0.9807852804032304306, 1.000000000000000000, 0.9807852804032304306, 1.000000000000000000, 0.9807852804032304306, 1.000000000000000000, 0.9807852804032304306, 1.000000000000000000, 0.9807852804032304306, 1.000000000000000000, 0.9807852804032304306, 1.000000000000000000, 0.9807852804032304306, 1.000000000000000000, 0.9807852804032304306, 1.000000000000000000, 0.9807852804032304306, 1.000000000000000000, 0.9807852804032304306, 1.000000000000000000, 0.9807852804032304306, 1.000000000000000000, 0.9807852804032304306, 1.000000000000000000, 0.9807852804032304306, 1.000000000000000000, 0.9807852804032304306, 1.000000000000000000, 0.9807852804032304306, 1.000000000000000000, 0.9807852804032304306, 1.000000000000000000, 0.9807852804032304306, 1.000000000000000000, 0.9807852804032304306, 1.000000000000000000, 0.9807852804032304306, 1.000000000000000000, 0.9807852804032304306, 1.000000000000000000, 0.9807852804032304306, 1.000000000000000000, 0.9807852804032304306, 1.000000000000000000, 0.9807852804032304306, 1.000000000000000000, 0.9807852804032304306, 1.000000000000000000, 0.9807852804032304306, 1.000000000000000000, 0.9807852804032304306, 1.000000000000000000, 0.9807852804032304306, 1.000000000000000000, 0.9807852804032304306, 1.000000000000000000, 0.9807852804032304306, 1.000000000000000000, 0.9807852804032304306, 1.000000000000000000, 0.9807852804032304306, 1.000000000000000000, 0.9807852804032304306, 1.000000000000000000, 0.9807852804032304306, 1.000000000000000000, 0.9807852804032304306, 1.000000000000000000, 0.9807852804032304306, 1.000000000000000000, 0.9807852804032304306, 1.000000000000000000, 0.9807852804032304306, 1.000000000000000000, 0.9807852804032304306, 1.000000000000000000, 0.9807852804032304306, 1.000000000000000000, 0.9807852804032304306, 1.000000000000000000, 0.9807852804032304306, 1.000000000000000000, 0.9807852804032304306, 1.000000000000000000, 0.9807852804032304306, 1.000000000000000000, 0.9807852804032304306, 1.000000000000000000, 0.9807852804032304306, 1.000000000000000000, 0.9807852804032304306, 1.000000000000000000, 0.9807852804032304306, 1.000000000000000000, 0.9807852804032304306, 1.000000000000000000, 0.9807852804032304306, 1.000000000000000000, 0.9807852804032304306, 1.000000000000000000, 0.9807852804032304306, 1.000000000000000000, 0.9807852804032304306, 1.000000000000000000, 0.9807852804032304306, 1.000000000000000000, 0.9807852804032304306, 1.000000000000000000, 0.9807852804032304306, 1.000000000000000000, 0.9807852804032304306, 1.000000000000000000, 0.9807852804032304306, 1.000000000000000000, 0.9807852804032304306, 1.000000000000000000, 0.9807852804032304306, 1.000000000000000000, 0.9807852804032304306, 1.000000000000000000, 0.9807852804032304306, 1.000000000000000000, 0.9807852804032304306, 1.000000000000000000, 0.9807852804032304306, 1.000000000000000000, 0.9807852804032304306, 1.000000000000000000, 0.9807852804032304306, 1.000000000000000000, 0.9807852804032304306, 1.000000000000000000, 0.9807852804032304306, 1.000000000000000000, 0.9807852804032304306, 1.000000000000000000, 0.9807852804032304306, 1.000000000000000000, 0.9807852804032304306, 1.000000000000000000, 0.9807852804032304306, 1.000000000000000000, 0.9807852804032304306, 1.000000000000000000, 0.9807852804032304306, 1.000000000000000000, 0.9807852804032304306, 1.000000000000000000, 0.9807852804032304306, 1.000000000000000000, 0.9807852804032304306, 1.000000000000000000, 0.9807852804032304306, 1.000000000000000000, 0.9807852804032304306, 1.000000000000000000, 0.9807852804032304306, 1.000000000000000000, 0.9807852804032304306, 1.000000000000000000, 0.9807852804032304306, 1.000000000000000000, 0.9807852804032304306, 1.000000000000000000, 0.9807852804032304306, 1.000000000000000000, 0.9807852804032304306, 1.000000000000000000, 0.9807852804032304306, 1.000000000000000000, 0.9807852804032304306, 1.000000000000000000, 0.9807852804032304306, 1.000000000000000000, 0.9807852804032304306, 1.000000000000000000, 0.9807852804032304306, 1.000000000000000000, 0.9807852804032304306, 1.000000000000000000, 0.9807852804032304306, 1.000000000000000000, 0.9807852804032304306, 1.000000000000000000, 0.9807852804032304306, 1.000000000000000000, 0.9807852804032304306, 1.000000000000000000, 0.9807852804032304306, 1.000000000000000000, 0.9807852804032304306, 1.000000000000000000, 0.9807852804032304306, 1.000000000000000000, 0.9807852804032304306, 1.000000000000000000, 0.9807852804032304306, 1.000000000000000000, 0.9807852804032304306, 1.000000000000000000, 0.9807852804032304306, 1.000000000000000000, 0.9807852804032304306, 1.000000000000000000, 0.9807852804032304306, 1.000000000000000000, 0.9807852804032304306, 1.000000000000000000, 0.9807852804032304306, 1.000000000000000000, 0.9807852804032304306, 1.000000000000000000, 0.9807852804032304306, 1.000000000000000000, 0.9807852804032304306, 1.000000000000000000, 0.9807852804032304306, 1.000000000000000000, 0.9807852804032304306, 1.000000000000000000, 0.9807852804032304306, 1.000000000000000000, 0.9807852804032304306, 1.000000000000000000, 0.9807852804032304306, 1.000000000000000000, 0.9807852804032304306, 1.000000000000000000, 0.9807852804032304306, 1.000000000000000000, 0.9807852804032304306, 1.000000000000000000, 0.9807852804032304306, 1.000000000000000000, 0.9807852804032304306, 1.000000000000000000, 0.9807852804032304306, 1.000000000000000000, 0.9807852804032304306, 1.000000000000000000, 0.9807852804032304306, 1.000000000000000000, 0.9807852804032304306, 1.000000000000000000, 0.9807852804032304306, 1.000000000000000000, 0.9807852804032304306, 1.000000000000000000, 0.9807852804032304306, 1.000000000000000000, 0.9807852804032304306, 1.000000000000000000, 0.9807852804032304306, 1.000000000000000000, 0.9807852804032304306, 1.000000000000000000, 0.9807852804032304306, 1.000000000000000000, 0.9807852804032304306, 1.000000000000000000, 0.9807852804032304306, 1.000000000000000000, 0.9807852804032304306, 1.000000000000000000, 0.9807852804032304306, 1.000000000000000000, 0.9807852804032304306, 1.000000000000000000, 0.9807852804032304306, 1.000000000000000000, 0.9807852804032304306, 1.000000000000000000, 0.9807852804032304306, 1.000000000000000000, 0.9807852804032304306, 1.000000000000000000, 0.9807852804032304306, 1.000000000000000000, 0.9807852804032304306, 1.000000000000000000, 0.9807852804032304306, 1.000000000000000000, 0.9807852804032304306, 1.000000000000000000, 0.9807852804032304306, 1.000000000000000000, 0.9807852804032304306, 1.000000000000000000, 0.9807852804032304306, 1.000000000000000000, 0.9807852804032304306, 1.000000000000000000, 0.9807852804032304306, 1.000000000000000000) ) ) 
 REPRESENTATION_ITEM ( '' )  SURFACE ( )  );
#27454 = AXIS2_PLACEMENT_3D ( 'NONE', #35671, #3649, #24128 ) ;
#27455 = CARTESIAN_POINT ( 'NONE',  ( -55.14955436395491262, 213.3788001182225003, -3.209657149897400252 ) ) ;
#27456 = FACE_BOUND ( 'NONE', #20968, .T. ) ;
#27457 = CARTESIAN_POINT ( 'NONE',  ( 8.843639120294245259, 48.46481371789856496, 3.474262827703527901 ) ) ;
#27458 = CARTESIAN_POINT ( 'NONE',  ( 22.80587116629410716, 3.604726614523238837, -8.878124999385546445 ) ) ;
#27459 = CARTESIAN_POINT ( 'NONE',  ( -9.465287035748106703, 107.4023137178985650, 2.064181346179061460 ) ) ;
#27460 = CARTESIAN_POINT ( 'NONE',  ( 21.00000000000000355, 0.000000000000000000, 50.00000000000001421 ) ) ;
#27461 = CARTESIAN_POINT ( 'NONE',  ( 12.50000000000000355, 29.48981371789854933, -0.1745138560722771515 ) ) ;
#27462 =( GEOMETRIC_REPRESENTATION_CONTEXT ( 3 ) GLOBAL_UNCERTAINTY_ASSIGNED_CONTEXT ( ( #27144 ) ) GLOBAL_UNIT_ASSIGNED_CONTEXT ( ( #6853, #21275, #3811 ) ) REPRESENTATION_CONTEXT ( 'NONE', 'WORKASPACE' ) );
#27463 = CARTESIAN_POINT ( 'NONE',  ( -10.69584247140444866, 85.44768628210144357, 6.932735513423972762 ) ) ;
#27464 = CARTESIAN_POINT ( 'NONE',  ( 19.56230152254410370, 5.196152422706631135, -8.137499998771001941 ) ) ;
#27465 = CIRCLE ( 'NONE', #17785, 3.999999999999996447 ) ;
#27466 = CARTESIAN_POINT ( 'NONE',  ( 0.000000000000000000, 143.0000000000000000, 0.000000000000000000 ) ) ;
#27467 = CARTESIAN_POINT ( 'NONE',  ( 24.55661210480496948, 3.604726614523236616, 162.2891901003200132 ) ) ;
#27468 = CARTESIAN_POINT ( 'NONE',  ( 19.68408634441912142, -5.407089921784861808, -3.196874999385534988 ) ) ;
#27469 = DIRECTION ( 'NONE',  ( 1.000000000000000000, 0.000000000000000000, 0.000000000000000000 ) ) ;
#27470 = CARTESIAN_POINT ( 'NONE',  ( 20.99999999999999645, 185.0294372515228645, 5.999999999999999112 ) ) ;
#27471 = EDGE_CURVE ( 'NONE', #15328, #30939, #10260, .T. ) ;
#27472 = CARTESIAN_POINT ( 'NONE',  ( 0.000000000000000000, 200.0000000000000000, -27.00000000000000355 ) ) ;
#27473 = CARTESIAN_POINT ( 'NONE',  ( 0.1745138560725194299, 88.61018628210146630, -9.500000000000005329 ) ) ;
#27474 = CARTESIAN_POINT ( 'NONE',  ( 10.49813415415989581, 137.7726862821014606, 7.228626920339068285 ) ) ;
#27475 = CARTESIAN_POINT ( 'NONE',  ( 22.56230152254319421, 3.464101615138294843, -4.687500000000025757 ) ) ;
#27476 = CARTESIAN_POINT ( 'NONE',  ( 18.12178482187500350, 240.3718750006145228, 4.985214923628407568 ) ) ;
#27477 = VERTEX_POINT ( 'NONE', #27324 ) ;
#27478 = CARTESIAN_POINT ( 'NONE',  ( 30.92676673731498482, 7.209453229046475009, 163.4634630048305439 ) ) ;
#27479 = CARTESIAN_POINT ( 'NONE',  ( 26.75643035624999655, 3.323476615752271712, -2.128124999385482052 ) ) ;
#27481 = ADVANCED_FACE ( 'NONE', ( #1352 ), #27699, .T. ) ;
#27480 = CARTESIAN_POINT ( 'NONE',  ( 13.62178482187499640, 198.8093750006145513, -23.59362340125807123 ) ) ;
#27482 = CARTESIAN_POINT ( 'NONE',  ( 34.42112650116913386, -5.196152422706635576, 168.9830381333390505 ) ) ;
#27483 = LINE ( 'NONE', #5102, #24107 ) ;
#27484 = CARTESIAN_POINT ( 'NONE',  ( 26.75643035624999655, 242.9218750006145626, -3.323476615752271712 ) ) ;
#27485 = CARTESIAN_POINT ( 'NONE',  ( 16.56230152254411436, -7.209453229046475009, -0.9281249993855145153 ) ) ;
#27486 = CARTESIAN_POINT ( 'NONE',  ( -9.500000000000005329, 6.489813717898557321, 0.1745138560723101806 ) ) ;
#27487 = CARTESIAN_POINT ( 'NONE',  ( -13.62178482187500528, 196.6343750006145399, -23.59362340125807123 ) ) ;
#27489 = ORIENTED_EDGE ( 'NONE', *, *, #32635, .F. ) ;
#27488 = ORIENTED_EDGE ( 'NONE', *, *, #14751, .T. ) ;
#27490 = VECTOR ( 'NONE', #9582, 1000.000000000000000 ) ;
#27491 =( BOUNDED_CURVE ( )  B_SPLINE_CURVE ( 2, ( #19810, #31345, #37389, #2713, #16951, #25655, #11255, #34557, #22825 ),
 .UNSPECIFIED., .F., .F. ) 
 B_SPLINE_CURVE_WITH_KNOTS ( ( 3, 2, 2, 2, 3 ),
 ( 0.7291666666666667407, 0.7361111111111111605, 0.7500000000000000000, 0.7638888888888888395, 0.7708333333333333703 ),
 .UNSPECIFIED. ) 
 CURVE ( )  GEOMETRIC_REPRESENTATION_ITEM ( )  RATIONAL_B_SPLINE_CURVE ( ( 0.9330127018922192983, 0.9330127018922198534, 1.000000000000000000, 0.8660254037844387076, 1.000000000000000000, 0.8660254037844387076, 1.000000000000000000, 0.9330127018922187432, 0.9330127018922192983 ) ) 
 REPRESENTATION_ITEM ( '' )  );
#27492 = AXIS2_PLACEMENT_3D ( 'NONE', #29501, #12066, #26467 ) ;
#27493 = CARTESIAN_POINT ( 'NONE',  ( 15.24356964374999990, 247.9468750006145115, 0.000000000000000000 ) ) ;
#27494 = ADVANCED_FACE ( 'NONE', ( #9887 ), #33010, .T. ) ;
#27495 = CARTESIAN_POINT ( 'NONE',  ( 12.50000000000000355, 29.48981371789854933, -0.1745138560722771515 ) ) ;
#27496 = VECTOR ( 'NONE', #1810, 1000.000000000000000 ) ;
#27497 = CARTESIAN_POINT ( 'NONE',  ( 23.87821517812500005, -4.985214923628404016, -3.140624999385472016 ) ) ;
#27498 = CARTESIAN_POINT ( 'NONE',  ( 8.927990412390371944, 122.9273137178985422, 13.04141134922778811 ) ) ;
#27499 = PRESENTATION_LAYER_ASSIGNMENT (  '', '', ( #1459 ) ) ;
#27500 = CARTESIAN_POINT ( 'NONE',  ( 24.00000000000000000, -5.196152422706629359, -9.693749998770956111 ) ) ;
#27501 = ORIENTED_EDGE ( 'NONE', *, *, #9725, .T. ) ;
#27502 = CARTESIAN_POINT ( 'NONE',  ( 13.44051670066911441, -5.407089921784865361, -6.871874999385546801 ) ) ;
#27503 = ORIENTED_EDGE ( 'NONE', *, *, #10396, .F. ) ;
#27504 = CARTESIAN_POINT ( 'NONE',  ( 13.62178482187501416, 197.2531250006145456, 23.59362340125806767 ) ) ;
#27505 = CARTESIAN_POINT ( 'NONE',  ( 12.53471296425194836, 127.4226862821014663, -2.311890736173178418 ) ) ;
#27506 = CARTESIAN_POINT ( 'NONE',  ( 24.47326942580252407, 3.604726614523240613, 161.3365789202697727 ) ) ;
#27507 = CARTESIAN_POINT ( 'NONE',  ( -55.14211230271182984, 201.5309553116392181, 2.393094931466368980 ) ) ;
#27508 = CARTESIAN_POINT ( 'NONE',  ( 20.99999999999999645, 246.4843750006145058, -6.646953231504538984 ) ) ;
#27509 = PRESENTATION_STYLE_ASSIGNMENT (( #4378 ) ) ;
#27510 = PLANE ( 'NONE',  #35781 ) ;
#27511 = CARTESIAN_POINT ( 'NONE',  ( -50.98586230271183695, 207.8500491399821613, 3.954877714930852495 ) ) ;
#27512 = CARTESIAN_POINT ( 'NONE',  ( 19.39230484541326049, 245.8575961894323427, -5.999999999999997335 ) ) ;
#27513 = CARTESIAN_POINT ( 'NONE',  ( 13.44051670066910731, 5.407089921784862696, -10.17187499938551554 ) ) ;
#27514 = EDGE_LOOP ( 'NONE', ( #36083, #36154, #13109, #15700 ) ) ;
#27515 = LINE ( 'NONE', #18630, #381 ) ;
#27516 = CARTESIAN_POINT ( 'NONE',  ( 8.927990412390657937, 126.2726862821014464, -13.04141134922759804 ) ) ;
#27517 = CARTESIAN_POINT ( 'NONE',  ( -48.42038769728824832, 207.6069050685337913, 8.469044688360781947 ) ) ;
#27518 = CARTESIAN_POINT ( 'NONE',  ( -3.796722387233375073, 112.1851862821014691, 8.710071997420127943 ) ) ;
#27519 = ADVANCED_FACE ( 'NONE', ( #36403 ), #4384, .T. ) ;
#27520 = CARTESIAN_POINT ( 'NONE',  ( -8.715434833791929847, 13.86018628210145032, -8.962234695871762469 ) ) ;
#27521 = CARTESIAN_POINT ( 'NONE',  ( 22.56230152254412147, 3.464101615137759271, -9.187500000000026645 ) ) ;
#27522 = VERTEX_POINT ( 'NONE', #7059 ) ;
#27523 = DIRECTION ( 'NONE',  ( 1.000000000000000000, 0.000000000000000000, 0.000000000000000000 ) ) ;
#27524 = CARTESIAN_POINT ( 'NONE',  ( 6.594114490232313663, 82.86018628210146630, 6.840914352312096547 ) ) ;
#27525 = FILL_AREA_STYLE_COLOUR ( '', #27881 ) ;
#27526 = CARTESIAN_POINT ( 'NONE',  ( 1.715153634034445762, 128.6773137178985280, -9.534712964251895073 ) ) ;
#27527 = CARTESIAN_POINT ( 'NONE',  ( 27.24356964375000700, 198.6406250006145058, 15.72908226750537075 ) ) ;
#27528 = FACE_OUTER_BOUND ( 'NONE', #7600, .T. ) ;
#27529 = CARTESIAN_POINT ( 'NONE',  ( 13.62178482187501416, 197.3093750006145513, 23.59362340125806767 ) ) ;
#27530 = CARTESIAN_POINT ( 'NONE',  ( 15.00000000000000000, 250.0000000000000000, 0.000000000000000000 ) ) ;
#27531 = CARTESIAN_POINT ( 'NONE',  ( 10.56230152254410726, 0.000000000000000000, -3.600000000000047606 ) ) ;
#27532 = CARTESIAN_POINT ( 'NONE',  ( -9.534712964251895073, 80.37731371789853085, -1.715153634034446428 ) ) ;
#27533 = ORIENTED_EDGE ( 'NONE', *, *, #26302, .T. ) ;
#27534 = CARTESIAN_POINT ( 'NONE',  ( 15.00000000000000000, 244.6562500012290400, 0.000000000000000000 ) ) ;
#27535 = CARTESIAN_POINT ( 'NONE',  ( -0.1745138560722763466, 82.38981371789854791, -12.50000000000000355 ) ) ;
#27536 = CARTESIAN_POINT ( 'NONE',  ( 19.68408634441911076, 5.407089921784862696, -3.496874999385557459 ) ) ;
#27537 = CARTESIAN_POINT ( 'NONE',  ( 20.99999999999995381, 242.9124999999999943, 5.999999999999998224 ) ) ;
#27538 = CARTESIAN_POINT ( 'NONE',  ( 23.87821517812500005, -4.985214923628404016, -5.053124999385483207 ) ) ;
#27539 = CARTESIAN_POINT ( 'NONE',  ( -10.69584247140429412, 44.15231371789854364, -6.932735513424201024 ) ) ;
#27540 = ORIENTED_EDGE ( 'NONE', *, *, #30260, .T. ) ;
#27541 = CARTESIAN_POINT ( 'NONE',  ( 15.24356964374999990, 0.000000000000000000, -6.440624999385469174 ) ) ;
#27542 = CARTESIAN_POINT ( 'NONE',  ( 18.12178482187499640, 243.8218750006145399, -4.985214923628404904 ) ) ;
#27543 = CARTESIAN_POINT ( 'NONE',  ( -11.61527771782819940, 30.53518628210144570, 4.622313124798574258 ) ) ;
#27544 = VECTOR ( 'NONE', #30891, 1000.000000000000114 ) ;
#27545 = CARTESIAN_POINT ( 'NONE',  ( -37.13169563604516554, 210.1155267958017703, 6.500000000000000888 ) ) ;
#27546 = CARTESIAN_POINT ( 'NONE',  ( -58.90252896937850124, 206.6499508600178387, -5.571401726697954970 ) ) ;
#27547 = CARTESIAN_POINT ( 'NONE',  ( 24.67097253372167387, -3.464101615137757051, 160.8016875364665736 ) ) ;
#27548 = CARTESIAN_POINT ( 'NONE',  ( -12.50000000000000355, 70.88981371789856212, 0.1745138560722786503 ) ) ;
#27549 = CARTESIAN_POINT ( 'NONE',  ( -47.03497103062157692, 206.1606490808709111, -2.350049139982163027 ) ) ;
#27550 = EDGE_CURVE ( 'NONE', #2357, #26075, #27515, .T. ) ;
#27551 = CARTESIAN_POINT ( 'NONE',  ( -60.09747103062156981, 213.3500491399821328, -5.571401726697985168 ) ) ;
#27552 = FACE_OUTER_BOUND ( 'NONE', #9078, .T. ) ;
#27553 = CARTESIAN_POINT ( 'NONE',  ( -14.50000000000000533, 252.0000000000000000, 2.500000000000000000 ) ) ;
#27554 = CARTESIAN_POINT ( 'NONE',  ( -2.908627838312453306, 32.07731371789855501, 15.53471296425188797 ) ) ;
#27555 = EDGE_CURVE ( 'NONE', #18752, #11631, #10447, .T. ) ;
#27556 = CARTESIAN_POINT ( 'NONE',  ( -41.48586230271182984, 205.8500491399821613, 7.418979330068642852 ) ) ;
#27557 = CARTESIAN_POINT ( 'NONE',  ( -27.00000000000000355, 198.2000000000000171, 0.000000000000000000 ) ) ;
#27558 = CARTESIAN_POINT ( 'NONE',  ( -4.944772684328673229, 75.38518628210144357, 11.48171059495397728 ) ) ;
#27559 = ADVANCED_FACE ( 'NONE', ( #33761 ), #8357, .T. ) ;
#27560 = CARTESIAN_POINT ( 'NONE',  ( -10.83675517735155047, 32.26018628210145067, -11.08355503943142750 ) ) ;
#27561 = CARTESIAN_POINT ( 'NONE',  ( -3.253724281355068545E-15, 197.3000000012290229, -27.00000000000000000 ) ) ;
#27562 = ORIENTED_EDGE ( 'NONE', *, *, #5692, .F. ) ;
#27563 = CARTESIAN_POINT ( 'NONE',  ( -0.1745138560725817967, 38.01018628210144357, 15.50000000000000533 ) ) ;
#27564 = CARTESIAN_POINT ( 'NONE',  ( -13.62178482187500528, 196.5781250006145342, -23.59362340125807123 ) ) ;
#27565 = CARTESIAN_POINT ( 'NONE',  ( 16.56230152254411081, -6.928203230275506996, -0.6749999987709801585 ) ) ;
#27566 = CYLINDRICAL_SURFACE ( 'NONE', #7480, 27.00000000000000355 ) ;
#27567 = CARTESIAN_POINT ( 'NONE',  ( -33.37872103062156981, 203.4690446883607535, 1.626142955000567936 ) ) ;
#27568 = CARTESIAN_POINT ( 'NONE',  ( 26.99999999999999645, 196.3250000012290570, -15.58845726811990495 ) ) ;
#27569 = CIRCLE ( 'NONE', #12416, 5.000000000000000888 ) ;
#27570 = CARTESIAN_POINT ( 'NONE',  ( 10.56230152254410726, 0.000000000000000000, -8.887499998771003717 ) ) ;
#27571 = CARTESIAN_POINT ( 'NONE',  ( -5.529263428287297444, 127.5273137178985792, -7.954856959092311719 ) ) ;
#27572 = CARTESIAN_POINT ( 'NONE',  ( 15.24356964375000167, 244.4968750006145513, 3.323476615752272600 ) ) ;
#27573 = VERTEX_POINT ( 'NONE', #2469 ) ;
#27574 = CYLINDRICAL_SURFACE ( 'NONE', #20844, 6.000000000000001776 ) ;
#27575 = LINE ( 'NONE', #32558, #13239 ) ;
#27576 = CARTESIAN_POINT ( 'NONE',  ( 4.622313124798831829, 138.1648137178985678, -11.61527771782809282 ) ) ;
#27577 = CARTESIAN_POINT ( 'NONE',  ( 16.56230152254411436, 7.209453229046475009, -7.003124999385537564 ) ) ;
#27578 = CARTESIAN_POINT ( 'NONE',  ( 34.02033052368495447, -5.407089921784855591, 163.0045950240894967 ) ) ;
#27579 = CARTESIAN_POINT ( 'NONE',  ( 19.95811783012620566, 240.0005235271234483, -5.908847734042487865 ) ) ;
#27580 = CARTESIAN_POINT ( 'NONE',  ( 5.727106289114498080E-15, 198.7625000000000455, 31.17691453623979214 ) ) ;
#27581 = ORIENTED_EDGE ( 'NONE', *, *, #18191, .F. ) ;
#27582 = CARTESIAN_POINT ( 'NONE',  ( 12.50000000000000355, 35.71018628210144641, 0.1745138560725507937 ) ) ;
#27583 = ORIENTED_EDGE ( 'NONE', *, *, #10140, .T. ) ;
#27584 = ORIENTED_EDGE ( 'NONE', *, *, #18763, .F. ) ;
#27585 = CARTESIAN_POINT ( 'NONE',  ( 23.99999999999999645, 5.196152422706631135, -4.593749998770962684 ) ) ;
#27586 = CARTESIAN_POINT ( 'NONE',  ( 26.75643035624999655, 3.323476615752271268, -1.228124999385458160 ) ) ;
#27587 = CARTESIAN_POINT ( 'NONE',  ( 16.56230152254411436, -6.928203230275514990, -9.337500000000018119 ) ) ;
#27588 = CARTESIAN_POINT ( 'NONE',  ( -27.00000000000000355, 196.4000000000000057, 0.000000000000000000 ) ) ;
#27589 = CARTESIAN_POINT ( 'NONE',  ( 18.12178482187500350, -4.985214923628407568, -8.165624999385473259 ) ) ;
#27590 = CARTESIAN_POINT ( 'NONE',  ( 6.932735513423970097, 83.14768628210144641, 10.69584247140445044 ) ) ;
#27591 = CARTESIAN_POINT ( 'NONE',  ( -0.1745138560722442889, 8.789813717898553591, -15.50000000000000533 ) ) ;
#27592 = CARTESIAN_POINT ( 'NONE',  ( 33.76419009031582874, -5.196152422706629359, 161.4742205976968989 ) ) ;
#27593 = CARTESIAN_POINT ( 'NONE',  ( 17.99309595496610470, 218.0184107867572720, 5.206989594055762893 ) ) ;
#27594 = CARTESIAN_POINT ( 'NONE',  ( -54.74627896937850835, 205.4690446883607535, -1.090244570138286351 ) ) ;
#27595 = CARTESIAN_POINT ( 'NONE',  ( 37.14824336730853105, -3.464101615137751278, 165.7329868120451977 ) ) ;
#27596 = CARTESIAN_POINT ( 'NONE',  ( -10.49813415416004858, 125.2273137178985820, 7.228626920338839135 ) ) ;
#27597 = CARTESIAN_POINT ( 'NONE',  ( -51.78497103062156981, 204.4285982733020148, -3.350049139982115509 ) ) ;
#27598 = CARTESIAN_POINT ( 'NONE',  ( -51.78497103062156981, 202.6965474657331185, -4.350049139982091084 ) ) ;
#27599 = AXIS2_PLACEMENT_3D ( 'NONE', #8181, #31658, #11198 ) ;
#27600 = APPLICATION_PROTOCOL_DEFINITION ( 'draft international standard', 'automotive_design', 1998, #14628 ) ;
#27601 = CARTESIAN_POINT ( 'NONE',  ( 23.87821517812500005, -4.985214923628404016, -1.903124999385497063 ) ) ;
#27602 = CARTESIAN_POINT ( 'NONE',  ( -1.926257025242585782E-15, 196.5406250006145399, -31.45816453501075927 ) ) ;
#27603 = CARTESIAN_POINT ( 'NONE',  ( -15.50000000000000533, 107.6898137178985735, 0.1745138560722471477 ) ) ;
#27604 = CARTESIAN_POINT ( 'NONE',  ( -49.20461230271183695, 208.1428034533959135, -6.469044688360754414 ) ) ;
#27605 = ORIENTED_EDGE ( 'NONE', *, *, #16987, .T. ) ;
#27606 = CARTESIAN_POINT ( 'NONE',  ( -13.49999999999998401, 196.1375000012290286, 23.38268590217985476 ) ) ;
#27607 = CARTESIAN_POINT ( 'NONE',  ( -2.311890736173176641, 125.1226862821014549, -12.53471296425194836 ) ) ;
#27608 = CARTESIAN_POINT ( 'NONE',  ( -2.908627838312119351, 79.12268628210145494, -15.53471296425195369 ) ) ;
#27609 = CARTESIAN_POINT ( 'NONE',  ( 0.000000000000000000, 200.0000000000000000, 0.000000000000000000 ) ) ;
#27610 = CARTESIAN_POINT ( 'NONE',  ( 34.14616162727688931, 5.407089921784862696, 164.4428511194594478 ) ) ;
#27611 = CARTESIAN_POINT ( 'NONE',  ( -15.53471296425195369, 76.82268628210144357, 2.908627838312118019 ) ) ;
#27612 = CIRCLE ( 'NONE', #25208, 3.999999999999996447 ) ;
#27613 = CARTESIAN_POINT ( 'NONE',  ( -61.28497103062156981, 204.4285982733020148, -3.350049139982115509 ) ) ;
#27614 = CARTESIAN_POINT ( 'NONE',  ( 13.44051670066911797, -5.407089921784859143, -4.115624999385558702 ) ) ;
#27615 = CARTESIAN_POINT ( 'NONE',  ( -8.843639120294326972, 48.93518628210144072, 3.474262827703335166 ) ) ;
#27616 = CARTESIAN_POINT ( 'NONE',  ( 6.000000000000000000, -30.00000000000000000, 20.00000000000000000 ) ) ;
#27617 = CARTESIAN_POINT ( 'NONE',  ( -41.88913769728823411, 205.8500491399820760, -7.418979330068584233 ) ) ;
#27618 = CARTESIAN_POINT ( 'NONE',  ( 20.99999999999999645, 250.0000000000000000, 0.000000000000000000 ) ) ;
#27619 = EDGE_CURVE ( 'NONE', #3985, #253, #37148, .T. ) ;
#27620 = CARTESIAN_POINT ( 'NONE',  ( -12.46528703574805697, 68.19768628210144357, -2.660918448318280838 ) ) ;
#27621 = LINE ( 'NONE', #13405, #11817 ) ;
#27622 = CARTESIAN_POINT ( 'NONE',  ( 13.50000000000001421, 199.2500000000000000, 23.38268590217984055 ) ) ;
#27624 = CARTESIAN_POINT ( 'NONE',  ( 10.31873187879410381, 3.604726614523240613, -1.134374999385481697 ) ) ;
#27623 = CARTESIAN_POINT ( 'NONE',  ( 3.474262827703335166, 37.43518628210144072, 8.843639120294326972 ) ) ;
#27625 = DIRECTION ( 'NONE',  ( 0.000000000000000000, 0.000000000000000000, -1.000000000000000000 ) ) ;
#27626 = ORIENTED_EDGE ( 'NONE', *, *, #1145, .F. ) ;
#27627 = CARTESIAN_POINT ( 'NONE',  ( 15.00000000000000000, 3.464101615137752166, -3.187499999999998668 ) ) ;
#27628 = CARTESIAN_POINT ( 'NONE',  ( 37.13187018199665346, 7.646167579472024665E-16, 162.7511921998298590 ) ) ;
#27629 = CARTESIAN_POINT ( 'NONE',  ( 30.68409246604844043, -6.928203230275514990, 160.6896833917191714 ) ) ;
#27630 = CARTESIAN_POINT ( 'NONE',  ( 18.00000000000000355, 246.4749999999999943, 5.196152422706632912 ) ) ;
#27631 = CARTESIAN_POINT ( 'NONE',  ( 2.999999999999997335, 244.5000000000000000, -10.00000000000000000 ) ) ;
#27632 = CIRCLE ( 'NONE', #8260, 4.899999999999999467 ) ;
#27633 = CARTESIAN_POINT ( 'NONE',  ( 0.1745138560722779009, 86.98981371789855643, 12.50000000000000355 ) ) ;
#27634 = CARTESIAN_POINT ( 'NONE',  ( -10.49813415415989404, 77.97268628210144925, -7.228626920339069173 ) ) ;
#27635 = ORIENTED_EDGE ( 'NONE', *, *, #28917, .T. ) ;
#27636 = EDGE_LOOP ( 'NONE', ( #26728, #28539, #19444, #11230 ) ) ;
#27637 = CARTESIAN_POINT ( 'NONE',  ( -13.49999999999998401, 198.8375000012290457, 23.38268590217985476 ) ) ;
#27638 = CARTESIAN_POINT ( 'NONE',  ( 20.99999999999999645, -6.928203230275506996, -3.937500000000003109 ) ) ;
#27639 = CARTESIAN_POINT ( 'NONE',  ( -13.23911966647199812, 53.35231371789856780, -8.632099005475788900 ) ) ;
#27640 = ADVANCED_FACE ( 'NONE', ( #11189 ), #10821, .T. ) ;
#27641 = CARTESIAN_POINT ( 'NONE',  ( 26.75643035624999655, -3.323476615752267715, -7.265624999385483562 ) ) ;
#27642 = CARTESIAN_POINT ( 'NONE',  ( 26.75643035624999655, 245.9968750006145513, 3.323476615752267715 ) ) ;
#27643 = ADVANCED_FACE ( 'NONE', ( #22764 ), #19929, .F. ) ;
#27644 = CARTESIAN_POINT ( 'NONE',  ( -50.59747103062156981, 212.3500491399821613, -3.839350919129076445 ) ) ;
#27645 = AXIS2_PLACEMENT_3D ( 'NONE', #125, #5813, #495 ) ;
#27646 = DIRECTION ( 'NONE',  ( -0.000000000000000000, -0.000000000000000000, 1.000000000000000000 ) ) ;
#27647 = CARTESIAN_POINT ( 'NONE',  ( -0.1745138560723084320, 63.98981371789855643, -9.500000000000005329 ) ) ;
#27648 = CARTESIAN_POINT ( 'NONE',  ( 22.80587116629410360, -3.604726614523235284, -8.953124999385538629 ) ) ;
#27649 = CARTESIAN_POINT ( 'NONE',  ( 9.500000000000005329, 93.88981371789856212, -0.1745138560723090149 ) ) ;
#27650 = CARTESIAN_POINT ( 'NONE',  ( 15.24356964374999990, 239.8093750006145228, -3.323476615752268604 ) ) ;
#27651 = CARTESIAN_POINT ( 'NONE',  ( 6.932735513424201024, 37.25231371789855217, -10.69584247140429412 ) ) ;
#27652 =( BOUNDED_CURVE ( )  B_SPLINE_CURVE ( 2, ( #32554, #3745, #23854, #12088, #6784, #15511, #15319, #3936, #24040 ),
 .UNSPECIFIED., .F., .F. ) 
 B_SPLINE_CURVE_WITH_KNOTS ( ( 3, 2, 2, 2, 3 ),
 ( 0.2291666666666666574, 0.2361111111111111049, 0.2500000000000000000, 0.2638888888888888951, 0.2708333333333333703 ),
 .UNSPECIFIED. ) 
 CURVE ( )  GEOMETRIC_REPRESENTATION_ITEM ( )  RATIONAL_B_SPLINE_CURVE ( ( 0.9330127018922194093, 0.9330127018922194093, 1.000000000000000000, 0.8660254037844387076, 1.000000000000000000, 0.8660254037844387076, 1.000000000000000000, 0.9330127018922190762, 0.9330127018922194093 ) ) 
 REPRESENTATION_ITEM ( '' )  );
#27653 = CARTESIAN_POINT ( 'NONE',  ( -10.69584247140444866, 76.24768628210144072, 6.932735513423972762 ) ) ;
#27654 = CARTESIAN_POINT ( 'NONE',  ( 19.56230152254410370, 5.196152422706631135, -9.037499998771014731 ) ) ;
#27655 = DIRECTION ( 'NONE',  ( -0.000000000000000000, 1.000000000000000000, -0.000000000000000000 ) ) ;
#27656 = CARTESIAN_POINT ( 'NONE',  ( 37.05506418370026722, -3.604726614523235284, 161.8732956221364532 ) ) ;
#27657 = CARTESIAN_POINT ( 'NONE',  ( 13.44051670066911441, -5.407089921784865361, -6.421874999385540406 ) ) ;
#27658 = CARTESIAN_POINT ( 'NONE',  ( -7.234628195640316228, 197.6575961894323257, -27.00000000000000000 ) ) ;
#27659 = CARTESIAN_POINT ( 'NONE',  ( -7.234628195640354420, 195.7049038117966404, 26.99999999999996803 ) ) ;
#27660 = CARTESIAN_POINT ( 'NONE',  ( -3.474262827703337830, 88.03518628210144925, -8.843639120294326972 ) ) ;
#27661 = LINE ( 'NONE', #30514, #16473 ) ;
#27662 = ADVANCED_FACE ( 'NONE', ( #31467 ), #22394, .T. ) ;
#27663 = CARTESIAN_POINT ( 'NONE',  ( 8.715434833791931624, 138.0601862821014549, 8.962234695871760692 ) ) ;
#27664 = CARTESIAN_POINT ( 'NONE',  ( -10.88186518451280627, 142.9999999999999716, 1.989529451084718126 ) ) ;
#27665 = CARTESIAN_POINT ( 'NONE',  ( 23.87821517812499650, 249.7093750006145285, -4.985214923628404904 ) ) ;
#27666 = VERTEX_POINT ( 'NONE', #5490 ) ;
#27667 = CARTESIAN_POINT ( 'NONE',  ( 27.93778984224218931, 5.407089921784856479, 165.1177646232817153 ) ) ;
#27668 = CARTESIAN_POINT ( 'NONE',  ( 21.00000000000000000, -6.646953231504538984, -4.978124999385476812 ) ) ;
#27669 = CARTESIAN_POINT ( 'NONE',  ( -27.24356964375000345, 196.7093750006145569, 0.000000000000000000 ) ) ;
#27670 = CARTESIAN_POINT ( 'NONE',  ( 28.34590810202754696, 5.196152422706636465, 168.3852535544717739 ) ) ;
#27671 = CARTESIAN_POINT ( 'NONE',  ( 26.75643035624999655, 243.3343750006145285, -7.049594010296217766E-16 ) ) ;
#27672 = CARTESIAN_POINT ( 'NONE',  ( -51.40635080957662950, 236.9611623878118110, -0.4999999999999978351 ) ) ;
#27673 =( BOUNDED_CURVE ( )  B_SPLINE_CURVE ( 2, ( #22249, #30960, #4978, #16005, #16560, #28106, #1580, #27362, #2137 ),
 .UNSPECIFIED., .F., .F. ) 
 B_SPLINE_CURVE_WITH_KNOTS ( ( 3, 2, 2, 2, 3 ),
 ( 0.6875000000000000000, 0.6944444444444444198, 0.7083333333333333703, 0.7222222222222222099, 0.7291666666666667407 ),
 .UNSPECIFIED. ) 
 CURVE ( )  GEOMETRIC_REPRESENTATION_ITEM ( )  RATIONAL_B_SPLINE_CURVE ( ( 0.9330127018922194093, 0.9330127018922194093, 1.000000000000000000, 0.8660254037844387076, 1.000000000000000000, 0.8660254037844387076, 1.000000000000000000, 0.9330127018922187432, 0.9330127018922192983 ) ) 
 REPRESENTATION_ITEM ( '' )  );
#27674 = CARTESIAN_POINT ( 'NONE',  ( 2.660918448318002838, 132.7023137178985621, 12.46528703574811558 ) ) ;
#27675 = CARTESIAN_POINT ( 'NONE',  ( -13.62178482187498396, 195.4343750006145228, 23.59362340125808188 ) ) ;
#27677 = ORIENTED_EDGE ( 'NONE', *, *, #2165, .F. ) ;
#27676 = VERTEX_POINT ( 'NONE', #8536 ) ;
#27678 = CARTESIAN_POINT ( 'NONE',  ( 15.24356964374999990, 243.4468750006145115, 0.000000000000000000 ) ) ;
#27679 = CARTESIAN_POINT ( 'NONE',  ( 2.311890736173452421, 9.077313717898549683, -12.53471296425189152 ) ) ;
#27680 = CARTESIAN_POINT ( 'NONE',  ( 15.24356964374999990, 3.323476615752268604, -4.678124999385468108 ) ) ;
#27681 = CARTESIAN_POINT ( 'NONE',  ( -15.53471296425188442, 117.1773137178985706, -2.908627838312459080 ) ) ;
#27682 = CARTESIAN_POINT ( 'NONE',  ( 13.56230152254411614, -5.196152422706638241, -9.825000000000056133 ) ) ;
#27683 = ADVANCED_FACE ( 'NONE', ( #25409 ), #17073, .F. ) ;
#27684 = CARTESIAN_POINT ( 'NONE',  ( 15.00000000000000000, 0.000000000000000000, -9.393749998770960730 ) ) ;
#27685 = CARTESIAN_POINT ( 'NONE',  ( 22.80587116629411781, 3.604726614523243278, -6.684374999385513938 ) ) ;
#27686 = VERTEX_POINT ( 'NONE', #33942 ) ;
#27687 = CARTESIAN_POINT ( 'NONE',  ( -13.62178482187498396, 195.8281250006145342, 23.59362340125808188 ) ) ;
#27688 = CARTESIAN_POINT ( 'NONE',  ( -6.932735513423968321, 124.5476862821014663, -10.69584247140445221 ) ) ;
#27689 = CARTESIAN_POINT ( 'NONE',  ( 27.74986027194257332, -5.407089921784865361, 162.9697198055213789 ) ) ;
#27690 = CARTESIAN_POINT ( 'NONE',  ( -52.37127896937850835, 218.5309553116392465, 2.162041339862725842 ) ) ;
#27691 = CARTESIAN_POINT ( 'NONE',  ( 18.12178482187499640, 247.8718750006145228, -4.985214923628404904 ) ) ;
#27692 = SURFACE_STYLE_USAGE ( .BOTH. , #1531 ) ;
#27693 = VECTOR ( 'NONE', #3301, 1000.000000000000000 ) ;
#27694 = CARTESIAN_POINT ( 'NONE',  ( 26.99999999999999645, 240.2874999999999943, 3.464101615137751278 ) ) ;
#27695 = CARTESIAN_POINT ( 'NONE',  ( -66.62127896937846572, 216.5309553116391612, 1.626142955000506873 ) ) ;
#27696 = CARTESIAN_POINT ( 'NONE',  ( -8.715434833791929847, 133.4601862821014606, -8.962234695871762469 ) ) ;
#27697 = CARTESIAN_POINT ( 'NONE',  ( 13.56230152254410726, 5.196152422706630247, -0.4124999987710209481 ) ) ;
#27698 = ORIENTED_EDGE ( 'NONE', *, *, #676, .F. ) ;
#27699 = CYLINDRICAL_SURFACE ( 'NONE', #28236, 27.00000000000000355 ) ;
#27700 = CARTESIAN_POINT ( 'NONE',  ( 3.257655550457285720, 125.6976862821014578, -15.46528703574804986 ) ) ;
#27701 = EDGE_CURVE ( 'NONE', #8607, #14469, #16766, .T. ) ;
#27702 = CARTESIAN_POINT ( 'NONE',  ( -1.715153634034234598, 115.9226862821014521, -9.534712964251941258 ) ) ;
#27703 = DIRECTION ( 'NONE',  ( 0.9961946980917462113, 0.000000000000000000, -0.08715574274765118534 ) ) ;
#27704 = CARTESIAN_POINT ( 'NONE',  ( 6.932735513423970097, 9.547686282101453870, 10.69584247140445044 ) ) ;
#27705 = CARTESIAN_POINT ( 'NONE',  ( 10.56230152254410548, -3.464101615137761048, -9.412500000000042277 ) ) ;
#27706 = VERTEX_POINT ( 'NONE', #22950 ) ;
#27707 = DIRECTION ( 'NONE',  ( 0.000000000000000000, 0.000000000000000000, -1.000000000000000000 ) ) ;
#27708 = CARTESIAN_POINT ( 'NONE',  ( 1.715153634034233487, 83.72268628210143504, 9.534712964251941258 ) ) ;
#27709 =( BOUNDED_CURVE ( )  B_SPLINE_CURVE ( 2, ( #18291, #15442, #9563, #12402, #29265, #29458, #26423 ),
 .UNSPECIFIED., .F., .F. ) 
 B_SPLINE_CURVE_WITH_KNOTS ( ( 3, 2, 2, 3 ),
 ( 0.6304347826086944551, 0.6376811594202886901, 0.6449275362318829252, 0.6521739130434772713 ),
 .UNSPECIFIED. ) 
 CURVE ( )  GEOMETRIC_REPRESENTATION_ITEM ( )  RATIONAL_B_SPLINE_CURVE ( ( 1.000000000000022649, 0.8660254037844161701, 1.000000000000000000, 0.8660254037844387076, 1.000000000000000000, 0.8660254037844571373, 0.9999999999999815703 ) ) 
 REPRESENTATION_ITEM ( '' )  );
#27710 = CARTESIAN_POINT ( 'NONE',  ( 2.064181346179061460, 123.5023137178985451, 9.465287035748106703 ) ) ;
#27711 = CARTESIAN_POINT ( 'NONE',  ( 5.778771075727756162E-15, 197.2156250006145513, 31.45816453501075927 ) ) ;
#27712 = CARTESIAN_POINT ( 'NONE',  ( 25.09912511996950713, 0.000000000000000000, 165.6954939908422944 ) ) ;
#27713 = CARTESIAN_POINT ( 'NONE',  ( -13.62178482187500528, 198.8843750006145399, -23.59362340125807123 ) ) ;
#27714 = FACE_OUTER_BOUND ( 'NONE', #15655, .T. ) ;
#27715 = FACE_OUTER_BOUND ( 'NONE', #24475, .T. ) ;
#27716 = CARTESIAN_POINT ( 'NONE',  ( 5.233372021372610483, 55.65231371789855785, -8.152565276336593669 ) ) ;
#27717 = CARTESIAN_POINT ( 'NONE',  ( 26.99999999999999645, 7.347880794884117764E-16, -7.424999999999987388 ) ) ;
#27718 = ORIENTED_EDGE ( 'NONE', *, *, #33864, .T. ) ;
#27719 = CARTESIAN_POINT ( 'NONE',  ( 15.00000000000000178, 241.5437500012290570, 3.464101615137757051 ) ) ;
#27720 = CIRCLE ( 'NONE', #2012, 28.99999999999999645 ) ;
#27721 = CARTESIAN_POINT ( 'NONE',  ( 12.46528703574811558, 75.20231371789854791, -2.660918448318005947 ) ) ;
#27722 = CARTESIAN_POINT ( 'NONE',  ( 10.31873187879410736, 3.604726614523240613, -6.084374999385531169 ) ) ;
#27723 = CARTESIAN_POINT ( 'NONE',  ( -13.62178482187500528, 199.7281250006145399, -23.59362340125807123 ) ) ;
#27724 = CARTESIAN_POINT ( 'NONE',  ( 15.24356964374999990, 3.323476615752268604, -6.140624999385478233 ) ) ;
#27725 = CARTESIAN_POINT ( 'NONE',  ( -8.962234695871565293, 26.03981371789855359, -8.715434833792128799 ) ) ;
#27726 = ORIENTED_EDGE ( 'NONE', *, *, #20040, .T. ) ;
#27727 = CIRCLE ( 'NONE', #11378, 28.99999999999999645 ) ;
#27728 = CARTESIAN_POINT ( 'NONE',  ( 15.24356964374999990, 3.323476615752268604, -7.828124999385471128 ) ) ;
#27729 = CARTESIAN_POINT ( 'NONE',  ( 11.48171059495397728, 17.88518628210143646, 4.944772684328674117 ) ) ;
#27730 = ADVANCED_FACE ( 'NONE', ( #5314, #34124 ), #25964, .T. ) ;
#27731 = CARTESIAN_POINT ( 'NONE',  ( 28.24664800560418243, 5.407089921784862696, 168.6480295846443482 ) ) ;
#27732 = CARTESIAN_POINT ( 'NONE',  ( -56.13169563604517265, 210.1155267958017703, 6.500000000000000888 ) ) ;
#27733 = CARTESIAN_POINT ( 'NONE',  ( -27.00000000000000355, 196.4000000000000057, 0.000000000000000000 ) ) ;
#27734 = CARTESIAN_POINT ( 'NONE',  ( 10.49813415416005213, 65.42731371789855643, -7.228626920338837358 ) ) ;
#27735 = CARTESIAN_POINT ( 'NONE',  ( -35.75372103062156981, 214.5309553116392749, -1.090244570138262148 ) ) ;
#27736 = CARTESIAN_POINT ( 'NONE',  ( -61.87872103062154849, 203.4690446883607535, 1.626142955000567936 ) ) ;
#27737 = CLOSED_SHELL ( 'NONE', ( #29378, #9574, #26465, #4055, #22363, #30691, #8890, #33127, #31420, #27730, #36098, #2063, #7335, #3343, #24640, #165, #21077, #15517, #35849, #11878, #16362, #22891, #22610, #14129, #20159, #2225, #17078, #31832, #33336, #22943, #7750, #20439, #12134, #31495, #4367, #23509, #29315 ) ) ;
#27738 = AXIS2_PLACEMENT_3D ( 'NONE', #27797, #16432, #19471 ) ;
#27739 = DIRECTION ( 'NONE',  ( -0.000000000000000000, 0.000000000000000000, -1.000000000000000000 ) ) ;
#27740 = CARTESIAN_POINT ( 'NONE',  ( 10.56230152254405752, -3.464101615137729961, -6.262500000000040146 ) ) ;
#27741 = CARTESIAN_POINT ( 'NONE',  ( -14.25334919248795096, 33.51481371789854791, 6.092822981423662299 ) ) ;
#27742 = CARTESIAN_POINT ( 'NONE',  ( -48.61086230271182984, 214.1499508600178387, -7.418979330068641964 ) ) ;
#27743 = CARTESIAN_POINT ( 'NONE',  ( -81.72704584564829133, 216.6260876520869658, 7.500000000000000000 ) ) ;
#27744 = CARTESIAN_POINT ( 'NONE',  ( 10.49813415415989581, 64.17268628210143788, 7.228626920339068285 ) ) ;
#27745 = CARTESIAN_POINT ( 'NONE',  ( 11.08355503943142750, 16.16018628210144570, -10.83675517735155225 ) ) ;
#27746 = CARTESIAN_POINT ( 'NONE',  ( 13.56230152254411614, -5.196152422706638241, -1.275000000000053868 ) ) ;
#27747 = CARTESIAN_POINT ( 'NONE',  ( 3.306546357697854128E-15, 200.0000000000000000, 27.00000000000000355 ) ) ;
#27748 = ORIENTED_EDGE ( 'NONE', *, *, #32055, .F. ) ;
#27749 = CARTESIAN_POINT ( 'NONE',  ( -13.23911966647218463, 21.04768628210144499, 8.632099005475506459 ) ) ;
#27750 = CARTESIAN_POINT ( 'NONE',  ( 27.24356964375000345, 195.9781250006145399, -3.336375036156643733E-15 ) ) ;
#27751 = CARTESIAN_POINT ( 'NONE',  ( 27.24356964374999635, 197.4218750006145342, -15.72908226750539029 ) ) ;
#27752 = CARTESIAN_POINT ( 'NONE',  ( 33.83282523762249383, -5.196152422706635576, 162.2587239212197971 ) ) ;
#27753 = DIRECTION ( 'NONE',  ( 0.000000000000000000, 0.000000000000000000, 1.000000000000000000 ) ) ;
#27754 = CARTESIAN_POINT ( 'NONE',  ( 4.944772684328679446, 6.385186282101440014, -11.48171059495397373 ) ) ;
#27755 = CARTESIAN_POINT ( 'NONE',  ( 26.75643035624999655, 248.3218750006145399, -3.323476615752271712 ) ) ;
#27756 = CARTESIAN_POINT ( 'NONE',  ( -8.843639120294245259, 117.4648137178985650, -3.474262827703533230 ) ) ;
#27757 = CARTESIAN_POINT ( 'NONE',  ( 26.75643035624999655, 243.3343750006145285, -7.049594010296217766E-16 ) ) ;
#27758 = VERTEX_POINT ( 'NONE', #31651 ) ;
#27759 = SURFACE_SIDE_STYLE ('',( #2351 ) ) ;
#27760 = CARTESIAN_POINT ( 'NONE',  ( 2.999999999999997335, 252.0000000000000000, -5.000000000000000000 ) ) ;
#27761 = CARTESIAN_POINT ( 'NONE',  ( 11.61527771782809637, 140.4648137178985792, 4.622313124798827388 ) ) ;
#27762 = EDGE_CURVE ( 'NONE', #37335, #20530, #5678, .T. ) ;
#27763 = CARTESIAN_POINT ( 'NONE',  ( 13.44051670066911264, 5.407089921784856479, -8.315624999385541116 ) ) ;
#27764 = CARTESIAN_POINT ( 'NONE',  ( 37.17926111711567927, 3.604726614523238837, 163.2928730669172523 ) ) ;
#27765 = CARTESIAN_POINT ( 'NONE',  ( 26.99999999999999645, 240.7937500012290570, 3.464101615137751278 ) ) ;
#27766 = CARTESIAN_POINT ( 'NONE',  ( -13.49999999999998401, 198.2750000000000057, 23.38268590217985476 ) ) ;
#27767 = ORIENTED_EDGE ( 'NONE', *, *, #4409, .F. ) ;
#27768 = CARTESIAN_POINT ( 'NONE',  ( 2.660918448318279950, 33.69768628210144357, -12.46528703574805874 ) ) ;
#27769 = ORIENTED_EDGE ( 'NONE', *, *, #33781, .T. ) ;
#27770 = CIRCLE ( 'NONE', #4765, 7.500000000000000000 ) ;
#27771 = ORIENTED_EDGE ( 'NONE', *, *, #17291, .F. ) ;
#27772 = CARTESIAN_POINT ( 'NONE',  ( 15.00000000000000000, 3.464101615137752166, -4.931249998770940834 ) ) ;
#27773 = CARTESIAN_POINT ( 'NONE',  ( 21.00000000000000000, 242.0687500012289775, 5.999999999999998224 ) ) ;
#27774 = CARTESIAN_POINT ( 'NONE',  ( -13.50000000000000533, 196.3249999999999886, -23.38268590217984411 ) ) ;
#27775 = CARTESIAN_POINT ( 'NONE',  ( 15.24356964374999990, 0.000000000000000000, -7.790624999385459049 ) ) ;
#27776 = CARTESIAN_POINT ( 'NONE',  ( 10.69584247140445221, 80.84768628210144925, -6.932735513423970097 ) ) ;
#27777 = EDGE_CURVE ( 'NONE', #7496, #27046, #17361, .T. ) ;
#27778 = CARTESIAN_POINT ( 'NONE',  ( -3.257655550457281723, 139.4976862821014549, 15.46528703574804986 ) ) ;
#27779 = EDGE_CURVE ( 'NONE', #23066, #20369, #10954, .T. ) ;
#27780 = FACE_OUTER_BOUND ( 'NONE', #30623, .T. ) ;
#27781 = CARTESIAN_POINT ( 'NONE',  ( 14.99999999999999822, 225.9999999999999716, -0.1963495407219250366 ) ) ;
#27782 =( BOUNDED_CURVE ( )  B_SPLINE_CURVE ( 2, ( #16039, #7316, #19076, #36110, #27588, #1617, #27774, #13187, #24377 ),
 .UNSPECIFIED., .F., .F. ) 
 B_SPLINE_CURVE_WITH_KNOTS ( ( 3, 2, 2, 2, 3 ),
 ( 0.6458333333333333703, 0.6527777777777777901, 0.6666666666666666297, 0.6805555555555555802, 0.6875000000000000000 ),
 .UNSPECIFIED. ) 
 CURVE ( )  GEOMETRIC_REPRESENTATION_ITEM ( )  RATIONAL_B_SPLINE_CURVE ( ( 0.9330127018922192983, 0.9330127018922198534, 1.000000000000000000, 0.8660254037844387076, 1.000000000000000000, 0.8660254037844387076, 1.000000000000000000, 0.9330127018922194093, 0.9330127018922194093 ) ) 
 REPRESENTATION_ITEM ( '' )  );
#27783 = CARTESIAN_POINT ( 'NONE',  ( -57.12127896937850124, 214.5309553116392749, 1.090244570138288127 ) ) ;
#27784 = CARTESIAN_POINT ( 'NONE',  ( 20.99999999999999645, 185.0294372515228645, -5.999999999999999112 ) ) ;
#27785 = CARTESIAN_POINT ( 'NONE',  ( 37.10902328307209785, -3.464101615137751278, 165.2846991979039615 ) ) ;
#27786 = CARTESIAN_POINT ( 'NONE',  ( 12.53471296425189330, 130.9773137178985678, 2.311890736173451977 ) ) ;
#27787 = CARTESIAN_POINT ( 'NONE',  ( -47.23288769728823411, 203.5309553116391612, -1.857196546604028775 ) ) ;
#27788 = CARTESIAN_POINT ( 'NONE',  ( -60.29538769728823411, 212.3930949314662371, -8.469044688360781947 ) ) ;
#27789 = CARTESIAN_POINT ( 'NONE',  ( 18.12178482187499640, 4.985214923628404904, -3.028124999385484184 ) ) ;
#27790 = CARTESIAN_POINT ( 'NONE',  ( 27.24356964375000700, 197.2906250006145399, 15.72908226750537075 ) ) ;
#27791 = CARTESIAN_POINT ( 'NONE',  ( 14.38691631536194393, 94.46481371789855075, 5.770363421894124656 ) ) ;
#27792 = CARTESIAN_POINT ( 'NONE',  ( -49.60044563604517265, 205.1570982666397072, -4.673758765035155527 ) ) ;
#27793 = VERTEX_POINT ( 'NONE', #23134 ) ;
#27794 = CARTESIAN_POINT ( 'NONE',  ( 24.89321967762106169, 0.000000000000000000, 163.3419840153761982 ) ) ;
#27795 = CARTESIAN_POINT ( 'NONE',  ( -10.69584247140444866, 122.2476862821014549, 6.932735513423972762 ) ) ;
#27796 = CARTESIAN_POINT ( 'NONE',  ( -11.08355503943142573, 66.76018628210144357, 10.83675517735155402 ) ) ;
#27797 = CARTESIAN_POINT ( 'NONE',  ( 0.000000000000000000, 143.0000000000000000, 0.000000000000000000 ) ) ;
#27798 = CARTESIAN_POINT ( 'NONE',  ( 34.09386818162830224, -5.407089921784861808, 163.8451343006043999 ) ) ;
#27799 = CARTESIAN_POINT ( 'NONE',  ( 11.08355503943142750, 89.76018628210145778, -10.83675517735155225 ) ) ;
#27800 = ADVANCED_BREP_SHAPE_REPRESENTATION ( '', ( #20793, #17215 ), #15973 ) ;
#27801 = CARTESIAN_POINT ( 'NONE',  ( -52.18080436395490551, 203.5000000000000000, -0.1155267958017335561 ) ) ;
#27802 = CARTESIAN_POINT ( 'NONE',  ( 16.56230152254411436, -7.209453229046475009, -4.528124999385512162 ) ) ;
#27803 = CARTESIAN_POINT ( 'NONE',  ( -6.594114490232312775, 41.46018628210145351, -6.840914352312096547 ) ) ;
#27804 = DIRECTION ( 'NONE',  ( 0.000000000000000000, 1.000000000000000000, 0.000000000000000000 ) ) ;
#27805 = CARTESIAN_POINT ( 'NONE',  ( -67.61830436395489130, 209.8844732041982581, 6.500000000000000888 ) ) ;
#27806 = CARTESIAN_POINT ( 'NONE',  ( 2.999999999999997335, 244.5000000000000000, -2.499999999999999556 ) ) ;
#27807 = CARTESIAN_POINT ( 'NONE',  ( -8.962234695871760692, 57.56018628210145494, 8.715434833791933400 ) ) ;
#27808 = CARTESIAN_POINT ( 'NONE',  ( -13.49999999999998401, 199.6250000000000284, 23.38268590217985476 ) ) ;
#27809 = DIRECTION ( 'NONE',  ( -0.000000000000000000, -1.000000000000000000, -0.000000000000000000 ) ) ;
#27811 = CARTESIAN_POINT ( 'NONE',  ( 10.31873187879410736, 3.604726614523240613, -2.034374999385505145 ) ) ;
#27810 = CARTESIAN_POINT ( 'NONE',  ( 5.529263428287477744, 25.07268628210145067, -7.954856959092191815 ) ) ;
#27812 = DIRECTION ( 'NONE',  ( -0.000000000000000000, -0.000000000000000000, 1.000000000000000000 ) ) ;
#27813 = ORIENTED_EDGE ( 'NONE', *, *, #36921, .F. ) ;
#27814 = CARTESIAN_POINT ( 'NONE',  ( 26.99999999999999645, 3.464101615137755275, -1.987499999999999600 ) ) ;
#27815 = CARTESIAN_POINT ( 'NONE',  ( 27.77600699476686330, 5.407089921784862696, 163.2685782149489171 ) ) ;
#27816 = CARTESIAN_POINT ( 'NONE',  ( 24.69385091608581462, 3.464101615137757051, 161.0631886434913156 ) ) ;
#27817 = CARTESIAN_POINT ( 'NONE',  ( 26.99999999999999645, 246.1750000000000114, -7.347880794884117764E-16 ) ) ;
#27818 = CARTESIAN_POINT ( 'NONE',  ( 21.00000000000000355, 0.000000000000000000, 50.00000000000001421 ) ) ;
#27819 = CARTESIAN_POINT ( 'NONE',  ( -4.622313124798826500, 87.56481371789855928, 11.61527771782809637 ) ) ;
#27820 = CARTESIAN_POINT ( 'NONE',  ( 4.622313124798573369, 92.63518628210145778, 11.61527771782819940 ) ) ;
#27821 = ORIENTED_EDGE ( 'NONE', *, *, #33561, .T. ) ;
#27822 = ORIENTED_EDGE ( 'NONE', *, *, #36115, .F. ) ;
#27823 = CARTESIAN_POINT ( 'NONE',  ( 27.00000000000001066, 199.4000000012290172, 15.58845726811988897 ) ) ;
#27824 = CARTESIAN_POINT ( 'NONE',  ( 6.092822981423662299, 58.81481371789855217, 14.25334919248795096 ) ) ;
#27825 = CARTESIAN_POINT ( 'NONE',  ( 18.12178482187499640, 4.985214923628404904, -5.728124999385491911 ) ) ;
#27826 = CARTESIAN_POINT ( 'NONE',  ( 26.75643035624999655, 246.0718750006145115, -3.323476615752271712 ) ) ;
#27827 = CARTESIAN_POINT ( 'NONE',  ( -56.73288769728824832, 205.5309553116392465, -1.321298161741839117 ) ) ;
#27828 = CARTESIAN_POINT ( 'NONE',  ( 26.99999999999946354, 3.464101615138061696, -7.387499999999973532 ) ) ;
#27829 = CARTESIAN_POINT ( 'NONE',  ( -3.474262827703527901, 41.56481371789855217, 8.843639120294245259 ) ) ;
#27830 = CARTESIAN_POINT ( 'NONE',  ( 13.44051670066911441, -5.407089921784859143, -8.615624999385563143 ) ) ;
#27831 = CARTESIAN_POINT ( 'NONE',  ( -0.1745138560723084320, 100.7898137178985536, -9.500000000000005329 ) ) ;
#27832 = CARTESIAN_POINT ( 'NONE',  ( 27.24356964375000700, 198.2468750006145513, 15.72908226750537075 ) ) ;
#27833 = CARTESIAN_POINT ( 'NONE',  ( 12.46528703574811558, 10.80231371789855466, -2.660918448318005503 ) ) ;
#27834 = CARTESIAN_POINT ( 'NONE',  ( -12.50000000000000355, 58.71018628210145351, -0.1745138560725492671 ) ) ;
#27835 = CARTESIAN_POINT ( 'NONE',  ( 19.56230152254410370, 5.196152422706631135, -7.687499998771024856 ) ) ;
#27836 = CARTESIAN_POINT ( 'NONE',  ( 19.39230484541327471, 247.3924038105677141, 6.000000000000002665 ) ) ;
#27837 = CARTESIAN_POINT ( 'NONE',  ( 24.63832061363088854, 0.000000000000000000, 163.2231226297810451 ) ) ;
#27838 = CARTESIAN_POINT ( 'NONE',  ( 14.39393254099748276, 5.957544813848101306, -10.18332777273551848 ) ) ;
#27839 = CARTESIAN_POINT ( 'NONE',  ( 16.56230152254411436, 7.209453229046482114, -6.609374999385519978 ) ) ;
#27840 = VECTOR ( 'NONE', #11068, 1000.000000000000000 ) ;
#27841 = CARTESIAN_POINT ( 'NONE',  ( -89.59418277001438469, 62.43429747954478159, 5.000000000000000000 ) ) ;
#27842 = CARTESIAN_POINT ( 'NONE',  ( -8.843639120294326972, 94.93518628210146915, 3.474262827703335166 ) ) ;
#27843 = CYLINDRICAL_SURFACE ( 'NONE', #21937, 7.500000000000000000 ) ;
#27844 = CARTESIAN_POINT ( 'NONE',  ( -11.61527771782819940, 104.1351862821014578, 4.622313124798574258 ) ) ;
#27845 = CARTESIAN_POINT ( 'NONE',  ( -6.415111792407825142, 142.9999999999984936, 10.48095429381284838 ) ) ;
#27846 = ORIENTED_EDGE ( 'NONE', *, *, #31954, .T. ) ;
#27847 = CARTESIAN_POINT ( 'NONE',  ( 24.75271252598717808, 3.604726614523236616, 164.5306281710264216 ) ) ;
#27848 = CARTESIAN_POINT ( 'NONE',  ( 18.12178482187499640, 4.985214923628404904, -4.715624999385465088 ) ) ;
#27849 = CARTESIAN_POINT ( 'NONE',  ( 13.62178482187501416, 198.2093750006145285, 23.59362340125806767 ) ) ;
#27850 = CARTESIAN_POINT ( 'NONE',  ( 15.50407758876934672, -2.353417321935399098, -8.000000000000001776 ) ) ;
#27851 = CARTESIAN_POINT ( 'NONE',  ( 37.29531868308808384, -3.464101615137755275, 167.4140653638507388 ) ) ;
#27852 = CARTESIAN_POINT ( 'NONE',  ( 9.184850993605147944E-16, 141.0000000000000000, -7.500000000000000000 ) ) ;
#27853 = CARTESIAN_POINT ( 'NONE',  ( 21.00000000000000000, 243.6718750006145058, 6.646953231504538984 ) ) ;
#27854 = CARTESIAN_POINT ( 'NONE',  ( -77.35272773637332477, 226.7246823105297153, 0.4999999999999995559 ) ) ;
#27855 = CARTESIAN_POINT ( 'NONE',  ( -10.49813415416004858, 143.6273137178986019, 7.228626920338839135 ) ) ;
#27856 = CARTESIAN_POINT ( 'NONE',  ( 6.932735513423970097, 138.3476862821014493, 10.69584247140445044 ) ) ;
#27857 = CIRCLE ( 'NONE', #12103, 27.00000000000000355 ) ;
#27859 = EDGE_LOOP ( 'NONE', ( #21991, #34555, #25152, #15 ) ) ;
#27858 = ORIENTED_EDGE ( 'NONE', *, *, #32161, .T. ) ;
#27860 = CARTESIAN_POINT ( 'NONE',  ( 23.87821517812500005, 243.5968750006145171, 4.985214923628404016 ) ) ;
#27861 = CARTESIAN_POINT ( 'NONE',  ( -47.00000000000000711, 244.5000000000000000, 0.4999999999999995559 ) ) ;
#27862 = CARTESIAN_POINT ( 'NONE',  ( 18.12178482187500350, -4.985214923628407568, -5.015624999385459581 ) ) ;
#27863 = CARTESIAN_POINT ( 'NONE',  ( 14.38691631536194393, 103.6648137178985678, 5.770363421894124656 ) ) ;
#27864 = CARTESIAN_POINT ( 'NONE',  ( 16.56230152254411792, -6.928203230275514990, -0.3375000000000368816 ) ) ;
#27865 = CARTESIAN_POINT ( 'NONE',  ( 23.99999999999999645, 5.196152422706631135, -9.543749998770945098 ) ) ;
#27866 = CARTESIAN_POINT ( 'NONE',  ( 16.56230152254411436, -7.209453229046482114, -7.734374999385494220 ) ) ;
#27867 = ORIENTED_EDGE ( 'NONE', *, *, #16847, .T. ) ;
#27868 = CARTESIAN_POINT ( 'NONE',  ( -27.00000000000000355, 198.7250000012290059, -15.58845726811989429 ) ) ;
#27869 = AXIS2_PLACEMENT_3D ( 'NONE', #29301, #2967, #20607 ) ;
#27870 = CARTESIAN_POINT ( 'NONE',  ( -11.61527771782819940, 122.5351862821014635, 4.622313124798574258 ) ) ;
#27871 = DIRECTION ( 'NONE',  ( -0.1155267958017757585, -0.9933043639548629899, 1.378486719154166141E-14 ) ) ;
#27872 =( BOUNDED_CURVE ( )  B_SPLINE_CURVE ( 2, ( #23803, #17562, #11671, #35343, #29666, #14896, #32504, #9208, #15270 ),
 .UNSPECIFIED., .F., .F. ) 
 B_SPLINE_CURVE_WITH_KNOTS ( ( 3, 2, 2, 2, 3 ),
 ( 0.4375000000000000000, 0.4444444444444444198, 0.4583333333333333148, 0.4722222222222222099, 0.4791666666666666852 ),
 .UNSPECIFIED. ) 
 CURVE ( )  GEOMETRIC_REPRESENTATION_ITEM ( )  RATIONAL_B_SPLINE_CURVE ( ( 0.9330127018922194093, 0.9330127018922194093, 1.000000000000000000, 0.8660254037844387076, 1.000000000000000000, 0.8660254037844387076, 1.000000000000000000, 0.9330127018922190762, 0.9330127018922194093 ) ) 
 REPRESENTATION_ITEM ( '' )  );
#27873 = CARTESIAN_POINT ( 'NONE',  ( -38.51711230271182984, 218.4690446883607535, -2.393094931466363651 ) ) ;
#27874 = CARTESIAN_POINT ( 'NONE',  ( 23.87821517812500005, 244.9468750006145115, 4.985214923628404016 ) ) ;
#27875 = CARTESIAN_POINT ( 'NONE',  ( -27.00000000000000355, 197.4125000012290343, 0.000000000000000000 ) ) ;
#27876 = CARTESIAN_POINT ( 'NONE',  ( -67.80877896937850835, 211.6261429550004607, -6.530955311639245586 ) ) ;
#27877 = CARTESIAN_POINT ( 'NONE',  ( 6.932735513423970097, 138.3476862821014493, 10.69584247140445044 ) ) ;
#27878 = CARTESIAN_POINT ( 'NONE',  ( 16.56230152254411081, -6.928203230275506996, -2.474999998771027165 ) ) ;
#27879 = ORIENTED_EDGE ( 'NONE', *, *, #22340, .F. ) ;
#27880 = CARTESIAN_POINT ( 'NONE',  ( 7.234628195640322446, 195.2950961906613827, 26.99999999999999645 ) ) ;
#27881 = COLOUR_RGB ( '',0.8941176470588234615, 0.8941176470588234615, 0.8941176470588234615 ) ;
#27882 = CARTESIAN_POINT ( 'NONE',  ( 20.99999999999999289, 244.4874999999999829, -5.999999999999997335 ) ) ;
#27883 = CARTESIAN_POINT ( 'NONE',  ( -15.46528703574804986, 123.3976862821014606, -3.257655550457287497 ) ) ;
#27884 = CARTESIAN_POINT ( 'NONE',  ( 13.50000000000001421, 197.9000000000000341, 23.38268590217984055 ) ) ;
#27885 = CARTESIAN_POINT ( 'NONE',  ( -6.932735513423968321, 4.947686282101432909, -10.69584247140445221 ) ) ;
#27886 = EDGE_CURVE ( 'NONE', #18467, #2746, #31834, .T. ) ;
#27887 = CARTESIAN_POINT ( 'NONE',  ( 10.56230152254410903, 3.464101615137757051, -8.587500000000074962 ) ) ;
#27888 = VERTEX_POINT ( 'NONE', #28984 ) ;
#27889 = CARTESIAN_POINT ( 'NONE',  ( 10.56230152254443055, -3.464101615137944457, -3.562500000000028422 ) ) ;
#27890 = CARTESIAN_POINT ( 'NONE',  ( 0.1745138560725194299, 79.41018628210144925, -9.500000000000005329 ) ) ;
#27891 = FACE_BOUND ( 'NONE', #22976, .T. ) ;
#27892 = CARTESIAN_POINT ( 'NONE',  ( 3.474262827703532341, 128.9648137178985792, -8.843639120294245259 ) ) ;
#27893 = CARTESIAN_POINT ( 'NONE',  ( 27.24356964375000345, 197.3281250006145342, -3.336375036156643733E-15 ) ) ;
#27894 = FACE_OUTER_BOUND ( 'NONE', #20491, .T. ) ;
#27895 = CARTESIAN_POINT ( 'NONE',  ( -13.62178482187498396, 198.5843750006145569, 23.59362340125808188 ) ) ;
#27896 = CARTESIAN_POINT ( 'NONE',  ( 9.262227810926050964, 194.9999999999998579, 25.63589452377446065 ) ) ;
#27897 = ADVANCED_FACE ( 'NONE', ( #3025 ), #549, .F. ) ;
#27898 = CARTESIAN_POINT ( 'NONE',  ( 6.840914352311949109, 58.23981371789854222, 6.594114490232462877 ) ) ;
#27899 = CARTESIAN_POINT ( 'NONE',  ( 37.13843834614275607, -3.464101615137510137, 165.6209149072855098 ) ) ;
#27900 = EDGE_LOOP ( 'NONE', ( #27074, #32702, #9823, #19964, #10238, #23764, #29430, #3848 ) ) ;
#27901 = CARTESIAN_POINT ( 'NONE',  ( 26.99999999999999645, 242.6312500012290343, -7.347880794884117764E-16 ) ) ;
#27902 = CARTESIAN_POINT ( 'NONE',  ( -4.944772684328424539, 54.21481371789854364, -11.48171059495408031 ) ) ;
#27903 = CARTESIAN_POINT ( 'NONE',  ( 10.31873187879411091, -3.604726614523244610, -6.009374999385537208 ) ) ;
#27904 = CARTESIAN_POINT ( 'NONE',  ( -1.926257025242585782E-15, 198.3406250006145228, -31.45816453501075927 ) ) ;
#27905 = CARTESIAN_POINT ( 'NONE',  ( 15.24356964374999990, 0.000000000000000000, -7.453124999385495997 ) ) ;
#27906 = CARTESIAN_POINT ( 'NONE',  ( 11.61527771782809637, 30.06481371789855572, 4.622313124798827388 ) ) ;
#27907 = ORIENTED_EDGE ( 'NONE', *, *, #28617, .T. ) ;
#27908 = UNCERTAINTY_MEASURE_WITH_UNIT (LENGTH_MEASURE( 1.000000000000000082E-05 ), #34024, 'distance_accuracy_value', 'NONE');
#27909 = CARTESIAN_POINT ( 'NONE',  ( 16.56230152254411436, 7.209453229046482114, -0.3093749993854842395 ) ) ;
#27910 = EDGE_CURVE ( 'NONE', #18435, #2079, #28876, .T. ) ;
#27911 = CARTESIAN_POINT ( 'NONE',  ( 12.50000000000000355, 8.110186282101444988, 0.1745138560725507937 ) ) ;
#27912 = CARTESIAN_POINT ( 'NONE',  ( 16.56230152254411081, 6.928203230275506996, -9.449999998771041021 ) ) ;
#27913 = CARTESIAN_POINT ( 'NONE',  ( -56.52752896937850124, 213.3500491399821613, 5.571401726697954970 ) ) ;
#27914 = CARTESIAN_POINT ( 'NONE',  ( 22.56230152254369514, 3.464101615138004409, -9.637499999999985079 ) ) ;
#27915 = CARTESIAN_POINT ( 'NONE',  ( 4.622313124798831829, 64.56481371789855928, -11.61527771782809282 ) ) ;
#27916 = CARTESIAN_POINT ( 'NONE',  ( -35.55580436395489130, 214.5000000000000284, 0.1155267958017899832 ) ) ;
#27917 = CARTESIAN_POINT ( 'NONE',  ( -58.31622103062155560, 211.6261429550005744, 6.530955311639227823 ) ) ;
#27918 = CARTESIAN_POINT ( 'NONE',  ( 15.00000000000000000, 0.000000000000000000, -6.750000000000006217 ) ) ;
#27919 = CARTESIAN_POINT ( 'NONE',  ( 26.99999999999976197, -3.464101615137889834, -2.906249998770947141 ) ) ;
#27920 = CARTESIAN_POINT ( 'NONE',  ( 11.08355503943118769, 30.63981371789855146, 10.83675517735179028 ) ) ;
#27921 = CARTESIAN_POINT ( 'NONE',  ( -69.39955436395489130, 216.3070033484980002, -6.137860380172975638 ) ) ;
#27922 =( BOUNDED_CURVE ( )  B_SPLINE_CURVE ( 2, ( #33988, #9102, #14089, #31154, #17644, #12123, #2337, #8032, #2145 ),
 .UNSPECIFIED., .F., .F. ) 
 B_SPLINE_CURVE_WITH_KNOTS ( ( 3, 2, 2, 2, 3 ),
 ( 0.8541666666666667407, 0.8611111111111111605, 0.8750000000000000000, 0.8888888888888888395, 0.8958333333333333703 ),
 .UNSPECIFIED. ) 
 CURVE ( )  GEOMETRIC_REPRESENTATION_ITEM ( )  RATIONAL_B_SPLINE_CURVE ( ( 0.9330127018922192983, 0.9330127018922198534, 1.000000000000000000, 0.8660254037844387076, 1.000000000000000000, 0.8660254037844387076, 1.000000000000000000, 0.9330127018922187432, 0.9330127018922192983 ) ) 
 REPRESENTATION_ITEM ( '' )  );
#27923 = CARTESIAN_POINT ( 'NONE',  ( 7.228626920339068285, 25.07268628210144712, -10.49813415415989581 ) ) ;
#27924 = CYLINDRICAL_SURFACE ( 'NONE', #15336, 5.999999999999999112 ) ;
#27925 = CARTESIAN_POINT ( 'NONE',  ( -4.622313124798576922, 60.43518628210145494, -11.61527771782819762 ) ) ;
#27926 = CARTESIAN_POINT ( 'NONE',  ( 13.23911966647218996, 16.44768628210144001, -8.632099005475504683 ) ) ;
#27927 = CARTESIAN_POINT ( 'NONE',  ( 13.56230152254410903, 5.196152422706636465, -2.775000000000027445 ) ) ;
#27928 = CARTESIAN_POINT ( 'NONE',  ( -28.99999999999999645, 201.9999999999999716, -1.007612034238798379E-23 ) ) ;
#27929 = ORIENTED_EDGE ( 'NONE', *, *, #1898, .T. ) ;
#27930 = CARTESIAN_POINT ( 'NONE',  ( 8.632099005475504683, 37.14768628210143220, 13.23911966647218996 ) ) ;
#27931 = DIRECTION ( 'NONE',  ( 0.1155267958017759666, 0.9933043639548631010, -1.378486719154166141E-14 ) ) ;
#27932 = ADVANCED_FACE ( 'NONE', ( #3402 ), #23316, .T. ) ;
#27933 = CARTESIAN_POINT ( 'NONE',  ( -27.24356964374999990, 199.3718750006145513, -15.72908226750537786 ) ) ;
#27934 = DIRECTION ( 'NONE',  ( 0.000000000000000000, 0.000000000000000000, 1.000000000000000000 ) ) ;
#27935 = CARTESIAN_POINT ( 'NONE',  ( 31.26258870864309003, 6.928203230275506996, 167.3019257015274945 ) ) ;
#27936 = LINE ( 'NONE', #11061, #5109 ) ;
#27937 = CARTESIAN_POINT ( 'NONE',  ( 18.00000000000000000, 247.6750000000000114, -5.196152422706630247 ) ) ;
#27938 = CARTESIAN_POINT ( 'NONE',  ( 15.24356964374999990, 248.5093750006145399, 0.000000000000000000 ) ) ;
#27939 = CARTESIAN_POINT ( 'NONE',  ( 3.796722387233182339, 104.8148137178985593, 8.710071997420207879 ) ) ;
#27940 = CARTESIAN_POINT ( 'NONE',  ( 15.24356964374999990, 243.0718750006145399, -3.323476615752268604 ) ) ;
#27941 = ORIENTED_EDGE ( 'NONE', *, *, #32869, .F. ) ;
#27942 = CARTESIAN_POINT ( 'NONE',  ( 10.56230152254410903, 0.000000000000000000, -7.200000000000040146 ) ) ;
#27943 = CARTESIAN_POINT ( 'NONE',  ( 24.00000000000000000, 248.4062500012290400, 5.196152422706629359 ) ) ;
#27944 = CARTESIAN_POINT ( 'NONE',  ( -8.715434833792127023, 115.7398137178985706, 8.962234695871568846 ) ) ;
#27945 = ADVANCED_FACE ( 'NONE', ( #26518 ), #3773, .T. ) ;
#27946 = CARTESIAN_POINT ( 'NONE',  ( 22.80587116629410360, -3.604726614523235284, -8.953124999385540406 ) ) ;
#27947 = CARTESIAN_POINT ( 'NONE',  ( 37.05506418370026722, -3.604726614523235284, 161.8732956221364532 ) ) ;
#27948 = CARTESIAN_POINT ( 'NONE',  ( 18.12178482187499640, 4.985214923628404904, -0.7781249993854821856 ) ) ;
#27949 = CARTESIAN_POINT ( 'NONE',  ( 26.99999999999999645, 198.0125000000000455, -15.58845726811990495 ) ) ;
#27950 = VERTEX_POINT ( 'NONE', #32397 ) ;
#27951 = CARTESIAN_POINT ( 'NONE',  ( 11.48171059495397728, 27.08518628210144996, 4.944772684328674117 ) ) ;
#27952 = EDGE_LOOP ( 'NONE', ( #17477, #34544, #12004, #9358 ) ) ;
#27953 = EDGE_LOOP ( 'NONE', ( #11360, #19114, #4620, #19421 ) ) ;
#27954 = CARTESIAN_POINT ( 'NONE',  ( 15.00000000000000000, 3.464101615137752166, -5.381249998770968546 ) ) ;
#27955 = CARTESIAN_POINT ( 'NONE',  ( 20.99999999999999645, -6.646953231504538984, -0.9281249993854503444 ) ) ;
#27956 = CARTESIAN_POINT ( 'NONE',  ( -70.80918835584510873, 215.2843023367891249, 7.500000000000000000 ) ) ;
#27957 = CARTESIAN_POINT ( 'NONE',  ( 6.123233995736767268E-16, 143.0000000000000000, 5.000000000000000888 ) ) ;
#27958 = CARTESIAN_POINT ( 'NONE',  ( 15.24356964375000167, -3.323476615752272600, -10.00312499938545407 ) ) ;
#27959 = CARTESIAN_POINT ( 'NONE',  ( 7.228626920339068285, 61.87268628210145494, -10.49813415415989581 ) ) ;
#27960 = CARTESIAN_POINT ( 'NONE',  ( 15.50000000000000533, 136.9101862821014777, 0.1745138560725827404 ) ) ;
#27961 = CARTESIAN_POINT ( 'NONE',  ( -60.09002896937850124, 204.4285982733020433, 3.350049139982171020 ) ) ;
#27962 = CARTESIAN_POINT ( 'NONE',  ( 4.999999999999997335, 215.9999999999999716, -0.1963495407219245925 ) ) ;
#27963 = CARTESIAN_POINT ( 'NONE',  ( -59.49627896937850835, 205.4690446883607535, -1.090244570138286351 ) ) ;
#27964 = CIRCLE ( 'NONE', #11608, 8.000000000000000000 ) ;
#27965 = LINE ( 'NONE', #27784, #6296 ) ;
#27966 = CARTESIAN_POINT ( 'NONE',  ( 24.97819652690714065, 3.464101615137752166, 164.3132738472399694 ) ) ;
#27967 = CARTESIAN_POINT ( 'NONE',  ( 6.932735513424201024, 120.0523137178985564, -10.69584247140429412 ) ) ;
#27968 = CARTESIAN_POINT ( 'NONE',  ( -67.61830436395490551, 209.8844732041982297, 4.499999999999996447 ) ) ;
#27969 = CARTESIAN_POINT ( 'NONE',  ( -58.71205436395490551, 216.1378603801730094, 6.307003348497944195 ) ) ;
#27970 = CARTESIAN_POINT ( 'NONE',  ( 23.87821517812500005, -4.985214923628404016, -2.803124999385481431 ) ) ;
#27971 = CARTESIAN_POINT ( 'NONE',  ( 27.24356964375000345, 195.9781250006145399, -3.336375036156643733E-15 ) ) ;
#27972 = CARTESIAN_POINT ( 'NONE',  ( -15.50000000000000533, 89.28981371789856780, 0.1745138560722471477 ) ) ;
#27973 = CARTESIAN_POINT ( 'NONE',  ( -41.48586230271182984, 206.8500491399821328, 5.686928522499748340 ) ) ;
#27974 = VERTEX_POINT ( 'NONE', #29169 ) ;
#27975 =( BOUNDED_CURVE ( )  B_SPLINE_CURVE ( 2, ( #24824, #13649, #19352, #16495, #36377, #25202, #22369 ),
 .UNSPECIFIED., .F., .F. ) 
 B_SPLINE_CURVE_WITH_KNOTS ( ( 3, 2, 2, 3 ),
 ( 0.6304347826086958984, 0.6376811594202901334, 0.6449275362318845906, 0.6521739130434789367 ),
 .UNSPECIFIED. ) 
 CURVE ( )  GEOMETRIC_REPRESENTATION_ITEM ( )  RATIONAL_B_SPLINE_CURVE ( ( 0.9999999999999958922, 0.8660254037844428154, 1.000000000000000000, 0.8660254037844387076, 1.000000000000000000, 0.8660254037844263841, 1.000000000000012212 ) ) 
 REPRESENTATION_ITEM ( '' )  );
#27976 = CARTESIAN_POINT ( 'NONE',  ( 33.84589859903464060, 5.196152422706637353, 162.4081531259335804 ) ) ;
#27977 = CARTESIAN_POINT ( 'NONE',  ( 4.944772684328679446, 116.7851862821014635, -11.48171059495397373 ) ) ;
#27978 = CARTESIAN_POINT ( 'NONE',  ( -10.83675517735155047, 69.06018628210144072, -11.08355503943142750 ) ) ;
#27979 = CARTESIAN_POINT ( 'NONE',  ( -79.74198084750223359, 216.3821266856691636, -3.000000000000000000 ) ) ;
#27980 = CARTESIAN_POINT ( 'NONE',  ( 34.05464809739185483, -5.407089921784861808, 163.3968466864631068 ) ) ;
#27981 = CARTESIAN_POINT ( 'NONE',  ( -2.908627838312119351, 88.32268628210142936, -15.53471296425195369 ) ) ;
#27982 = CARTESIAN_POINT ( 'NONE',  ( -53.17038769728823411, 208.1428034533959703, 6.469044688360771289 ) ) ;
#27983 = EDGE_CURVE ( 'NONE', #37220, #2680, #19811, .T. ) ;
#27984 = CARTESIAN_POINT ( 'NONE',  ( 16.56230152254411436, 7.209453229046475009, -7.003124999385537564 ) ) ;
#27985 = CARTESIAN_POINT ( 'NONE',  ( 1.715153634034233487, 28.52268628210144286, 9.534712964251941258 ) ) ;
#27986 = DIRECTION ( 'NONE',  ( 0.000000000000000000, 0.000000000000000000, 1.000000000000000000 ) ) ;
#27987 = CARTESIAN_POINT ( 'NONE',  ( -69.00372103062157692, 216.5309553116391612, -1.626142955000564383 ) ) ;
#27988 = CARTESIAN_POINT ( 'NONE',  ( 4.944772684328679446, 52.38518628210145067, -11.48171059495397373 ) ) ;
#27989 = CARTESIAN_POINT ( 'NONE',  ( 13.49999999999999645, 198.5000000000000000, -23.38268590217984766 ) ) ;
#27990 = CARTESIAN_POINT ( 'NONE',  ( 22.56230152254411792, 7.347880794884125653E-16, -6.975000000000036948 ) ) ;
#27992 = CARTESIAN_POINT ( 'NONE',  ( 19.68408634441911431, 5.407089921784862696, -0.3468749993855158031 ) ) ;
#27991 = CARTESIAN_POINT ( 'NONE',  ( 5.529263428287477744, 34.27268628210144641, -7.954856959092191815 ) ) ;
#27993 = FACE_OUTER_BOUND ( 'NONE', #7798, .T. ) ;
#27994 = ORIENTED_EDGE ( 'NONE', *, *, #13578, .F. ) ;
#27995 = CARTESIAN_POINT ( 'NONE',  ( 26.99999999999999645, 3.464101615137755275, -1.087499999999976374 ) ) ;
#27996 = CARTESIAN_POINT ( 'NONE',  ( 24.70858993122118008, 3.604726614523240613, 164.0263046051175024 ) ) ;
#27997 = CARTESIAN_POINT ( 'NONE',  ( 24.88995133726802322, 3.464101615137757051, 163.3046267141977239 ) ) ;
#27998 = CARTESIAN_POINT ( 'NONE',  ( 21.00000000000000000, 242.6875000000000284, -6.928203230275506996 ) ) ;
#27999 = CYLINDRICAL_SURFACE ( 'NONE', #2804, 27.00000000000000355 ) ;
#28000 =( BOUNDED_CURVE ( )  B_SPLINE_CURVE ( 2, ( #35198, #145, #23655, #29517, #3365, #18163, #32546, #15120, #11709 ),
 .UNSPECIFIED., .F., .F. ) 
 B_SPLINE_CURVE_WITH_KNOTS ( ( 3, 2, 2, 2, 3 ),
 ( 0.4891304347826087029, 0.4927536231884058204, 0.5000000000000000000, 0.5072463768115942351, 0.5108695652173913526 ),
 .UNSPECIFIED. ) 
 CURVE ( )  GEOMETRIC_REPRESENTATION_ITEM ( )  RATIONAL_B_SPLINE_CURVE ( ( 0.9330127018922194093, 0.9330127018922194093, 1.000000000000000000, 0.8660254037844387076, 1.000000000000000000, 0.8660254037844387076, 1.000000000000000000, 0.9330127018922182991, 0.9330127018922192983 ) ) 
 REPRESENTATION_ITEM ( '' )  );
#28001 = CARTESIAN_POINT ( 'NONE',  ( -0.1745138560722763466, 82.38981371789854791, -12.50000000000000355 ) ) ;
#28002 = CARTESIAN_POINT ( 'NONE',  ( 8.962234695871762469, 80.56018628210145494, -8.715434833791931624 ) ) ;
#28003 = EDGE_LOOP ( 'NONE', ( #29606, #27308 ) ) ;
#28004 = ORIENTED_EDGE ( 'NONE', *, *, #24982, .F. ) ;
#28005 = CARTESIAN_POINT ( 'NONE',  ( -13.49999999999998401, 197.9375000012290400, 23.38268590217985476 ) ) ;
#28006 = CARTESIAN_POINT ( 'NONE',  ( 31.23317364535864726, -6.928203230275514990, 166.9657099896972170 ) ) ;
#28007 = CARTESIAN_POINT ( 'NONE',  ( 8.632099005475788900, 55.65231371789855785, -13.23911966647199812 ) ) ;
#28008 = CARTESIAN_POINT ( 'NONE',  ( 26.75643035624999655, -3.323476615752267715, -9.515624999385494220 ) ) ;
#28009 = CARTESIAN_POINT ( 'NONE',  ( 15.24356964374999990, 242.6218750006145228, -3.323476615752268604 ) ) ;
#28010 = CARTESIAN_POINT ( 'NONE',  ( -56.33705436395490551, 206.7903428501026042, -3.378800118222489157 ) ) ;
#28011 = CARTESIAN_POINT ( 'NONE',  ( -7.234628195640307347, 199.4575961894323370, -27.00000000000000711 ) ) ;
#28012 = CARTESIAN_POINT ( 'NONE',  ( 1.715153634034445762, 45.87731371789854506, -9.534712964251895073 ) ) ;
#28013 = CARTESIAN_POINT ( 'NONE',  ( 13.44051670066911619, -5.407089921784859143, -9.065624999385569538 ) ) ;
#28014 = VECTOR ( 'NONE', #15802, 1000.000000000000000 ) ;
#28015 = CARTESIAN_POINT ( 'NONE',  ( 3.796722387233182339, 95.61481371789857064, 8.710071997420207879 ) ) ;
#28016 = CARTESIAN_POINT ( 'NONE',  ( 27.24356964375000345, 198.7343750006145626, -3.336375036156643733E-15 ) ) ;
#28017 = CARTESIAN_POINT ( 'NONE',  ( 12.46528703574811558, 20.00231371789855217, -2.660918448318005503 ) ) ;
#28018 = ADVANCED_FACE ( 'NONE', ( #1447 ), #27453, .T. ) ;
#28019 = CARTESIAN_POINT ( 'NONE',  ( -8.715434833791929847, 59.86018628210145209, -8.962234695871762469 ) ) ;
#28020 = CARTESIAN_POINT ( 'NONE',  ( 19.56230152254410370, 5.196152422706631135, -9.487499998770992704 ) ) ;
#28021 = VECTOR ( 'NONE', #3879, 1000.000000000000000 ) ;
#28022 = CARTESIAN_POINT ( 'NONE',  ( 23.99999999999999645, 5.196152422706631135, -1.893749998770954956 ) ) ;
#28023 = CARTESIAN_POINT ( 'NONE',  ( 33.86345018673919327, -5.407089921784855591, 161.2114445675243530 ) ) ;
#28024 = CARTESIAN_POINT ( 'NONE',  ( 18.00000000000000355, -5.196152422706632912, -1.218749998770946030 ) ) ;
#28025 = CARTESIAN_POINT ( 'NONE',  ( 16.56230152254411081, -7.209453229046482114, -6.834374999385502747 ) ) ;
#28026 = CARTESIAN_POINT ( 'NONE',  ( 16.56230152254410726, 0.000000000000000000, 10.00000000000000000 ) ) ;
#28027 = CARTESIAN_POINT ( 'NONE',  ( 24.74614436184151955, 0.000000000000000000, 161.6609054635707423 ) ) ;
#28028 = CARTESIAN_POINT ( 'NONE',  ( 9.500000000000005329, 90.91018628210146346, 0.1745138560725188748 ) ) ;
#28029 = VECTOR ( 'NONE', #24037, 1000.000000000000000 ) ;
#28030 = LINE ( 'NONE', #16670, #20710 ) ;
#28031 = ADVANCED_FACE ( 'NONE', ( #10849 ), #5521, .T. ) ;
#28032 = CARTESIAN_POINT ( 'NONE',  ( 8.962234695871762469, 108.1601862821014635, -8.715434833791931624 ) ) ;
#28033 = CYLINDRICAL_SURFACE ( 'NONE', #3950, 10.00000000000000178 ) ;
#28034 = CARTESIAN_POINT ( 'NONE',  ( 13.56230152254411436, -5.196152422706638241, -0.3750000000000419664 ) ) ;
#28035 = ORIENTED_EDGE ( 'NONE', *, *, #21252, .F. ) ;
#28036 = CARTESIAN_POINT ( 'NONE',  ( 34.19028422204287665, 5.407089921784857367, 164.9471746853683669 ) ) ;
#28037 = CARTESIAN_POINT ( 'NONE',  ( 18.12178482187500350, -4.985214923628407568, -4.115624999385475213 ) ) ;
#28038 = CARTESIAN_POINT ( 'NONE',  ( -27.24356964374999279, 198.0968750006145456, 15.72908226750539384 ) ) ;
#28039 = CARTESIAN_POINT ( 'NONE',  ( 37.63846293671737442, -3.604726614523238837, 168.5415738824881373 ) ) ;
#28040 = CARTESIAN_POINT ( 'NONE',  ( 28.30668801779110311, 5.196152422706636465, 167.9369659403305093 ) ) ;
#28041 = CARTESIAN_POINT ( 'NONE',  ( -0.5000000000000052180, 244.5000000000000000, -11.00000000000000000 ) ) ;
#28042 = CARTESIAN_POINT ( 'NONE',  ( 26.99999999999999645, 249.8124999999999716, -3.464101615137755275 ) ) ;
#28043 = LINE ( 'NONE', #13838, #16058 ) ;
#28044 = CARTESIAN_POINT ( 'NONE',  ( 6.594114490232462877, 9.939813717898537959, -6.840914352311949109 ) ) ;
#28045 = CARTESIAN_POINT ( 'NONE',  ( -27.24356964374999279, 195.8468750006145740, 15.72908226750539384 ) ) ;
#28047 = ORIENTED_EDGE ( 'NONE', *, *, #28617, .F. ) ;
#28046 = ORIENTED_EDGE ( 'NONE', *, *, #2962, .T. ) ;
#28048 = CARTESIAN_POINT ( 'NONE',  ( 23.87821517812500005, 244.4968750006145228, 4.985214923628404016 ) ) ;
#28049 = DIRECTION ( 'NONE',  ( -0.000000000000000000, 0.000000000000000000, 1.000000000000000000 ) ) ;
#28050 = CARTESIAN_POINT ( 'NONE',  ( 26.75643035624999655, 7.049594010296217766E-16, -4.415624999385469707 ) ) ;
#28051 = CARTESIAN_POINT ( 'NONE',  ( 0.1745138560722461762, 114.5898137178985650, 15.50000000000000533 ) ) ;
#28052 = DIRECTION ( 'NONE',  ( 1.000000000000000000, 0.000000000000000000, 2.312964634635742957E-16 ) ) ;
#28053 = CARTESIAN_POINT ( 'NONE',  ( 21.00000000000000000, -6.646953231504538984, -1.940624999385496929 ) ) ;
#28054 = CARTESIAN_POINT ( 'NONE',  ( 10.31873187879410736, 0.000000000000000000, -8.296874999385501326 ) ) ;
#28055 = ORIENTED_EDGE ( 'NONE', *, *, #8524, .F. ) ;
#28056 = CARTESIAN_POINT ( 'NONE',  ( -27.00000000000000355, 198.2750000012290741, -15.58845726811989429 ) ) ;
#28057 = CARTESIAN_POINT ( 'NONE',  ( 11.61527771782819940, 108.7351862821014663, -4.622313124798573369 ) ) ;
#28058 = CARTESIAN_POINT ( 'NONE',  ( 13.44051670066911264, 5.407089921784856479, -1.115624999385556038 ) ) ;
#28059 = CARTESIAN_POINT ( 'NONE',  ( -41.48586230271182984, 205.8500491399821613, 7.418979330068642852 ) ) ;
#28060 = CARTESIAN_POINT ( 'NONE',  ( 20.99999999999999645, 244.2343750006145626, -6.646953231504538984 ) ) ;
#28061 = FACE_OUTER_BOUND ( 'NONE', #37448, .T. ) ;
#28062 = CARTESIAN_POINT ( 'NONE',  ( -66.42336230271182274, 215.6869285224997270, 3.149950860017831200 ) ) ;
#28063 = CARTESIAN_POINT ( 'NONE',  ( 10.69584247140445221, 126.8476862821014635, -6.932735513423970097 ) ) ;
#28064 = CARTESIAN_POINT ( 'NONE',  ( 13.56230152254411259, -5.196152422706632912, -0.7124999987710434191 ) ) ;
#28065 = VECTOR ( 'NONE', #7076, 1000.000000000000000 ) ;
#28066 = CARTESIAN_POINT ( 'NONE',  ( -43.47247103062156981, 206.6499508600178672, 5.571401726697986057 ) ) ;
#28067 = CARTESIAN_POINT ( 'NONE',  ( 27.00000000000000355, 195.3875000012290286, -3.306546357697854128E-15 ) ) ;
#28068 = CARTESIAN_POINT ( 'NONE',  ( -7.234628195640302017, 199.6424038105676857, 27.00000000000000711 ) ) ;
#28069 = CARTESIAN_POINT ( 'NONE',  ( 0.1745138560725837118, 116.2101862821014748, -15.50000000000000533 ) ) ;
#28070 = CARTESIAN_POINT ( 'NONE',  ( 5.438367727407757144E-14, 198.0875000000000057, -27.00000000000000000 ) ) ;
#28071 = CARTESIAN_POINT ( 'NONE',  ( -7.228626920339069173, 11.27268628210143042, 10.49813415415989581 ) ) ;
#28072 = CARTESIAN_POINT ( 'NONE',  ( 22.56230152254412147, 7.347880794884125653E-16, -8.775000000000032330 ) ) ;
#28073 = ORIENTED_EDGE ( 'NONE', *, *, #12017, .F. ) ;
#28074 = CARTESIAN_POINT ( 'NONE',  ( 13.56230152254411614, -5.196152422706638241, -8.025000000000058975 ) ) ;
#28075 = CARTESIAN_POINT ( 'NONE',  ( 3.796722387233379514, 79.98518628210145209, -8.710071997420127943 ) ) ;
#28076 =( NAMED_UNIT ( * ) PLANE_ANGLE_UNIT ( ) SI_UNIT ( $, .RADIAN. ) );
#28077 = CARTESIAN_POINT ( 'NONE',  ( -8.843639120294245259, 126.6648137178985820, -3.474262827703533230 ) ) ;
#28078 = CARTESIAN_POINT ( 'NONE',  ( 27.24356964375000700, 195.0406250006145399, 15.72908226750537075 ) ) ;
#28079 = CARTESIAN_POINT ( 'NONE',  ( 20.99999999999999645, -6.928203230275506996, -2.137499999999987743 ) ) ;
#28080 = CARTESIAN_POINT ( 'NONE',  ( -13.62178482187498396, 197.2343750006145626, 23.59362340125808188 ) ) ;
#28081 = CARTESIAN_POINT ( 'NONE',  ( 20.99999999999999645, -6.928203230275506996, -1.631249998770951004 ) ) ;
#28082 = AXIS2_PLACEMENT_3D ( 'NONE', #28910, #26072, #100 ) ;
#28083 = CARTESIAN_POINT ( 'NONE',  ( 22.60769515458672885, 242.0325961894323257, 5.999999999999997335 ) ) ;
#28084 = CARTESIAN_POINT ( 'NONE',  ( 9.465287035748106703, 56.80231371789854933, -2.064181346179063237 ) ) ;
#28085 = CARTESIAN_POINT ( 'NONE',  ( 15.00000000000000178, -3.464101615137757051, -8.512500000000017053 ) ) ;
#28086 = ORIENTED_EDGE ( 'NONE', *, *, #34278, .T. ) ;
#28087 = CARTESIAN_POINT ( 'NONE',  ( 21.00000000000000000, 242.0687500012290343, 6.928203230275506996 ) ) ;
#28088 = CARTESIAN_POINT ( 'NONE',  ( 12.53471296425189330, 57.37731371789855928, 2.311890736173451533 ) ) ;
#28089 = CARTESIAN_POINT ( 'NONE',  ( 22.80587116629411426, 7.646167579472024665E-16, -6.721874999385535787 ) ) ;
#28090 = CARTESIAN_POINT ( 'NONE',  ( -27.24356964374999990, 199.3156250006145171, -15.72908226750537786 ) ) ;
#28091 = CARTESIAN_POINT ( 'NONE',  ( 26.75643035624999655, -3.323476615752267715, -6.815624999385487826 ) ) ;
#28092 = CARTESIAN_POINT ( 'NONE',  ( -0.1745138560722763466, 27.18981371789855217, -12.50000000000000355 ) ) ;
#28093 = ORIENTED_EDGE ( 'NONE', *, *, #28167, .T. ) ;
#28094 = CARTESIAN_POINT ( 'NONE',  ( 13.44051670066911086, -5.407089921784865361, -0.5718749993855187785 ) ) ;
#28095 = CARTESIAN_POINT ( 'NONE',  ( 12.46528703574805874, 8.397686282101442856, 2.660918448318279950 ) ) ;
#28096 = EDGE_CURVE ( 'NONE', #26056, #27158, #22422, .T. ) ;
#28097 = CARTESIAN_POINT ( 'NONE',  ( -43.86086230271183695, 213.1499508600178387, -5.686928522499747451 ) ) ;
#28098 = CARTESIAN_POINT ( 'NONE',  ( 27.68897169117423829, 5.196152422706630247, 160.8764360188296223 ) ) ;
#28099 = AXIS2_PLACEMENT_3D ( 'NONE', #32877, #18303, #6924 ) ;
#28100 = SURFACE_STYLE_USAGE ( .BOTH. , #13329 ) ;
#28101 = CARTESIAN_POINT ( 'NONE',  ( 20.99999999999999645, 0.000000000000000000, -8.000000000000000000 ) ) ;
#28102 = CARTESIAN_POINT ( 'NONE',  ( 7.228626920338837358, 58.52731371789855785, 10.49813415416005036 ) ) ;
#28103 = CARTESIAN_POINT ( 'NONE',  ( -64.84002896937849414, 206.1606490808709111, 2.350049139982143931 ) ) ;
#28104 = AXIS2_PLACEMENT_3D ( 'NONE', #28953, #331, #21012 ) ;
#28105 = CARTESIAN_POINT ( 'NONE',  ( -47.82663769728823411, 204.3130714775002730, 3.149950860017883603 ) ) ;
#28106 = CARTESIAN_POINT ( 'NONE',  ( 27.00000000000001421, 195.8000000012290513, 15.58845726811988897 ) ) ;
#28107 = DIRECTION ( 'NONE',  ( 0.000000000000000000, -1.000000000000000000, 0.000000000000000000 ) ) ;
#28108 = CARTESIAN_POINT ( 'NONE',  ( -3.257655550456946880, 36.10231371789854649, -15.46528703574811736 ) ) ;
#28109 = CARTESIAN_POINT ( 'NONE',  ( -68.21205436395490551, 216.1378603801730094, 6.307003348497944195 ) ) ;
#28110 = CARTESIAN_POINT ( 'NONE',  ( -8.715434833791929847, 23.06018628210145138, -8.962234695871762469 ) ) ;
#28111 = CARTESIAN_POINT ( 'NONE',  ( -7.228626920339069173, 75.67268628210146630, 10.49813415415989581 ) ) ;
#28112 = CARTESIAN_POINT ( 'NONE',  ( 13.23911966647218996, 7.247686282101430066, -8.632099005475504683 ) ) ;
#28113 = EDGE_CURVE ( 'NONE', #5775, #4383, #5626, .T. ) ;
#28114 = CARTESIAN_POINT ( 'NONE',  ( 16.56230152254411436, -6.928203230275514990, -2.137500000000051692 ) ) ;
#28115 = ORIENTED_EDGE ( 'NONE', *, *, #29776, .F. ) ;
#28116 = CARTESIAN_POINT ( 'NONE',  ( -11.08355503943142573, 29.96018628210143575, 10.83675517735155402 ) ) ;
#28117 = CARTESIAN_POINT ( 'NONE',  ( -6.000000000000000888, -30.00000000000000000, 20.00000000000000711 ) ) ;
#28118 = CARTESIAN_POINT ( 'NONE',  ( -27.24356964374999635, 197.6468750006145285, 15.72908226750539384 ) ) ;
#28119 = CARTESIAN_POINT ( 'NONE',  ( 0.000000000000000000, 210.0000000000000284, 0.000000000000000000 ) ) ;
#28120 = SURFACE_STYLE_FILL_AREA ( #36647 ) ;
#28121 = CARTESIAN_POINT ( 'NONE',  ( 1.069080835302379631E-14, 195.6124999999999829, 27.00000000000000000 ) ) ;
#28122 = EDGE_CURVE ( 'NONE', #815, #2357, #8011, .T. ) ;
#28123 = CARTESIAN_POINT ( 'NONE',  ( 19.39230484541326049, 247.6575961894323541, -5.999999999999994671 ) ) ;
#28124 = CARTESIAN_POINT ( 'NONE',  ( 26.75643035624999655, 247.3843750006145399, -7.049594010296217766E-16 ) ) ;
#28125 = CARTESIAN_POINT ( 'NONE',  ( -5.529263428287297444, 118.3273137178985763, -7.954856959092311719 ) ) ;
#28126 = CARTESIAN_POINT ( 'NONE',  ( 15.24356964374999990, 240.8218750006145683, -3.323476615752268604 ) ) ;
#28127 = VERTEX_POINT ( 'NONE', #2128 ) ;
#28128 = CARTESIAN_POINT ( 'NONE',  ( 20.99999999999999645, 185.0294372515228645, 0.000000000000000000 ) ) ;
#28129 =( NAMED_UNIT ( * ) PLANE_ANGLE_UNIT ( ) SI_UNIT ( $, .RADIAN. ) );
#28130 = CARTESIAN_POINT ( 'NONE',  ( 23.99999999999999645, 248.1062500012290570, -5.196152422706631135 ) ) ;
#28131 = CARTESIAN_POINT ( 'NONE',  ( -10.49813415416004858, 116.0273137178985650, 7.228626920338840023 ) ) ;
#28132 = CARTESIAN_POINT ( 'NONE',  ( 10.31873187879410736, -3.604726614523240613, -8.203124999385503102 ) ) ;
#28133 = CARTESIAN_POINT ( 'NONE',  ( 30.76988640036921652, 7.209453229046475009, 161.6703125482654286 ) ) ;
#28134 = CARTESIAN_POINT ( 'NONE',  ( 24.00000000000000000, 240.7562500012290627, 5.196152422706629359 ) ) ;
#28135 = CARTESIAN_POINT ( 'NONE',  ( -27.24356964375000345, 199.4093750006145456, 0.000000000000000000 ) ) ;
#28136 = VERTEX_POINT ( 'NONE', #11408 ) ;
#28137 = VERTEX_POINT ( 'NONE', #13705 ) ;
#28138 = ORIENTED_EDGE ( 'NONE', *, *, #12715, .T. ) ;
#28139 = CARTESIAN_POINT ( 'NONE',  ( 21.00000000000000000, -6.928203230275506996, -4.331249998770957177 ) ) ;
#28140 = CARTESIAN_POINT ( 'NONE',  ( 15.24356964374999990, 3.323476615752268604, -1.978124999385461935 ) ) ;
#28141 = CARTESIAN_POINT ( 'NONE',  ( 10.56230152254514643, -3.464101615138358792, -4.462500000000011013 ) ) ;
#28142 = LINE ( 'NONE', #25113, #11147 ) ;
#28143 = CARTESIAN_POINT ( 'NONE',  ( 26.75643035624999655, 248.2093750006145285, -3.323476615752271712 ) ) ;
#28144 = CARTESIAN_POINT ( 'NONE',  ( 12.53471296425194836, 63.02268628210145351, -2.311890736173178418 ) ) ;
#28145 = CARTESIAN_POINT ( 'NONE',  ( -63.25669563604516554, 209.8844732041982013, -6.500000000000000888 ) ) ;
#28146 = CARTESIAN_POINT ( 'NONE',  ( 15.15359421270861340, 225.5904154327739661, 1.363118671454984554 ) ) ;
#28147 = CARTESIAN_POINT ( 'NONE',  ( -39.90252896937850124, 207.6499508600178387, -3.839350919129087547 ) ) ;
#28148 = CARTESIAN_POINT ( 'NONE',  ( 37.03711979530527287, 3.464101615137755275, 164.4628385719782671 ) ) ;
#28149 = CARTESIAN_POINT ( 'NONE',  ( -4.622313124798826500, 124.3648137178985706, 11.61527771782809637 ) ) ;
#28150 = EDGE_CURVE ( 'NONE', #17896, #6008, #25230, .T. ) ;
#28151 = CARTESIAN_POINT ( 'NONE',  ( -36.34747103062156981, 213.3500491399821328, -5.571401726697985168 ) ) ;
#28152 = CARTESIAN_POINT ( 'NONE',  ( -55.14955436395491262, 216.3070033484980002, -6.137860380172975638 ) ) ;
#28153 = CARTESIAN_POINT ( 'NONE',  ( 23.87821517812499650, 4.985214923628404904, -3.103124999385475924 ) ) ;
#28154 = CARTESIAN_POINT ( 'NONE',  ( 13.62178482187499640, 195.6031250006145115, -23.59362340125807123 ) ) ;
#28155 = CARTESIAN_POINT ( 'NONE',  ( -5.770363421894122880, 87.56481371789857349, 14.38691631536194393 ) ) ;
#28156 = CARTESIAN_POINT ( 'NONE',  ( -65.63169563604516554, 210.1155267958018271, 8.500000000000003553 ) ) ;
#28157 = EDGE_CURVE ( 'NONE', #17042, #23387, #19587, .T. ) ;
#28158 = ORIENTED_EDGE ( 'NONE', *, *, #2412, .T. ) ;
#28159 = LINE ( 'NONE', #37240, #21082 ) ;
#28160 = CARTESIAN_POINT ( 'NONE',  ( -12.53471296425194836, 113.6226862821014407, 2.311890736173176641 ) ) ;
#28161 = CARTESIAN_POINT ( 'NONE',  ( 15.53471296425195369, 63.02268628210144641, -2.908627838312120684 ) ) ;
#28162 = VECTOR ( 'NONE', #31220, 1000.000000000000000 ) ;
#28163 = CARTESIAN_POINT ( 'NONE',  ( 25.13834520420595098, 0.000000000000000000, 166.1437816049835874 ) ) ;
#28164 = CARTESIAN_POINT ( 'NONE',  ( 27.94596069312478903, -5.407089921784865361, 165.2111578762278157 ) ) ;
#28165 = CARTESIAN_POINT ( 'NONE',  ( -5.770363421893818234, 88.03518628210144925, -14.38691631536207005 ) ) ;
#28166 = CARTESIAN_POINT ( 'NONE',  ( -47.62872103062156270, 203.4690446883607535, 1.626142955000567936 ) ) ;
#28167 = EDGE_CURVE ( 'NONE', #22802, #6301, #9518, .T. ) ;
#28168 = CARTESIAN_POINT ( 'NONE',  ( 13.44051670066911619, -5.407089921784859143, -7.715624999385550353 ) ) ;
#28169 = CARTESIAN_POINT ( 'NONE',  ( 6.594114490232313663, 27.66018628210143859, 6.840914352312096547 ) ) ;
#28170 = FACE_OUTER_BOUND ( 'NONE', #30800, .T. ) ;
#28171 = CARTESIAN_POINT ( 'NONE',  ( -56.53497103062156270, 204.4285982733020148, -3.350049139982115509 ) ) ;
#28172 =( NAMED_UNIT ( * ) SI_UNIT ( $, .STERADIAN. ) SOLID_ANGLE_UNIT ( ) );
#28173 = CARTESIAN_POINT ( 'NONE',  ( 4.944772684328679446, 61.58518628210145351, -11.48171059495397373 ) ) ;
#28174 = CARTESIAN_POINT ( 'NONE',  ( -13.50000000000000533, 198.5749999999999886, -23.38268590217984411 ) ) ;
#28175 = LINE ( 'NONE', #16815, #34726 ) ;
#28177 = CARTESIAN_POINT ( 'NONE',  ( 10.31873187879411091, -3.604726614523244610, -0.6093749993855241964 ) ) ;
#28176 = CARTESIAN_POINT ( 'NONE',  ( 5.233372021372432847, 27.94768628210144001, 8.152565276336710909 ) ) ;
#28178 = ORIENTED_EDGE ( 'NONE', *, *, #18405, .T. ) ;
#28179 = CARTESIAN_POINT ( 'NONE',  ( 26.99999999999999645, 3.464101615137755275, -3.337499999999986589 ) ) ;
#28180 = DIRECTION ( 'NONE',  ( -0.000000000000000000, -0.000000000000000000, 1.000000000000000000 ) ) ;
#28181 = CARTESIAN_POINT ( 'NONE',  ( 27.50146640511176344, 5.407089921784862696, 160.1305649159599227 ) ) ;
#28182 = CARTESIAN_POINT ( 'NONE',  ( 22.80587116629411071, -3.604726614523235284, -1.303124999385484095 ) ) ;
#28183 = CARTESIAN_POINT ( 'NONE',  ( 37.60741370336351252, 7.646167579472015790E-16, 168.1866795212929446 ) ) ;
#28184 = CARTESIAN_POINT ( 'NONE',  ( 15.00000000000000000, 242.7625000000000171, -3.464101615137752166 ) ) ;
#28185 = CARTESIAN_POINT ( 'NONE',  ( 20.99999999999999289, 243.6437500012290229, -5.999999999999997335 ) ) ;
#28186 = ADVANCED_FACE ( 'NONE', ( #12148 ), #10500, .F. ) ;
#28187 = CARTESIAN_POINT ( 'NONE',  ( 10.69584247140445221, 80.84768628210144925, -6.932735513423970097 ) ) ;
#28188 = VERTEX_POINT ( 'NONE', #24246 ) ;
#28189 = ORIENTED_EDGE ( 'NONE', *, *, #11222, .T. ) ;
#28190 = CIRCLE ( 'NONE', #31803, 7.500000000000000000 ) ;
#28191 = CARTESIAN_POINT ( 'NONE',  ( 13.50000000000001421, 195.7625000012290570, 23.38268590217984055 ) ) ;
#28192 = DIRECTION ( 'NONE',  ( -0.000000000000000000, 1.000000000000000000, -0.000000000000000000 ) ) ;
#28193 = CARTESIAN_POINT ( 'NONE',  ( 11.08355503943118769, 49.03981371789855359, 10.83675517735179028 ) ) ;
#28194 = CARTESIAN_POINT ( 'NONE',  ( 23.87821517812500005, -4.985214923628404016, -8.653124999385475746 ) ) ;
#28195 = VECTOR ( 'NONE', #442, 1000.000000000000000 ) ;
#28196 = CARTESIAN_POINT ( 'NONE',  ( 23.87821517812499650, 242.5093750006145399, -4.985214923628404904 ) ) ;
#28197 = APPLICATION_CONTEXT ( 'automotive_design' ) ;
#28198 = CARTESIAN_POINT ( 'NONE',  ( -53.56622103062157692, 211.0902445701382533, 4.530955311639240257 ) ) ;
#28199 = CARTESIAN_POINT ( 'NONE',  ( 34.35249135386247588, -5.196152422706629359, 168.1985348098161808 ) ) ;
#28200 = ADVANCED_FACE ( 'NONE', ( #29924 ), #21782, .T. ) ;
#28201 = CARTESIAN_POINT ( 'NONE',  ( -9.500000000000005329, 43.28981371789856070, 0.1745138560723101806 ) ) ;
#28202 = CARTESIAN_POINT ( 'NONE',  ( -66.23288769728823411, 203.5309553116391612, -1.857196546604028775 ) ) ;
#28203 =( BOUNDED_CURVE ( )  B_SPLINE_CURVE ( 2, ( #31585, #25898, #17006, #17380, #10941, #23064, #2957, #3144, #11675 ),
 .UNSPECIFIED., .F., .F. ) 
 B_SPLINE_CURVE_WITH_KNOTS ( ( 3, 2, 2, 2, 3 ),
 ( 0.5625000000000000000, 0.5694444444444444198, 0.5833333333333333703, 0.5972222222222222099, 0.6041666666666667407 ),
 .UNSPECIFIED. ) 
 CURVE ( )  GEOMETRIC_REPRESENTATION_ITEM ( )  RATIONAL_B_SPLINE_CURVE ( ( 0.9330127018922194093, 0.9330127018922194093, 1.000000000000000000, 0.8660254037844387076, 1.000000000000000000, 0.8660254037844387076, 1.000000000000000000, 0.9330127018922187432, 0.9330127018922192983 ) ) 
 REPRESENTATION_ITEM ( '' )  );
#28204 = CARTESIAN_POINT ( 'NONE',  ( -8.843639120294245259, 89.86481371789855643, -3.474262827703533230 ) ) ;
#28205 = CARTESIAN_POINT ( 'NONE',  ( 13.62178482187501416, 199.1093750006145342, 23.59362340125806767 ) ) ;
#28206 = CARTESIAN_POINT ( 'NONE',  ( -12.53471296425189152, 6.777313717898553413, -2.311890736173453753 ) ) ;
#28207 = CARTESIAN_POINT ( 'NONE',  ( -11.48171059495397373, 68.48518628210145209, -4.944772684328680334 ) ) ;
#28208 = CARTESIAN_POINT ( 'NONE',  ( 13.56230152254410370, 5.196152422706630247, -9.862499998771006915 ) ) ;
#28209 = CARTESIAN_POINT ( 'NONE',  ( 16.56230152254410726, 0.000000000000000000, -10.00000000000000000 ) ) ;
#28210 = CARTESIAN_POINT ( 'NONE',  ( 27.59788244552635206, -5.407089921784859143, 161.2326053007238897 ) ) ;
#28211 = CARTESIAN_POINT ( 'NONE',  ( 15.00000000000000000, 3.464101615137752166, -0.4312499987709516591 ) ) ;
#28212 = CARTESIAN_POINT ( 'NONE',  ( 10.31873187879410558, 0.000000000000000000, -6.496874999385504168 ) ) ;
#28213 = DIRECTION ( 'NONE',  ( 1.000000000000000000, 0.000000000000000000, 0.000000000000000000 ) ) ;
#28214 = CARTESIAN_POINT ( 'NONE',  ( -27.00000000000000355, 195.5750000012290570, -15.58845726811989429 ) ) ;
#28215 = CARTESIAN_POINT ( 'NONE',  ( 3.474262827703335166, 74.23518628210142367, 8.843639120294326972 ) ) ;
#28216 = DIRECTION ( 'NONE',  ( -0.000000000000000000, -0.000000000000000000, 1.000000000000000000 ) ) ;
#28217 = AXIS2_PLACEMENT_3D ( 'NONE', #12086, #35022, #6217 ) ;
#28218 =( BOUNDED_CURVE ( )  B_SPLINE_CURVE ( 2, ( #3080, #2890, #8588, #237, #26200, #11612, #23187, #34920, #422 ),
 .UNSPECIFIED., .F., .F. ) 
 B_SPLINE_CURVE_WITH_KNOTS ( ( 3, 2, 2, 2, 3 ),
 ( 0.6041666666666667407, 0.6111111111111111605, 0.6250000000000000000, 0.6388888888888888395, 0.6458333333333333703 ),
 .UNSPECIFIED. ) 
 CURVE ( )  GEOMETRIC_REPRESENTATION_ITEM ( )  RATIONAL_B_SPLINE_CURVE ( ( 0.9330127018922192983, 0.9330127018922198534, 1.000000000000000000, 0.8660254037844387076, 1.000000000000000000, 0.8660254037844387076, 1.000000000000000000, 0.9330127018922187432, 0.9330127018922192983 ) ) 
 REPRESENTATION_ITEM ( '' )  );
#28219 = CARTESIAN_POINT ( 'NONE',  ( 7.228626920339068285, 117.0726862821014720, -10.49813415415989581 ) ) ;
#28220 = CARTESIAN_POINT ( 'NONE',  ( 26.99999999999999645, 7.347880794884117764E-16, -3.318749998770964549 ) ) ;
#28221 = CARTESIAN_POINT ( 'NONE',  ( 20.99999999999999289, 248.5937500012290400, -5.999999999999997335 ) ) ;
#28222 = ORIENTED_EDGE ( 'NONE', *, *, #24289, .T. ) ;
#28223 = CARTESIAN_POINT ( 'NONE',  ( 31.02481694790609268, -7.209453229046475009, 164.5841820401837765 ) ) ;
#28224 = CARTESIAN_POINT ( 'NONE',  ( 15.24356964374999990, 3.323476615752268604, -4.228124999385472371 ) ) ;
#28225 = CARTESIAN_POINT ( 'NONE',  ( 27.24356964374999279, 196.9718750006145456, -15.72908226750539207 ) ) ;
#28226 = CARTESIAN_POINT ( 'NONE',  ( 25.10732745429168489, -3.604726614523244610, 168.5838953488872676 ) ) ;
#28227 = CARTESIAN_POINT ( 'NONE',  ( 31.13512343476753230, 6.928203230275514990, 165.8449909543439560 ) ) ;
#28228 = CYLINDRICAL_SURFACE ( 'NONE', #7766, 8.000000000000000000 ) ;
#28229 = CARTESIAN_POINT ( 'NONE',  ( 26.75643035624999655, 241.4968750006145228, 3.323476615752267715 ) ) ;
#28230 = CARTESIAN_POINT ( 'NONE',  ( 34.01258395714663152, 5.196152422706631135, 164.3133754872583836 ) ) ;
#28231 = CARTESIAN_POINT ( 'NONE',  ( -12.46528703574811558, 135.0023137178985735, 2.660918448318003726 ) ) ;
#28232 = CARTESIAN_POINT ( 'NONE',  ( 2.660918448318279950, 134.8976862821014606, -12.46528703574805874 ) ) ;
#28234 = ORIENTED_EDGE ( 'NONE', *, *, #32700, .F. ) ;
#28233 = ORIENTED_EDGE ( 'NONE', *, *, #31699, .T. ) ;
#28235 = CARTESIAN_POINT ( 'NONE',  ( 26.75643035624999655, 245.4343750006145228, 3.323476615752267715 ) ) ;
#28236 = AXIS2_PLACEMENT_3D ( 'NONE', #12924, #4759, #24666 ) ;
#28237 = CARTESIAN_POINT ( 'NONE',  ( 11.61527771782809637, 11.66481371789854293, 4.622313124798827388 ) ) ;
#28238 = ADVANCED_FACE ( 'NONE', ( #15528, #29544 ), #1108, .T. ) ;
#28239 = CARTESIAN_POINT ( 'NONE',  ( 18.12178482187500350, -4.985214923628407568, -4.565624999385481608 ) ) ;
#28240 = CARTESIAN_POINT ( 'NONE',  ( -6.092822981423666739, 118.6148137178985706, -14.25334919248795096 ) ) ;
#28241 = CARTESIAN_POINT ( 'NONE',  ( 26.99999999999999645, 244.4124999999999943, -3.464101615137755275 ) ) ;
#28242 = CARTESIAN_POINT ( 'NONE',  ( 15.24356964374999990, 0.000000000000000000, -2.053124999385480542 ) ) ;
#28243 = CARTESIAN_POINT ( 'NONE',  ( 10.31873187879410736, 3.604726614523240613, -7.884374999385513227 ) ) ;
#28244 = CARTESIAN_POINT ( 'NONE',  ( -27.00000000000000355, 199.1750000012290513, -15.58845726811989429 ) ) ;
#28245 = CARTESIAN_POINT ( 'NONE',  ( -4.622313124798576922, 106.4351862821014549, -11.61527771782819762 ) ) ;
#28246 = CARTESIAN_POINT ( 'NONE',  ( 19.68408634441910365, 5.407089921784857367, -3.440624999385522020 ) ) ;
#28247 = ADVANCED_FACE ( 'NONE', ( #1294 ), #35602, .F. ) ;
#28248 = CARTESIAN_POINT ( 'NONE',  ( -36.93377896937849414, 207.8379586601372750, 8.530955311639258909 ) ) ;
#28249 = CARTESIAN_POINT ( 'NONE',  ( 20.99999999999999645, 244.0093750006145115, 6.646953231504538984 ) ) ;
#28250 = LINE ( 'NONE', #2279, #2470 ) ;
#28251 = CARTESIAN_POINT ( 'NONE',  ( -38.51711230271182984, 214.4690446883608104, -1.321298161741814914 ) ) ;
#28252 = CARTESIAN_POINT ( 'NONE',  ( -12.50000000000000355, 123.1101862821014663, -0.1745138560725492671 ) ) ;
#28253 = CARTESIAN_POINT ( 'NONE',  ( 22.56230152254410370, -3.464101615137751278, -1.949999998771005272 ) ) ;
#28254 = CARTESIAN_POINT ( 'NONE',  ( -45.25372103062155560, 216.5309553116391612, -1.626142955000564383 ) ) ;
#28255 = CARTESIAN_POINT ( 'NONE',  ( 0.000000000000000000, 141.0000000000000000, 0.000000000000000000 ) ) ;
#28256 =( LENGTH_UNIT ( ) NAMED_UNIT ( * ) SI_UNIT ( .MILLI., .METRE. ) );
#28257 = CARTESIAN_POINT ( 'NONE',  ( -6.092822981423970496, 112.1851862821014691, 14.25334919248782661 ) ) ;
#28258 = CARTESIAN_POINT ( 'NONE',  ( 21.00000000000000355, 0.000000000000000000, 50.00000000000001421 ) ) ;
#28259 = CARTESIAN_POINT ( 'NONE',  ( -5.233372021372430183, 124.5476862821014663, -8.152565276336710909 ) ) ;
#28260 = CARTESIAN_POINT ( 'NONE',  ( 16.56230152254411436, 7.209453229046475009, -0.2531249993855048674 ) ) ;
#28261 = CARTESIAN_POINT ( 'NONE',  ( 22.60769515458672174, 245.6888461906614225, 6.000000000000004441 ) ) ;
#28262 = VERTEX_POINT ( 'NONE', #12676 ) ;
#28263 = DIRECTION ( 'NONE',  ( 0.000000000000000000, 0.000000000000000000, -1.000000000000000000 ) ) ;
#28264 = CARTESIAN_POINT ( 'NONE',  ( 8.710071997420127943, 73.08518628210143220, 3.796722387233375073 ) ) ;
#28265 = DIRECTION ( 'NONE',  ( 1.000000000000000000, 0.000000000000000000, 0.000000000000000000 ) ) ;
#28266 = CARTESIAN_POINT ( 'NONE',  ( -1.926257025242585782E-15, 196.9906250006145569, -31.45816453501075927 ) ) ;
#28267 = CARTESIAN_POINT ( 'NONE',  ( 18.00000000000000000, 246.8312500012290513, -5.196152422706630247 ) ) ;
#28268 = CARTESIAN_POINT ( 'NONE',  ( -13.62178482187500528, 197.9843750006145626, -23.59362340125807123 ) ) ;
#28269 = DIRECTION ( 'NONE',  ( 0.000000000000000000, 0.000000000000000000, -1.000000000000000000 ) ) ;
#28270 = CARTESIAN_POINT ( 'NONE',  ( 2.064181346179061460, 49.90231371789854364, 9.465287035748106703 ) ) ;
#28271 = CARTESIAN_POINT ( 'NONE',  ( 15.00000000000000178, -3.464101615137757051, -9.862500000000006040 ) ) ;
#28272 = ORIENTED_EDGE ( 'NONE', *, *, #29776, .T. ) ;
#28273 = CARTESIAN_POINT ( 'NONE',  ( 26.99999999999999645, 241.3187500012290627, -3.464101615137755275 ) ) ;
#28274 = CARTESIAN_POINT ( 'NONE',  ( 6.932735513424201024, 64.85231371789855359, -10.69584247140429412 ) ) ;
#28275 = CARTESIAN_POINT ( 'NONE',  ( 19.68408634441911431, -5.407089921784861808, -5.446874999385537208 ) ) ;
#28276 = CARTESIAN_POINT ( 'NONE',  ( 18.12178482187499640, 4.985214923628404904, -7.978124999385494576 ) ) ;
#28277 = CARTESIAN_POINT ( 'NONE',  ( -12.53471296425189152, 25.17731371789855288, -2.311890736173453753 ) ) ;
#28278 = EDGE_LOOP ( 'NONE', ( #34567, #32597, #13750, #23531 ) ) ;
#28279 = CARTESIAN_POINT ( 'NONE',  ( 22.80587116629411071, -3.604726614523238837, -1.359374999385495775 ) ) ;
#28280 = AXIS2_PLACEMENT_3D ( 'NONE', #18193, #32956, #30308 ) ;
#28281 = CARTESIAN_POINT ( 'NONE',  ( -2.660918448318275509, 10.69768628210143646, 12.46528703574805874 ) ) ;
#28282 = CARTESIAN_POINT ( 'NONE',  ( 25.14327919817509027, 0.000000000000000000, 168.9948256618500864 ) ) ;
#28283 = CARTESIAN_POINT ( 'NONE',  ( -44.25669563604516554, 209.8844732041982013, -6.500000000000000888 ) ) ;
#28284 = DIRECTION ( 'NONE',  ( -0.000000000000000000, -1.000000000000000000, -0.000000000000000000 ) ) ;
#28285 = SURFACE_SIDE_STYLE ('',( #25626 ) ) ;
#28286 = DIRECTION ( 'NONE',  ( -1.000000000000000000, 0.000000000000000000, 0.000000000000000000 ) ) ;
#28287 = CARTESIAN_POINT ( 'NONE',  ( -33.18080436395489841, 205.4999999999999716, -0.1155267958017894420 ) ) ;
#28288 = CARTESIAN_POINT ( 'NONE',  ( -43.86830436395490551, 209.8844732041982581, 6.500000000000000888 ) ) ;
#28289 = ORIENTED_EDGE ( 'NONE', *, *, #19362, .T. ) ;
#28290 = CARTESIAN_POINT ( 'NONE',  ( -28.99999999999999289, 201.9999999999999432, 0.5242534236750171495 ) ) ;
#28291 = CARTESIAN_POINT ( 'NONE',  ( -13.66544594067261720, 216.1537252680216739, -5.164798763356904132 ) ) ;
#28292 = CARTESIAN_POINT ( 'NONE',  ( 14.38691631536194393, 39.26481371789855501, 5.770363421894124656 ) ) ;
#28293 = CARTESIAN_POINT ( 'NONE',  ( -31.19419563604517265, 201.5000000000000000, 0.1155267958018195706 ) ) ;
#28294 = PRODUCT ( 'handle', 'handle', '', ( #15295 ) ) ;
#28295 = CARTESIAN_POINT ( 'NONE',  ( -12.53471296425194836, 12.42268628210144321, 2.311890736173176641 ) ) ;
#28296 = CARTESIAN_POINT ( 'NONE',  ( -12.53471296425194836, 58.42268628210145209, 2.311890736173176641 ) ) ;
#28297 = CARTESIAN_POINT ( 'NONE',  ( -15.50000000000000533, 12.71018628210143753, -0.1745138560725808530 ) ) ;
#28298 = CARTESIAN_POINT ( 'NONE',  ( 19.56230152254412502, -5.196152422706635576, -1.200000000000062128 ) ) ;
#28299 = CARTESIAN_POINT ( 'NONE',  ( 10.56230152254410903, 0.000000000000000000, -5.551115123125782702E-14 ) ) ;
#28300 = ORIENTED_EDGE ( 'NONE', *, *, #22225, .F. ) ;
#28301 = CARTESIAN_POINT ( 'NONE',  ( -15.53471296425195369, 21.62268628210143717, 2.908627838312118019 ) ) ;
#28302 = CARTESIAN_POINT ( 'NONE',  ( 27.24356964375000700, 195.9406250006145456, 15.72908226750537075 ) ) ;
#28303 = CARTESIAN_POINT ( 'NONE',  ( 27.24356964375000345, 198.7343750006145626, -3.336375036156643733E-15 ) ) ;
#28304 = DIRECTION ( 'NONE',  ( -0.000000000000000000, 0.000000000000000000, 1.000000000000000000 ) ) ;
#28305 = CARTESIAN_POINT ( 'NONE',  ( 24.66116751255602679, -3.464101615138098111, 160.6896156317068858 ) ) ;
#28306 = CARTESIAN_POINT ( 'NONE',  ( 20.99999999999999645, 192.3000000000000398, 0.000000000000000000 ) ) ;
#28307 = CARTESIAN_POINT ( 'NONE',  ( 15.24356964375000167, 248.0968750006145456, 3.323476615752272600 ) ) ;
#28308 = CARTESIAN_POINT ( 'NONE',  ( -9.465287035748106703, 107.4023137178985650, 2.064181346179061460 ) ) ;
#28309 = CARTESIAN_POINT ( 'NONE',  ( 26.75643035624999655, 241.4968750006144944, 3.323476615752267271 ) ) ;
#28310 = VECTOR ( 'NONE', #36606, 1000.000000000000227 ) ;
#28311 = ORIENTED_EDGE ( 'NONE', *, *, #25444, .F. ) ;
#28312 = CARTESIAN_POINT ( 'NONE',  ( -66.03497103062157692, 204.4285982733020148, -3.350049139982115509 ) ) ;
#28313 = CARTESIAN_POINT ( 'NONE',  ( -27.00000000000000355, 199.9625000000000057, -15.58845726811989429 ) ) ;
#28314 = CARTESIAN_POINT ( 'NONE',  ( 11.48171059495408208, 111.7148137178985650, -4.944772684328420986 ) ) ;
#28315 = CARTESIAN_POINT ( 'NONE',  ( 22.80587116629411071, -3.604726614523235284, -8.503124999385544669 ) ) ;
#28316 = CARTESIAN_POINT ( 'NONE',  ( 33.95496371662422064, 5.407089921784857367, 162.2574490005206655 ) ) ;
#28317 = DIRECTION ( 'NONE',  ( 1.000000000000000000, 0.000000000000000000, 0.000000000000000000 ) ) ;
#28318 = CARTESIAN_POINT ( 'NONE',  ( -13.50000000000000533, 195.4250000000000114, -23.38268590217984411 ) ) ;
#28319 = ORIENTED_EDGE ( 'NONE', *, *, #2507, .F. ) ;
#28320 = ORIENTED_EDGE ( 'NONE', *, *, #6300, .F. ) ;
#28321 = VERTEX_POINT ( 'NONE', #921 ) ;
#28322 = CARTESIAN_POINT ( 'NONE',  ( 15.00000000000000000, 0.000000000000000000, -5.793749998770941545 ) ) ;
#28323 = CARTESIAN_POINT ( 'NONE',  ( 20.99999999999999645, 6.646953231504538984, -2.053124999385488092 ) ) ;
#28324 = CARTESIAN_POINT ( 'NONE',  ( 24.62521576877984231, 3.464101615138150514, 160.2786853199683605 ) ) ;
#28325 = CARTESIAN_POINT ( 'NONE',  ( 20.99999999999998579, 248.0875000000000057, -5.999999999999997335 ) ) ;
#28326 = CARTESIAN_POINT ( 'NONE',  ( 18.12178482187499640, 249.6718750006145342, -4.985214923628404904 ) ) ;
#28327 = CARTESIAN_POINT ( 'NONE',  ( -12.53471296425194836, 58.42268628210145209, 2.311890736173176641 ) ) ;
#28328 = CARTESIAN_POINT ( 'NONE',  ( -57.71502896937850124, 215.5714017266979567, -3.350049139982168800 ) ) ;
#28329 = CARTESIAN_POINT ( 'NONE',  ( 5.840947329778490626, 215.6846447513327121, -1.929602858956001032 ) ) ;
#28330 = VECTOR ( 'NONE', #7709, 1000.000000000000000 ) ;
#28331 = CARTESIAN_POINT ( 'NONE',  ( -38.91294563604516554, 213.2096571498974527, -3.378800118222469617 ) ) ;
#28332 = CARTESIAN_POINT ( 'NONE',  ( -69.00000000000002842, 206.0000000000000000, 2.500000000000002220 ) ) ;
#28333 = CARTESIAN_POINT ( 'NONE',  ( 31.02726820322443047, 6.928203230275506996, 164.6122000166797932 ) ) ;
#28334 = CARTESIAN_POINT ( 'NONE',  ( -2.660918448318004614, 118.9023137178985507, -12.46528703574811558 ) ) ;
#28335 = CARTESIAN_POINT ( 'NONE',  ( -37.73288769728821279, 203.5309553116391612, -1.857196546604028775 ) ) ;
#28336 = CARTESIAN_POINT ( 'NONE',  ( -40.89955436395489841, 216.3070033484980002, -6.137860380172975638 ) ) ;
#28337 = ITEM_DEFINED_TRANSFORMATION ( 'NONE', 'NONE', #16623,  #17215 ) ;
#28338 = CARTESIAN_POINT ( 'NONE',  ( 26.75643035624999655, 7.049594010296217766E-16, -3.178124999385495641 ) ) ;
#28339 = CARTESIAN_POINT ( 'NONE',  ( -1.926257025242585782E-15, 195.6406250006145058, -31.45816453501075927 ) ) ;
#28340 = AXIS2_PLACEMENT_3D ( 'NONE', #5255, #302, #34437 ) ;
#28341 = CARTESIAN_POINT ( 'NONE',  ( -14.25334919248795096, 88.71481371789855075, 6.092822981423662299 ) ) ;
#28342 = CARTESIAN_POINT ( 'NONE',  ( -65.03794563604515133, 203.8621396198271043, 6.307003348498029460 ) ) ;
#28343 = ORIENTED_EDGE ( 'NONE', *, *, #13033, .F. ) ;
#28344 = CARTESIAN_POINT ( 'NONE',  ( -10.49813415415989581, 114.7726862821014606, -7.228626920339068285 ) ) ;
#28345 = CARTESIAN_POINT ( 'NONE',  ( -6.092822981423970496, 56.98518628210145209, 14.25334919248782661 ) ) ;
#28346 = FACE_BOUND ( 'NONE', #36827, .T. ) ;
#28347 = CARTESIAN_POINT ( 'NONE',  ( 24.55170959427540822, 3.604726614523240613, 162.2331541485523587 ) ) ;
#28348 = CARTESIAN_POINT ( 'NONE',  ( 8.632099005475504683, 92.34768628210142083, 13.23911966647218996 ) ) ;
#28349 = CARTESIAN_POINT ( 'NONE',  ( 10.31873187879410914, 0.000000000000000000, -7.790624999385542537 ) ) ;
#28350 = CARTESIAN_POINT ( 'NONE',  ( 9.534712964251941258, 26.22268628210144925, -1.715153634034235708 ) ) ;
#28351 = CARTESIAN_POINT ( 'NONE',  ( 22.56230152254411792, 7.347880794884125653E-16, -7.425000000000042455 ) ) ;
#28352 = CARTESIAN_POINT ( 'NONE',  ( -60.88913769728823411, 206.8500491399821044, -5.686928522499717253 ) ) ;
#28353 = EDGE_CURVE ( 'NONE', #28711, #17872, #26695, .T. ) ;
#28354 = CARTESIAN_POINT ( 'NONE',  ( 15.00000000000000000, 249.0999999999999943, 0.000000000000000000 ) ) ;
#28355 = CARTESIAN_POINT ( 'NONE',  ( 10.69584247140445221, 62.44768628210145778, -6.932735513423970097 ) ) ;
#28356 = CARTESIAN_POINT ( 'NONE',  ( 27.00000000000000355, 197.0749999999999886, -3.306546357697854128E-15 ) ) ;
#28357 = LINE ( 'NONE', #7538, #22039 ) ;
#28359 = CARTESIAN_POINT ( 'NONE',  ( 22.80587116629412847, -3.604726614523238837, -2.259374999385487026 ) ) ;
#28358 = CARTESIAN_POINT ( 'NONE',  ( -8.843639120294326972, 30.53518628210144570, 3.474262827703335166 ) ) ;
#28360 = CARTESIAN_POINT ( 'NONE',  ( 15.24356964374999990, 249.8593750006145342, 0.000000000000000000 ) ) ;
#28361 = ORIENTED_EDGE ( 'NONE', *, *, #14499, .T. ) ;
#28362 = CARTESIAN_POINT ( 'NONE',  ( 24.00000000000000000, -5.196152422706629359, -3.899999999999987033 ) ) ;
#28363 = CARTESIAN_POINT ( 'NONE',  ( 37.15151170766156952, 7.347880794884117764E-16, 165.7703441132237003 ) ) ;
#28364 = CARTESIAN_POINT ( 'NONE',  ( 28.41103595111929181, 5.957544813848101306, 159.5877724440177303 ) ) ;
#28365 = CARTESIAN_POINT ( 'NONE',  ( 13.44051670066911619, -5.407089921784859143, -0.9656249993855170466 ) ) ;
#28366 = CARTESIAN_POINT ( 'NONE',  ( 37.64663378759995283, 7.646167579472015790E-16, 168.6349671354342092 ) ) ;
#28367 = CARTESIAN_POINT ( 'NONE',  ( 26.99999999999999645, 243.4749999999999943, -7.347880794884117764E-16 ) ) ;
#28368 = CARTESIAN_POINT ( 'NONE',  ( 10.56230152254410903, 7.347880794884117764E-16, -10.00000000000000000 ) ) ;
#28369 = CARTESIAN_POINT ( 'NONE',  ( -12.50000000000000355, 95.51018628210144357, -0.1745138560725492671 ) ) ;
#28370 = ORIENTED_EDGE ( 'NONE', *, *, #29328, .F. ) ;
#28371 = ORIENTED_EDGE ( 'NONE', *, *, #12248, .T. ) ;
#28372 = CARTESIAN_POINT ( 'NONE',  ( -13.50000000000000533, 195.5375000012290343, -23.38268590217984411 ) ) ;
#28373 = CARTESIAN_POINT ( 'NONE',  ( 36.72335912141303993, 3.464101615138153178, 160.8765376588480649 ) ) ;
#28374 = CARTESIAN_POINT ( 'NONE',  ( 13.23911966647199812, 30.35231371789855359, 8.632099005475788900 ) ) ;
#28375 = CARTESIAN_POINT ( 'NONE',  ( 21.00000000000000000, 6.646953231504538984, -8.015624999385487115 ) ) ;
#28376 = CARTESIAN_POINT ( 'NONE',  ( 23.87821517812500005, 242.8093750006145228, 4.985214923628404016 ) ) ;
#28377 = CARTESIAN_POINT ( 'NONE',  ( -41.49330436395490551, 210.1155267958017703, -4.499999999999996447 ) ) ;
#28378 = EDGE_CURVE ( 'NONE', #9298, #25022, #14829, .T. ) ;
#28379 = CARTESIAN_POINT ( 'NONE',  ( 23.99999999999999645, 5.196152422706631135, -7.349999999999995204 ) ) ;
#28380 = CARTESIAN_POINT ( 'NONE',  ( 30.84342405831255007, 7.209453229046482114, 162.5108518247803318 ) ) ;
#28381 = CARTESIAN_POINT ( 'NONE',  ( 3.796722387233182339, 31.21481371789855430, 8.710071997420207879 ) ) ;
#28382 = CARTESIAN_POINT ( 'NONE',  ( 16.56230152254411081, -7.209453229046475009, -9.478124999385530103 ) ) ;
#28383 = CARTESIAN_POINT ( 'NONE',  ( -2.064181346179062349, 91.30231371789854222, -9.465287035748106703 ) ) ;
#28384 = CARTESIAN_POINT ( 'NONE',  ( 27.24356964374999635, 198.7718750006145569, -15.72908226750539029 ) ) ;
#28385 = CARTESIAN_POINT ( 'NONE',  ( -2.908627838312453306, 142.4773137178985678, 15.53471296425188797 ) ) ;
#28386 = CARTESIAN_POINT ( 'NONE',  ( 0.1745138560725515708, 70.21018628210144641, -12.50000000000000355 ) ) ;
#28387 = LINE ( 'NONE', #5634, #6849 ) ;
#28388 = DIRECTION ( 'NONE',  ( -0.000000000000000000, -1.000000000000000000, -0.000000000000000000 ) ) ;
#28389 = CARTESIAN_POINT ( 'NONE',  ( 36.86550044322413555, 3.604726614523238837, 159.7065721537869365 ) ) ;
#28390 = CARTESIAN_POINT ( 'NONE',  ( 13.44051670066911264, -5.407089921784865361, -10.02187499938553294 ) ) ;
#28391 = CARTESIAN_POINT ( 'NONE',  ( 22.80587116629412847, -3.604726614523238837, -9.009374999385519445 ) ) ;
#28392 = FILL_AREA_STYLE_COLOUR ( '', #14909 ) ;
#28393 = CARTESIAN_POINT ( 'NONE',  ( -3.796722387233375073, 75.38518628210142936, 8.710071997420127943 ) ) ;
#28394 = FACE_OUTER_BOUND ( 'NONE', #2090, .T. ) ;
#28395 = CARTESIAN_POINT ( 'NONE',  ( 2.660918448318279950, 116.4976862821014549, -12.46528703574805697 ) ) ;
#28396 = CARTESIAN_POINT ( 'NONE',  ( 24.00000000000000000, 248.7999999999999829, 5.196152422706629359 ) ) ;
#28397 = CARTESIAN_POINT ( 'NONE',  ( 10.56230152254477339, 3.464101615138135415, -3.524999998771014109 ) ) ;
#28398 = VERTEX_POINT ( 'NONE', #18574 ) ;
#28399 = CARTESIAN_POINT ( 'NONE',  ( 33.82423010250274586, -5.407089921784855591, 160.7631569533830600 ) ) ;
#28400 = CARTESIAN_POINT ( 'NONE',  ( 15.24356964375000167, -3.323476615752272600, -8.653124999385468641 ) ) ;
#28401 = CARTESIAN_POINT ( 'NONE',  ( 13.62178482187499640, 195.2093750006145569, -23.59362340125807123 ) ) ;
#28402 = CARTESIAN_POINT ( 'NONE',  ( 25.10079077358561150, 3.604726614523240613, 168.5091807465304043 ) ) ;
#28403 = CARTESIAN_POINT ( 'NONE',  ( 37.25609859885165775, -3.464101615137755275, 166.9657777497094457 ) ) ;
#28404 = CARTESIAN_POINT ( 'NONE',  ( 19.56230152254411792, 5.196152422706637353, -9.150000000000046541 ) ) ;
#28405 = CARTESIAN_POINT ( 'NONE',  ( 26.75643035624999655, 241.0843750006145285, -7.049594010296217766E-16 ) ) ;
#28406 = CARTESIAN_POINT ( 'NONE',  ( -27.24356964375000345, 199.3156250006145171, -15.72908226750537786 ) ) ;
#28407 = CARTESIAN_POINT ( 'NONE',  ( -12.50000000000000355, 126.0898137178985650, 0.1745138560722786503 ) ) ;
#28408 = CARTESIAN_POINT ( 'NONE',  ( -2.311890736173176641, 134.3226862821014436, -12.53471296425194659 ) ) ;
#28410 = EDGE_LOOP ( 'NONE', ( #30644, #13641, #37218, #15394 ) ) ;
#28409 = ORIENTED_EDGE ( 'NONE', *, *, #11135, .F. ) ;
#28411 = CARTESIAN_POINT ( 'NONE',  ( 15.24356964374999990, 244.7593750006145115, -3.323476615752268604 ) ) ;
#28412 = CARTESIAN_POINT ( 'NONE',  ( -8.715434833792127023, 14.53981371789855892, 8.962234695871568846 ) ) ;
#28413 = CARTESIAN_POINT ( 'NONE',  ( -13.04141134922778456, 106.8273137178985479, 8.927990412390377273 ) ) ;
#28414 =( BOUNDED_CURVE ( )  B_SPLINE_CURVE ( 2, ( #36954, #25404, #11001, #34119, #21830, #27694, #24847, #2832, #34491 ),
 .UNSPECIFIED., .F., .F. ) 
 B_SPLINE_CURVE_WITH_KNOTS ( ( 3, 2, 2, 2, 3 ),
 ( 0.9239130434782608647, 0.9275362318840579823, 0.9347826086956522174, 0.9420289855072463414, 0.9456521739130434590 ),
 .UNSPECIFIED. ) 
 CURVE ( )  GEOMETRIC_REPRESENTATION_ITEM ( )  RATIONAL_B_SPLINE_CURVE ( ( 0.9330127018922194093, 0.9330127018922194093, 1.000000000000000000, 0.8660254037844387076, 1.000000000000000000, 0.8660254037844387076, 1.000000000000000000, 0.9330127018922194093, 0.9330127018922194093 ) ) 
 REPRESENTATION_ITEM ( '' )  );
#28415 = CARTESIAN_POINT ( 'NONE',  ( 10.56230152254437726, -3.464101615137914703, -9.862500000000036238 ) ) ;
#28416 = CARTESIAN_POINT ( 'NONE',  ( 23.87821517812499650, 4.985214923628404904, -0.8531249993854739255 ) ) ;
#28417 = CARTESIAN_POINT ( 'NONE',  ( 10.31873187879410736, -3.604726614523244610, -8.709374999385509852 ) ) ;
#28418 = CARTESIAN_POINT ( 'NONE',  ( 13.50000000000001421, 198.4625000012290172, 23.38268590217984055 ) ) ;
#28419 = CARTESIAN_POINT ( 'NONE',  ( 6.932735513423970097, 119.9476862821014578, 10.69584247140445044 ) ) ;
#28420 = CARTESIAN_POINT ( 'NONE',  ( 16.56230152254411081, -7.209453229046475009, -1.828124999385505989 ) ) ;
#28421 = CARTESIAN_POINT ( 'NONE',  ( -40.10044563604517265, 203.6929966515019430, -6.137860380172892150 ) ) ;
#28422 = CARTESIAN_POINT ( 'NONE',  ( 15.24356964375000167, 244.3843750006145115, 3.323476615752272600 ) ) ;
#28423 = CARTESIAN_POINT ( 'NONE',  ( 16.56230152254411081, 6.928203230275506996, -2.699999998771041021 ) ) ;
#28424 = CARTESIAN_POINT ( 'NONE',  ( -30.99627896937850480, 205.4690446883607535, -1.090244570138286351 ) ) ;
#28425 = CARTESIAN_POINT ( 'NONE',  ( 0.1745138560725515708, 116.2101862821014606, -12.50000000000000355 ) ) ;
#28426 = CARTESIAN_POINT ( 'NONE',  ( 19.56230152254411436, -5.196152422706629359, -4.237499998771044218 ) ) ;
#28427 = EDGE_CURVE ( 'NONE', #20921, #12708, #28647, .T. ) ;
#28428 =( BOUNDED_CURVE ( )  B_SPLINE_CURVE ( 2, ( #19895, #28397, #5459, #31437, #2435, #37298, #14008 ),
 .UNSPECIFIED., .F., .F. ) 
 B_SPLINE_CURVE_WITH_KNOTS ( ( 3, 2, 2, 3 ),
 ( 0.3043478260869579288, 0.3115942028985521639, 0.3188405797101463990, 0.3260869565217406896 ),
 .UNSPECIFIED. ) 
 CURVE ( )  GEOMETRIC_REPRESENTATION_ITEM ( )  RATIONAL_B_SPLINE_CURVE ( ( 0.9999999999999743538, 0.8660254037844643538, 1.000000000000000000, 0.8660254037844387076, 1.000000000000000000, 0.8660254037844099528, 1.000000000000028644 ) ) 
 REPRESENTATION_ITEM ( '' )  );
#28429 = CARTESIAN_POINT ( 'NONE',  ( -44.26413769728823411, 213.1499508600178672, 5.686928522499718142 ) ) ;
#28430 = CARTESIAN_POINT ( 'NONE',  ( 20.99999999999999289, 240.0437500012290570, -5.999999999999997335 ) ) ;
#28431 = DIRECTION ( 'NONE',  ( -0.000000000000000000, -1.000000000000000000, -0.000000000000000000 ) ) ;
#28432 = CARTESIAN_POINT ( 'NONE',  ( 5.770363421893814682, 101.8351862821014606, 14.38691631536207183 ) ) ;
#28433 = CARTESIAN_POINT ( 'NONE',  ( 12.50000000000000355, 17.31018628210144428, 0.1745138560725507937 ) ) ;
#28434 = CARTESIAN_POINT ( 'NONE',  ( 10.56230152254410726, 0.000000000000000000, -6.300000000000055778 ) ) ;
#28435 = CARTESIAN_POINT ( 'NONE',  ( 3.796722387233379514, 125.9851862821014521, -8.710071997420127943 ) ) ;
#28436 = CARTESIAN_POINT ( 'NONE',  ( 10.31873187879410736, 3.604726614523236616, -1.978124999385525662 ) ) ;
#28437 = CARTESIAN_POINT ( 'NONE',  ( -14.50000000000000533, 252.0000000000000000, -2.500000000000000000 ) ) ;
#28439 = ORIENTED_EDGE ( 'NONE', *, *, #31868, .F. ) ;
#28438 = CIRCLE ( 'NONE', #2419, 24.80000000000000426 ) ;
#28440 = CARTESIAN_POINT ( 'NONE',  ( 25.18413345258805691, 3.604726614523236616, 169.4617919265805881 ) ) ;
#28441 = CARTESIAN_POINT ( 'NONE',  ( -3.796722387233375073, 56.98518628210145209, 8.710071997420127943 ) ) ;
#28442 = FACE_OUTER_BOUND ( 'NONE', #17428, .T. ) ;
#28443 = ADVANCED_FACE ( 'NONE', ( #27456, #13058 ), #24615, .F. ) ;
#28444 = CARTESIAN_POINT ( 'NONE',  ( -27.24356964374999990, 195.2656250006145342, -15.72908226750537786 ) ) ;
#28445 = FACE_OUTER_BOUND ( 'NONE', #12763, .T. ) ;
#28446 = CARTESIAN_POINT ( 'NONE',  ( -27.24356964375000345, 195.3593750006145342, 0.000000000000000000 ) ) ;
#28447 = FACE_OUTER_BOUND ( 'NONE', #29104, .T. ) ;
#28448 = EDGE_CURVE ( 'NONE', #2167, #2407, #36535, .T. ) ;
#28449 = CARTESIAN_POINT ( 'NONE',  ( 25.28542051998549667, 0.000000000000000000, 167.8248601567890432 ) ) ;
#28450 = CARTESIAN_POINT ( 'NONE',  ( -9.465287035748106703, 33.80231371789854222, 2.064181346179061460 ) ) ;
#28451 = CARTESIAN_POINT ( 'NONE',  ( 20.99999999999999645, 239.8187500012290059, 5.999999999999998224 ) ) ;
#28452 = VERTEX_POINT ( 'NONE', #16467 ) ;
#28453 = CARTESIAN_POINT ( 'NONE',  ( 24.00000000000000000, 242.5562500012290457, 5.196152422706629359 ) ) ;
#28454 = AXIS2_PLACEMENT_3D ( 'NONE', #30378, #13495, #22410 ) ;
#28455 = CARTESIAN_POINT ( 'NONE',  ( 10.69584247140429589, 67.15231371789855075, 6.932735513424201024 ) ) ;
#28456 = CARTESIAN_POINT ( 'NONE',  ( 19.68408634441911076, 5.407089921784862696, -8.446874999385538985 ) ) ;
#28457 = CARTESIAN_POINT ( 'NONE',  ( 15.24356964374999990, 3.323476615752268604, -7.940624999385462068 ) ) ;
#28458 = CARTESIAN_POINT ( 'NONE',  ( 4.622313124798831829, 36.96481371789854364, -11.61527771782809282 ) ) ;
#28459 = EDGE_CURVE ( 'NONE', #15329, #26034, #13394, .T. ) ;
#28460 = ORIENTED_EDGE ( 'NONE', *, *, #15354, .T. ) ;
#28461 = CARTESIAN_POINT ( 'NONE',  ( 13.44051670066911441, -5.407089921784865361, -1.021874999385524729 ) ) ;
#28462 = CARTESIAN_POINT ( 'NONE',  ( 15.00000000000000178, 246.0437500012290570, 3.464101615137757051 ) ) ;
#28463 = CARTESIAN_POINT ( 'NONE',  ( 37.52407102436108488, 7.646167579472024665E-16, 167.2340683412427040 ) ) ;
#28464 = CARTESIAN_POINT ( 'NONE',  ( -39.30877896937850124, 211.6261429550004607, -6.530955311639245586 ) ) ;
#28465 = DIRECTION ( 'NONE',  ( 0.000000000000000000, 0.000000000000000000, -1.000000000000000000 ) ) ;
#28466 =( BOUNDED_CURVE ( )  B_SPLINE_CURVE ( 2, ( #30933, #18643, #36415, #25050, #33587, #30749, #15789 ),
 .UNSPECIFIED., .F., .F. ) 
 B_SPLINE_CURVE_WITH_KNOTS ( ( 3, 2, 2, 3 ),
 ( 0.5434782608695644113, 0.5507246376811587574, 0.5579710144927531035, 0.5652173913043473386 ),
 .UNSPECIFIED. ) 
 CURVE ( )  GEOMETRIC_REPRESENTATION_ITEM ( )  RATIONAL_B_SPLINE_CURVE ( ( 1.000000000000014433, 0.8660254037844243857, 1.000000000000000000, 0.8660254037844387076, 1.000000000000000000, 0.8660254037844469233, 0.9999999999999917843 ) ) 
 REPRESENTATION_ITEM ( '' )  );
#28467 = CARTESIAN_POINT ( 'NONE',  ( 22.56230152254462240, 3.464101615137467949, -2.887500000000029932 ) ) ;
#28468 = CARTESIAN_POINT ( 'NONE',  ( -32.38913769728823411, 207.8500491399821613, -3.954877714930864485 ) ) ;
#28469 = CARTESIAN_POINT ( 'NONE',  ( -43.67038769728823411, 208.1428034533959703, 6.469044688360770401 ) ) ;
#28470 = CARTESIAN_POINT ( 'NONE',  ( 25.18740179294109183, 0.000000000000000000, 169.4991492277590339 ) ) ;
#28471 = EDGE_LOOP ( 'NONE', ( #23224, #12901 ) ) ;
#28472 = DIRECTION ( 'NONE',  ( 1.000000000000000000, 0.000000000000000000, 0.000000000000000000 ) ) ;
#28473 = CARTESIAN_POINT ( 'NONE',  ( 26.99999999999999645, 7.347880794884117764E-16, -1.518749998770940746 ) ) ;
#28474 = CARTESIAN_POINT ( 'NONE',  ( 15.50000000000000533, 20.28981371789855004, -0.1745138560722452326 ) ) ;
#28475 = CARTESIAN_POINT ( 'NONE',  ( -36.73586230271183695, 205.8500491399821613, 7.418979330068642852 ) ) ;
#28476 = CARTESIAN_POINT ( 'NONE',  ( -0.1745138560725182642, 139.2101862821014890, 9.500000000000005329 ) ) ;
#28477 = CARTESIAN_POINT ( 'NONE',  ( 0.1745138560725515708, 42.61018628210144499, -12.50000000000000355 ) ) ;
#28478 = B_SPLINE_CURVE_WITH_KNOTS ( 'NONE', 3,
 ( #31849, #19941, #28627, #2665 ),
 .UNSPECIFIED., .F., .F.,
 ( 4, 4 ),
 ( 0.000000000000000000, 1.000000000000000000 ),
 .UNSPECIFIED. ) ;
#28479 = CARTESIAN_POINT ( 'NONE',  ( 22.56230152254411792, 7.347880794884125653E-16, -5.625000000000018652 ) ) ;
#28480 = CARTESIAN_POINT ( 'NONE',  ( 20.99999999999999645, 240.6624999999999943, 5.999999999999998224 ) ) ;
#28481 = EDGE_LOOP ( 'NONE', ( #19187, #36707, #10610 ) ) ;
#28482 = CARTESIAN_POINT ( 'NONE',  ( 2.908627838312118019, 10.12268628210144428, 15.53471296425195369 ) ) ;
#28483 = CARTESIAN_POINT ( 'NONE',  ( -13.62178482187498396, 197.6843750006145228, 23.59362340125808188 ) ) ;
#28484 = CARTESIAN_POINT ( 'NONE',  ( 10.56230152254410726, 0.000000000000000000, -6.300000000000055778 ) ) ;
#28485 = CYLINDRICAL_SURFACE ( 'NONE', #35953, 27.00000000000000000 ) ;
#28486 = EDGE_CURVE ( 'NONE', #8415, #9774, #22213, .T. ) ;
#28487 = LINE ( 'NONE', #28858, #22415 ) ;
#28488 = CARTESIAN_POINT ( 'NONE',  ( 21.00000000000000000, 245.6968750006145399, -6.646953231504538984 ) ) ;
#28489 = CARTESIAN_POINT ( 'NONE',  ( -3.796722387233185003, 118.6148137178985706, -8.710071997420207879 ) ) ;
#28490 = CARTESIAN_POINT ( 'NONE',  ( 20.99999999999999645, 241.6468750006145285, -6.646953231504538984 ) ) ;
#28491 = AXIS2_PLACEMENT_3D ( 'NONE', #28980, #19924, #11555 ) ;
#28492 = ORIENTED_EDGE ( 'NONE', *, *, #21063, .T. ) ;
#28493 = CARTESIAN_POINT ( 'NONE',  ( -65.83705436395487709, 205.3262412349647263, -4.842901733360204020 ) ) ;
#28494 = CARTESIAN_POINT ( 'NONE',  ( 27.00000000000001421, 197.1500000012290172, 15.58845726811988897 ) ) ;
#28495 = CARTESIAN_POINT ( 'NONE',  ( 15.00000000000000000, 249.1187500012290741, -3.464101615137752166 ) ) ;
#28496 = CARTESIAN_POINT ( 'NONE',  ( 10.69584247140429589, 122.3523137178985678, 6.932735513424201024 ) ) ;
#28497 = CARTESIAN_POINT ( 'NONE',  ( 10.31873187879410914, 0.000000000000000000, -0.1968749993855323233 ) ) ;
#28498 = CARTESIAN_POINT ( 'NONE',  ( 37.10082094864278446, 3.604726614523238837, 162.3962978386346663 ) ) ;
#28499 = DIRECTION ( 'NONE',  ( 0.000000000000000000, 0.000000000000000000, 1.000000000000000000 ) ) ;
#28500 = CARTESIAN_POINT ( 'NONE',  ( -13.50000000000000533, 196.3249999999999886, -23.38268590217984411 ) ) ;
#28501 = ORIENTED_EDGE ( 'NONE', *, *, #19913, .F. ) ;
#28502 = ORIENTED_EDGE ( 'NONE', *, *, #18466, .T. ) ;
#28503 = ORIENTED_EDGE ( 'NONE', *, *, #13446, .F. ) ;
#28504 = CARTESIAN_POINT ( 'NONE',  ( 15.00000000000000000, 0.000000000000000000, -7.143749998770959841 ) ) ;
#28505 = CARTESIAN_POINT ( 'NONE',  ( 26.75643035624999655, 3.323476615752271268, -3.478124999385468819 ) ) ;
#28506 = CARTESIAN_POINT ( 'NONE',  ( -27.00000000000000355, 199.8312500006145171, 0.000000000000000000 ) ) ;
#28507 = CARTESIAN_POINT ( 'NONE',  ( 28.28054129496681313, -5.196152422706638241, 167.6381075309029711 ) ) ;
#28508 = CARTESIAN_POINT ( 'NONE',  ( 18.12178482187499640, 248.3218750006145115, -4.985214923628404904 ) ) ;
#28509 = CARTESIAN_POINT ( 'NONE',  ( -12.46528703574805697, 49.79768628210145209, -2.660918448318280838 ) ) ;
#28510 = CARTESIAN_POINT ( 'NONE',  ( -60.48586230271183695, 206.8500491399821328, 5.686928522499748340 ) ) ;
#28511 = CARTESIAN_POINT ( 'NONE',  ( 5.536961926789909505, 215.7986392774538729, 1.553813268097265832 ) ) ;
#28512 = CARTESIAN_POINT ( 'NONE',  ( -42.47544563604517265, 213.3788001182224718, 3.209657149897419348 ) ) ;
#28513 = CARTESIAN_POINT ( 'NONE',  ( 36.95214294612631534, -3.464101615137751278, 163.4915487413387893 ) ) ;
#28514 = CARTESIAN_POINT ( 'NONE',  ( -10.69584247140429412, 99.35231371789855359, -6.932735513424201024 ) ) ;
#28515 = CARTESIAN_POINT ( 'NONE',  ( -34.96205436395488420, 214.6737587650352168, 4.842901733360204908 ) ) ;
#28516 = CARTESIAN_POINT ( 'NONE',  ( -47.03497103062157692, 202.6965474657331185, -4.350049139982091084 ) ) ;
#28517 = CARTESIAN_POINT ( 'NONE',  ( 18.12178482187500350, -4.985214923628407568, -5.578124999385480898 ) ) ;
#28518 = VECTOR ( 'NONE', #7018, 1000.000000000000000 ) ;
#28519 = CARTESIAN_POINT ( 'NONE',  ( 20.99999999999999645, 6.928203230275506996, -0.5624999999999866773 ) ) ;
#28520 = CARTESIAN_POINT ( 'NONE',  ( 10.83675517735179206, 92.73981371789854222, -11.08355503943118769 ) ) ;
#28521 = CARTESIAN_POINT ( 'NONE',  ( -32.38169563604517265, 210.1155267958017703, 6.500000000000000888 ) ) ;
#28522 = ORIENTED_EDGE ( 'NONE', *, *, #17122, .F. ) ;
#28523 = CARTESIAN_POINT ( 'NONE',  ( 3.306546357697854128E-15, 200.0000000000000000, 27.00000000000000355 ) ) ;
#28524 = CARTESIAN_POINT ( 'NONE',  ( 11.48171059495397728, 100.6851862821014691, 4.944772684328674117 ) ) ;
#28525 = CARTESIAN_POINT ( 'NONE',  ( 14.25334919248782661, 73.08518628210143220, 6.092822981423971385 ) ) ;
#28526 = CARTESIAN_POINT ( 'NONE',  ( 10.56230152254482846, -3.464101615138174051, -0.8625000000000174749 ) ) ;
#28527 = CARTESIAN_POINT ( 'NONE',  ( 30.82381401619432637, -7.209453229046482114, 162.2867080177096852 ) ) ;
#28528 = CARTESIAN_POINT ( 'NONE',  ( -2.908627838312119351, 60.72268628210144925, -15.53471296425195369 ) ) ;
#28529 = CARTESIAN_POINT ( 'NONE',  ( 19.68408634441910721, 5.407089921784857367, -6.590624999385563676 ) ) ;
#28530 = CARTESIAN_POINT ( 'NONE',  ( -0.1745138560725182642, 19.61018628210144144, 9.500000000000005329 ) ) ;
#28531 = CARTESIAN_POINT ( 'NONE',  ( -55.52725981217218276, 242.6196170348268879, 5.000000000000000000 ) ) ;
#28532 = CARTESIAN_POINT ( 'NONE',  ( -58.11830436395490551, 209.8844732041982581, 6.500000000000000888 ) ) ;
#28533 = CARTESIAN_POINT ( 'NONE',  ( -2.311890736173176641, 51.52268628210145351, -12.53471296425194836 ) ) ;
#28534 = CARTESIAN_POINT ( 'NONE',  ( 13.49999999999999645, 197.5999999999999943, -23.38268590217984766 ) ) ;
#28535 = DIRECTION ( 'NONE',  ( -1.000000000000000000, -0.000000000000000000, -0.000000000000000000 ) ) ;
#28537 = CARTESIAN_POINT ( 'NONE',  ( 22.80587116629411426, 3.604726614523243278, -2.634374999385520777 ) ) ;
#28536 = CARTESIAN_POINT ( 'NONE',  ( -6.840914352312096547, 20.76018628210144001, 6.594114490232313663 ) ) ;
#28538 = CARTESIAN_POINT ( 'NONE',  ( 15.24356964374999990, 248.9593750006145285, 0.000000000000000000 ) ) ;
#28539 = ORIENTED_EDGE ( 'NONE', *, *, #11717, .T. ) ;
#28540 = CARTESIAN_POINT ( 'NONE',  ( 15.00000000000000178, -3.464101615137757051, -5.362499999999983835 ) ) ;
#28541 = CARTESIAN_POINT ( 'NONE',  ( -0.5000000000000047740, 244.5000000000000000, 1.000000000000000000 ) ) ;
#28542 = VECTOR ( 'NONE', #29424, 1000.000000000000114 ) ;
#28543 = CARTESIAN_POINT ( 'NONE',  ( 24.47653776615555898, 0.000000000000000000, 161.3739362214482469 ) ) ;
#28544 = CARTESIAN_POINT ( 'NONE',  ( 22.80587116629410360, -3.604726614523235284, -1.753124999385512028 ) ) ;
#28545 = CARTESIAN_POINT ( 'NONE',  ( 24.65463083184936366, 3.464101615137757051, 160.6149010293500226 ) ) ;
#28546 = CARTESIAN_POINT ( 'NONE',  ( 26.99999999999999645, 242.5374999999999943, 3.464101615137751278 ) ) ;
#28547 = CARTESIAN_POINT ( 'NONE',  ( 1.069080835302379631E-14, 199.2125000000000057, 27.00000000000000000 ) ) ;
#28548 = CARTESIAN_POINT ( 'NONE',  ( 12.50000000000000355, 63.31018628210144072, 0.1745138560725507937 ) ) ;
#28549 = ORIENTED_EDGE ( 'NONE', *, *, #23549, .T. ) ;
#28550 = ORIENTED_EDGE ( 'NONE', *, *, #1371, .F. ) ;
#28551 = AXIS2_PLACEMENT_3D ( 'NONE', #33487, #27804, #27986 ) ;
#28552 = CARTESIAN_POINT ( 'NONE',  ( -27.00000000000000355, 196.5125000012290570, 0.000000000000000000 ) ) ;
#28553 = CARTESIAN_POINT ( 'NONE',  ( -5.732297079746171420, 222.9518338469886203, -2.500000000000000000 ) ) ;
#28554 = CARTESIAN_POINT ( 'NONE',  ( -8.927990412390371944, 35.52731371789855075, -13.04141134922778988 ) ) ;
#28555 = CARTESIAN_POINT ( 'NONE',  ( 26.75643035624999655, 7.049594010296217766E-16, -9.028124999385489957 ) ) ;
#28556 = CARTESIAN_POINT ( 'NONE',  ( 21.00000000000000000, 241.6468750006145285, -6.646953231504538984 ) ) ;
#28557 = CARTESIAN_POINT ( 'NONE',  ( -47.03497103062157692, 206.1606490808709111, -2.350049139982163027 ) ) ;
#28558 = CARTESIAN_POINT ( 'NONE',  ( 24.98477879236699195, 0.000000000000000000, 49.65137702900941008 ) ) ;
#28559 = CARTESIAN_POINT ( 'NONE',  ( 24.59092967851185207, 3.604726614523240613, 162.6814417626936518 ) ) ;
#28560 = CARTESIAN_POINT ( 'NONE',  ( 8.843639120294245259, 30.06481371789855572, 3.474262827703527901 ) ) ;
#28561 = CARTESIAN_POINT ( 'NONE',  ( 13.44051670066911086, 5.407089921784856479, -9.215624999385523708 ) ) ;
#28562 = EDGE_CURVE ( 'NONE', #7301, #11787, #19728, .T. ) ;
#28563 = DIRECTION ( 'NONE',  ( 1.000000000000000000, 0.000000000000000000, 0.000000000000000000 ) ) ;
#28564 = CARTESIAN_POINT ( 'NONE',  ( 24.55568120905228113, 195.0000000000000853, 11.66401174564247789 ) ) ;
#28565 = CARTESIAN_POINT ( 'NONE',  ( -27.24356964374999990, 198.9218750006145626, -15.72908226750537786 ) ) ;
#28566 = CARTESIAN_POINT ( 'NONE',  ( 11.48171059495408208, 19.71481371789854364, -4.944772684328420986 ) ) ;
#28567 = CIRCLE ( 'NONE', #105, 7.500000000000000000 ) ;
#28568 = ORIENTED_EDGE ( 'NONE', *, *, #20383, .T. ) ;
#28569 = CARTESIAN_POINT ( 'NONE',  ( 4.944772684328679446, 70.78518628210144925, -11.48171059495397373 ) ) ;
#28570 = CARTESIAN_POINT ( 'NONE',  ( 20.99999999999999645, 248.3687500012290457, 5.999999999999998224 ) ) ;
#28571 = CARTESIAN_POINT ( 'NONE',  ( 36.82628035898769525, 3.604726614523238837, 159.2582845396456719 ) ) ;
#28572 = CARTESIAN_POINT ( 'NONE',  ( 15.00000000000000178, -3.464101615137757051, -0.8062499987709534910 ) ) ;
#28573 = CARTESIAN_POINT ( 'NONE',  ( 16.56230152254411081, -7.209453229046482114, -8.184374999385489957 ) ) ;
#28574 = CARTESIAN_POINT ( 'NONE',  ( -3.253724281355068545E-15, 197.3000000012290229, -27.00000000000000000 ) ) ;
#28575 = CARTESIAN_POINT ( 'NONE',  ( -8.843639120294326972, 85.73518628210145209, 3.474262827703335166 ) ) ;
#28576 = DIRECTION ( 'NONE',  ( 0.000000000000000000, 0.000000000000000000, 1.000000000000000000 ) ) ;
#28577 = ADVANCED_FACE ( 'NONE', ( #10392 ), #5261, .F. ) ;
#28578 = CARTESIAN_POINT ( 'NONE',  ( -8.715434833791929847, 105.8601862821014521, -8.962234695871762469 ) ) ;
#28579 = CARTESIAN_POINT ( 'NONE',  ( 20.99999999999999289, 249.8874999999999886, -5.999999999999997335 ) ) ;
#28580 = DIRECTION ( 'NONE',  ( 1.000000000000000000, 0.000000000000000000, 0.000000000000000000 ) ) ;
#28581 = VERTEX_POINT ( 'NONE', #8121 ) ;
#28582 = CARTESIAN_POINT ( 'NONE',  ( 37.02238078016990386, 3.604726614523238837, 161.4997226103520802 ) ) ;
#28583 = CARTESIAN_POINT ( 'NONE',  ( 15.24356964375000167, -3.323476615752272600, -6.853124999385484806 ) ) ;
#28584 = CARTESIAN_POINT ( 'NONE',  ( -13.62178482187498396, 196.3343750006145285, 23.59362340125808188 ) ) ;
#28585 = CARTESIAN_POINT ( 'NONE',  ( 28.14206111430700474, -5.407089921784865361, 167.4525959469342524 ) ) ;
#28586 = CARTESIAN_POINT ( 'NONE',  ( 25.16776026727616511, 0.000000000000000000, 166.4799973143651926 ) ) ;
#28587 = FACE_OUTER_BOUND ( 'NONE', #25275, .T. ) ;
#28588 = CARTESIAN_POINT ( 'NONE',  ( 15.24356964374999990, 239.9218750006145626, -3.323476615752268604 ) ) ;
#28589 = CARTESIAN_POINT ( 'NONE',  ( 27.24356964375000700, 199.0906250006145228, 15.72908226750537075 ) ) ;
#28590 = EDGE_CURVE ( 'NONE', #952, #2107, #32762, .T. ) ;
#28591 = CARTESIAN_POINT ( 'NONE',  ( -4.622313124798826500, 115.1648137178985678, 11.61527771782809637 ) ) ;
#28592 = CARTESIAN_POINT ( 'NONE',  ( -4.944772684328673229, 130.5851862821014606, 11.48171059495397728 ) ) ;
#28594 = ORIENTED_EDGE ( 'NONE', *, *, #32287, .T. ) ;
#28593 = ORIENTED_EDGE ( 'NONE', *, *, #34661, .T. ) ;
#28595 = CARTESIAN_POINT ( 'NONE',  ( 21.00000000000000000, 241.0843750006145285, -6.646953231504538984 ) ) ;
#28596 = CARTESIAN_POINT ( 'NONE',  ( 22.56230152254317645, -3.464101615138286849, -1.949999998771017262 ) ) ;
#28597 = CARTESIAN_POINT ( 'NONE',  ( 15.50000000000000533, 93.88981371789856212, -0.1745138560722452326 ) ) ;
#28598 = AXIS2_PLACEMENT_3D ( 'NONE', #27466, #4528, #21791 ) ;
#28599 = CARTESIAN_POINT ( 'NONE',  ( 8.715434833791931624, 92.06018628210145494, 8.962234695871760692 ) ) ;
#28600 = CARTESIAN_POINT ( 'NONE',  ( 26.75643035624999655, -3.323476615752267715, -2.765624999385494220 ) ) ;
#28601 = PRODUCT ( 'follower', 'follower', '', ( #32908 ) ) ;
#28602 = CARTESIAN_POINT ( 'NONE',  ( 26.99999999999999645, 197.6750000012290513, -15.58845726811990495 ) ) ;
#28603 = CARTESIAN_POINT ( 'NONE',  ( -11.48171059495397373, 114.4851862821014521, -4.944772684328680334 ) ) ;
#28604 = CARTESIAN_POINT ( 'NONE',  ( 13.44051670066911797, -5.407089921784859143, -3.665624999385552751 ) ) ;
#28605 = CARTESIAN_POINT ( 'NONE',  ( 18.12178482187499640, 244.7218750006145171, -4.985214923628404904 ) ) ;
#28606 = CARTESIAN_POINT ( 'NONE',  ( 23.99999999999999645, 246.7562500012290627, -5.196152422706631135 ) ) ;
#28607 = EDGE_CURVE ( 'NONE', #34104, #32257, #18944, .T. ) ;
#28608 = CARTESIAN_POINT ( 'NONE',  ( -54.35044563604515133, 205.1570982666397072, -4.673758765035155527 ) ) ;
#28609 = CARTESIAN_POINT ( 'NONE',  ( 8.715434833791931624, 119.6601862821014493, 8.962234695871760692 ) ) ;
#28610 = CARTESIAN_POINT ( 'NONE',  ( 10.56230152254411081, 0.000000000000000000, -3.037499998771009402 ) ) ;
#28611 = CARTESIAN_POINT ( 'NONE',  ( -40.50372103062156981, 216.5309553116391612, -1.626142955000564383 ) ) ;
#28612 = CARTESIAN_POINT ( 'NONE',  ( 16.56230152254410726, 0.000000000000000000, -10.00000000000000000 ) ) ;
#28613 = CYLINDRICAL_SURFACE ( 'NONE', #29891, 27.00000000000000000 ) ;
#28614 = CARTESIAN_POINT ( 'NONE',  ( -8.632099005475501130, 96.94768628210147199, -13.23911966647218996 ) ) ;
#28615 = CARTESIAN_POINT ( 'NONE',  ( -12.53471296425194659, 21.62268628210144072, 2.311890736173176641 ) ) ;
#28616 = FACE_OUTER_BOUND ( 'NONE', #22904, .T. ) ;
#28617 = EDGE_CURVE ( 'NONE', #26185, #34425, #6860, .T. ) ;
#28618 = CARTESIAN_POINT ( 'NONE',  ( 34.34268633269625326, -5.196152422706635576, 168.0864629050564929 ) ) ;
#28619 = CARTESIAN_POINT ( 'NONE',  ( -9.534712964251941258, 122.8226862821014294, 1.715153634034234154 ) ) ;
#28620 = CARTESIAN_POINT ( 'NONE',  ( 10.31873187879411091, 3.604726614523236616, -2.428124999385521399 ) ) ;
#28621 = CARTESIAN_POINT ( 'NONE',  ( 20.99999999999997868, 245.6687500012291139, 5.999999999999999112 ) ) ;
#28622 = VERTEX_POINT ( 'NONE', #22158 ) ;
#28623 = CARTESIAN_POINT ( 'NONE',  ( 25.19067013329413385, -3.604726614523240613, 169.5365065289374513 ) ) ;
#28624 = CARTESIAN_POINT ( 'NONE',  ( -2.064181346179269738, 65.89768628210143220, 9.465287035748067623 ) ) ;
#28625 = CARTESIAN_POINT ( 'NONE',  ( -49.64999999999999858, 244.5000000000000000, 5.000000000000000000 ) ) ;
#28626 = EDGE_CURVE ( 'NONE', #1229, #14950, #13166, .T. ) ;
#28627 = CARTESIAN_POINT ( 'NONE',  ( -20.86978560514296532, 194.8401013911397683, -17.51182845191284798 ) ) ;
#28629 = LINE ( 'NONE', #37340, #36054 ) ;
#28628 =( BOUNDED_CURVE ( )  B_SPLINE_CURVE ( 2, ( #17832, #6630, #23888, #14975, #12314, #1124, #18391, #27100, #35429 ),
 .UNSPECIFIED., .F., .F. ) 
 B_SPLINE_CURVE_WITH_KNOTS ( ( 3, 2, 2, 2, 3 ),
 ( 0.1458333333333333426, 0.1527777777777777901, 0.1666666666666666574, 0.1805555555555555525, 0.1875000000000000000 ),
 .UNSPECIFIED. ) 
 CURVE ( )  GEOMETRIC_REPRESENTATION_ITEM ( )  RATIONAL_B_SPLINE_CURVE ( ( 0.9330127018922194093, 0.9330127018922194093, 1.000000000000000000, 0.8660254037844387076, 1.000000000000000000, 0.8660254037844387076, 1.000000000000000000, 0.9330127018922194093, 0.9330127018922194093 ) ) 
 REPRESENTATION_ITEM ( '' )  );
#28630 = CARTESIAN_POINT ( 'NONE',  ( -27.24356964375000345, 196.2593750006145399, 0.000000000000000000 ) ) ;
#28631 = CARTESIAN_POINT ( 'NONE',  ( 10.56230152254410726, 0.000000000000000000, -8.887499998771003717 ) ) ;
#28632 = CARTESIAN_POINT ( 'NONE',  ( -47.00000000000000711, 244.5000000000000000, 5.000000000000000000 ) ) ;
#28633 = CARTESIAN_POINT ( 'NONE',  ( -8.152565276336593669, 44.15231371789854364, -5.233372021372610483 ) ) ;
#28634 = CARTESIAN_POINT ( 'NONE',  ( 26.99999999999999645, -3.464101615137751278, -9.262500000000022382 ) ) ;
#28635 = VERTEX_POINT ( 'NONE', #22337 ) ;
#28636 = ORIENTED_EDGE ( 'NONE', *, *, #22077, .F. ) ;
#28637 = CARTESIAN_POINT ( 'NONE',  ( 15.24356964375000167, 248.8843750006145399, 3.323476615752272600 ) ) ;
#28638 = CARTESIAN_POINT ( 'NONE',  ( 7.228626920338837358, 58.52731371789855785, 10.49813415416005036 ) ) ;
#28639 = CARTESIAN_POINT ( 'NONE',  ( 10.31873187879410736, 3.604726614523240613, -7.884374999385513227 ) ) ;
#28640 = CARTESIAN_POINT ( 'NONE',  ( 18.12178482187499640, 4.985214923628404904, -9.328124999385483562 ) ) ;
#28641 = CARTESIAN_POINT ( 'NONE',  ( -10.83675517735179028, 143.3398137178985507, 11.08355503943118947 ) ) ;
#28642 = EDGE_CURVE ( 'NONE', #16220, #20921, #18272, .T. ) ;
#28643 = EDGE_LOOP ( 'NONE', ( #12192, #30854, #12743, #20686, #4661, #31176, #2544, #9495 ) ) ;
#28644 = CARTESIAN_POINT ( 'NONE',  ( 19.68408634441911431, -5.407089921784861808, -0.9468749993855329894 ) ) ;
#28645 = CARTESIAN_POINT ( 'NONE',  ( -8.715434833791929847, 4.660186282101435928, -8.962234695871762469 ) ) ;
#28646 = CARTESIAN_POINT ( 'NONE',  ( 37.36719068741531657, 7.646167579472024665E-16, 165.4409178846775603 ) ) ;
#28647 =( BOUNDED_CURVE ( )  B_SPLINE_CURVE ( 2, ( #15145, #24431, #35981, #10017, #21598, #33147, #7191 ),
 .UNSPECIFIED., .F., .F. ) 
 B_SPLINE_CURVE_WITH_KNOTS ( ( 3, 2, 2, 3 ),
 ( 0.5869565217391301548, 0.5942028985507243899, 0.6014492753623187360, 0.6086956521739130821 ),
 .UNSPECIFIED. ) 
 CURVE ( )  GEOMETRIC_REPRESENTATION_ITEM ( )  RATIONAL_B_SPLINE_CURVE ( ( 1.000000000000006217, 0.8660254037844326014, 1.000000000000000000, 0.8660254037844387076, 1.000000000000000000, 0.8660254037844387076, 1.000000000000000000 ) ) 
 REPRESENTATION_ITEM ( '' )  );
#28648 = CIRCLE ( 'NONE', #6890, 1.500000000000001332 ) ;
#28649 = CARTESIAN_POINT ( 'NONE',  ( -38.12127896937848703, 216.5309553116391612, 1.626142955000506873 ) ) ;
#28650 = CYLINDRICAL_SURFACE ( 'NONE', #10128, 9.999999999999994671 ) ;
#28651 = EDGE_CURVE ( 'NONE', #24633, #2680, #2970, .T. ) ;
#28652 = CARTESIAN_POINT ( 'NONE',  ( -59.89211230271182274, 205.5309553116392465, 1.321298161741817356 ) ) ;
#28653 = CARTESIAN_POINT ( 'NONE',  ( -42.68080436395489841, 203.5000000000000000, -0.1155267958017335561 ) ) ;
#28654 = CARTESIAN_POINT ( 'NONE',  ( 25.37366570962461054, 0.000000000000000000, 168.8335072898312887 ) ) ;
#28655 = ORIENTED_EDGE ( 'NONE', *, *, #5296, .T. ) ;
#28656 = CARTESIAN_POINT ( 'NONE',  ( 1.120210788295102201E-13, 196.7375000000000398, -27.00000000000000711 ) ) ;
#28657 = CARTESIAN_POINT ( 'NONE',  ( 5.770363421894130873, 18.56481371789855928, -14.38691631536193860 ) ) ;
#28658 = CARTESIAN_POINT ( 'NONE',  ( -32.38169563604516554, 210.1155267958018271, 8.500000000000003553 ) ) ;
#28659 = CARTESIAN_POINT ( 'NONE',  ( -11.48171059495397373, 13.28518628210142971, -4.944772684328680334 ) ) ;
#28660 = CARTESIAN_POINT ( 'NONE',  ( -4.622313124798576922, 42.03518628210144215, -11.61527771782819762 ) ) ;
#28661 = VECTOR ( 'NONE', #24591, 1000.000000000000000 ) ;
#28662 = CARTESIAN_POINT ( 'NONE',  ( 16.56230152254411436, -6.928203230275514990, -4.387500000000030376 ) ) ;
#28663 = ORIENTED_EDGE ( 'NONE', *, *, #28157, .F. ) ;
#28664 = CARTESIAN_POINT ( 'NONE',  ( -27.00000000000000355, 198.7250000012290343, -15.58845726811989429 ) ) ;
#28665 = CARTESIAN_POINT ( 'NONE',  ( 13.62178482187499640, 196.5593750006145513, -23.59362340125807123 ) ) ;
#28666 = CARTESIAN_POINT ( 'NONE',  ( 33.88511868327108090, 5.196152422706637353, 162.8564407400748451 ) ) ;
#28667 = DIRECTION ( 'NONE',  ( 0.9961946980917462113, 0.000000000000000000, -0.08715574274765118534 ) ) ;
#28668 = DIRECTION ( 'NONE',  ( 0.000000000000000000, 0.000000000000000000, -1.000000000000000000 ) ) ;
#28669 = CARTESIAN_POINT ( 'NONE',  ( 18.00000000000000000, 240.0812500012290513, -5.196152422706630247 ) ) ;
#28670 = CARTESIAN_POINT ( 'NONE',  ( 15.24356964375000167, 245.3968750006145285, 3.323476615752272600 ) ) ;
#28671 = CARTESIAN_POINT ( 'NONE',  ( -5.529263428287297444, 99.92731371789854222, -7.954856959092311719 ) ) ;
#28672 = CARTESIAN_POINT ( 'NONE',  ( 23.87821517812500005, 241.0093750006145399, 4.985214923628404016 ) ) ;
#28673 = ORIENTED_EDGE ( 'NONE', *, *, #11736, .F. ) ;
#28674 = CARTESIAN_POINT ( 'NONE',  ( -82.45892874490161262, 210.6708926576488921, 5.000000000000000000 ) ) ;
#28675 = DIRECTION ( 'NONE',  ( -0.000000000000000000, 1.000000000000000000, -0.000000000000000000 ) ) ;
#28676 = CARTESIAN_POINT ( 'NONE',  ( 15.00000000000000000, 246.9062500012290400, 0.000000000000000000 ) ) ;
#28677 = EDGE_LOOP ( 'NONE', ( #34153, #26688 ) ) ;
#28678 = CARTESIAN_POINT ( 'NONE',  ( 2.311890736173452421, 110.2773137178985650, -12.53471296425189152 ) ) ;
#28679 = CARTESIAN_POINT ( 'NONE',  ( 19.68408634441911431, 5.407089921784862696, -0.3468749993855158031 ) ) ;
#28680 = CARTESIAN_POINT ( 'NONE',  ( 27.75476278247212747, -5.407089921784859143, 163.0257557572890335 ) ) ;
#28681 = CARTESIAN_POINT ( 'NONE',  ( 21.00000000000000000, -6.646953231504538984, -2.390624999385460470 ) ) ;
#28682 = CARTESIAN_POINT ( 'NONE',  ( -11.48171059495408208, 79.51481371789856212, 4.944772684328421875 ) ) ;
#28683 = CARTESIAN_POINT ( 'NONE',  ( -13.62178482187500528, 199.7843750006145456, -23.59362340125807123 ) ) ;
#28684 = ORIENTED_EDGE ( 'NONE', *, *, #23360, .F. ) ;
#28685 = ORIENTED_EDGE ( 'NONE', *, *, #9132, .F. ) ;
#28686 = VERTEX_POINT ( 'NONE', #2784 ) ;
#28687 = CARTESIAN_POINT ( 'NONE',  ( 21.00000000000000000, -6.928203230275506996, -6.131249998770972098 ) ) ;
#28689 = COLOUR_RGB ( '',0.8941176470588234615, 0.8941176470588234615, 0.8941176470588234615 ) ;
#28688 = CARTESIAN_POINT ( 'NONE',  ( 26.75643035624999655, 3.323476615752271268, -2.128124999385481608 ) ) ;
#28690 = CARTESIAN_POINT ( 'NONE',  ( 27.61053152270135058, 5.196152422706630247, 159.9798607905470362 ) ) ;
#28691 =( BOUNDED_CURVE ( )  B_SPLINE_CURVE ( 2, ( #30984, #1972, #31168, #8046, #10324, #36277, #27942 ),
 .UNSPECIFIED., .F., .F. ) 
 B_SPLINE_CURVE_WITH_KNOTS ( ( 3, 2, 2, 3 ),
 ( 0.6739130434782591994, 0.6811594202898535455, 0.6884057971014477806, 0.6956521739130421267 ),
 .UNSPECIFIED. ) 
 CURVE ( )  GEOMETRIC_REPRESENTATION_ITEM ( )  RATIONAL_B_SPLINE_CURVE ( ( 1.000000000000030864, 0.8660254037844079544, 1.000000000000000000, 0.8660254037844387076, 1.000000000000000000, 0.8660254037844633546, 0.9999999999999753530 ) ) 
 REPRESENTATION_ITEM ( '' )  );
#28692 = AXIS2_PLACEMENT_3D ( 'NONE', #35184, #26099, #12257 ) ;
#28693 = CARTESIAN_POINT ( 'NONE',  ( 0.000000000000000000, 210.0000000000000284, -28.99999999999999645 ) ) ;
#28694 = CARTESIAN_POINT ( 'NONE',  ( -8.962234695871760692, 57.56018628210145494, 8.715434833791933400 ) ) ;
#28695 = AXIS2_PLACEMENT_3D ( 'NONE', #16780, #22842, #29393 ) ;
#28696 = EDGE_CURVE ( 'NONE', #29694, #36021, #29304, .T. ) ;
#28697 =( GEOMETRIC_REPRESENTATION_CONTEXT ( 3 ) GLOBAL_UNCERTAINTY_ASSIGNED_CONTEXT ( ( #19218 ) ) GLOBAL_UNIT_ASSIGNED_CONTEXT ( ( #17902, #23584, #32289 ) ) REPRESENTATION_CONTEXT ( 'NONE', 'WORKASPACE' ) );
#28698 = CARTESIAN_POINT ( 'NONE',  ( -55.73586230271182984, 206.8500491399821328, 5.686928522499748340 ) ) ;
#28699 = CARTESIAN_POINT ( 'NONE',  ( 21.00000000000000355, 0.000000000000000000, 50.00000000000001421 ) ) ;
#28700 = CARTESIAN_POINT ( 'NONE',  ( -41.09002896937850124, 206.1606490808709111, 2.350049139982143931 ) ) ;
#28701 = CARTESIAN_POINT ( 'NONE',  ( 34.03873067997093216, -5.196152422706629359, 164.6122338966858933 ) ) ;
#28702 = CARTESIAN_POINT ( 'NONE',  ( 12.46528703574811558, 102.8023137178985422, -2.660918448318005503 ) ) ;
#28703 = CARTESIAN_POINT ( 'NONE',  ( -37.93080436395489841, 203.5000000000000000, -0.1155267958017335561 ) ) ;
#28705 = ADVANCED_FACE ( 'NONE', ( #32151 ), #26461, .F. ) ;
#28704 = CARTESIAN_POINT ( 'NONE',  ( -43.27455436395490551, 203.6929966515020283, 6.137860380172978303 ) ) ;
#28706 = CARTESIAN_POINT ( 'NONE',  ( 23.87821517812499650, 4.985214923628404904, -4.453124999385494220 ) ) ;
#28707 = CYLINDRICAL_SURFACE ( 'NONE', #28865, 2.499999999999997335 ) ;
#28708 = CARTESIAN_POINT ( 'NONE',  ( 8.927990412390371944, 67.72731371789853938, 13.04141134922778811 ) ) ;
#28709 = CARTESIAN_POINT ( 'NONE',  ( -35.94419563604516554, 203.5000000000000000, 0.1155267958017914542 ) ) ;
#28710 = PRODUCT_DEFINITION ( 'UNKNOWN', '', #17214, #3152 ) ;
#28711 = VERTEX_POINT ( 'NONE', #23076 ) ;
#28712 = CARTESIAN_POINT ( 'NONE',  ( 24.94551312337715032, -3.464101615137971546, 163.9397008354555965 ) ) ;
#28713 = CARTESIAN_POINT ( 'NONE',  ( 7.228626920339068285, 98.67268628210145209, -10.49813415415989581 ) ) ;
#28714 = CARTESIAN_POINT ( 'NONE',  ( -11.08355503943142573, 39.16018628210144215, 10.83675517735155402 ) ) ;
#28715 = CARTESIAN_POINT ( 'NONE',  ( 16.56230152254411081, 6.928203230275506996, -9.899999998771034981 ) ) ;
#28716 = CARTESIAN_POINT ( 'NONE',  ( 30.74537384772143866, -7.209453229046482114, 161.3901327894271276 ) ) ;
#28717 = CARTESIAN_POINT ( 'NONE',  ( -3.257655550457281723, 75.09768628210143504, 15.46528703574804986 ) ) ;
#28718 = CARTESIAN_POINT ( 'NONE',  ( 13.44051670066911264, 5.407089921784856479, -6.065624999385538452 ) ) ;
#28719 = LINE ( 'NONE', #6160, #33407 ) ;
#28720 = CARTESIAN_POINT ( 'NONE',  ( -51.58705436395488420, 205.3262412349647263, -4.842901733360204020 ) ) ;
#28721 = CARTESIAN_POINT ( 'NONE',  ( -11.61527771782819940, 30.53518628210144570, 4.622313124798574258 ) ) ;
#28722 = CARTESIAN_POINT ( 'NONE',  ( 27.00000000000001066, 198.3875000000000171, 15.58845726811988897 ) ) ;
#28723 = CARTESIAN_POINT ( 'NONE',  ( 25.09585677961620576, 3.464101615137598067, 165.6581366896638770 ) ) ;
#28724 = CARTESIAN_POINT ( 'NONE',  ( -3.474262827703337830, 14.43518628210144072, -8.843639120294326972 ) ) ;
#28725 = CARTESIAN_POINT ( 'NONE',  ( 26.75643035624999655, 248.6968750006145115, 3.323476615752267271 ) ) ;
#28726 = ORIENTED_EDGE ( 'NONE', *, *, #11552, .T. ) ;
#28727 = CARTESIAN_POINT ( 'NONE',  ( 21.00000000000000000, -6.928203230275506996, -3.487500000000006928 ) ) ;
#28728 = DIRECTION ( 'NONE',  ( -1.000000000000000000, 0.000000000000000000, 0.000000000000000000 ) ) ;
#28729 = CARTESIAN_POINT ( 'NONE',  ( 24.44058602227215360, -3.604726614523244610, 160.9630059084853997 ) ) ;
#28730 = CARTESIAN_POINT ( 'NONE',  ( 13.44051670066911264, 5.407089921784856479, -3.815624999385564209 ) ) ;
#28731 = CARTESIAN_POINT ( 'NONE',  ( 30.64487238181199302, -6.928203230275514990, 160.2413957775779068 ) ) ;
#28732 = CARTESIAN_POINT ( 'NONE',  ( 15.00000000000000178, 243.7374999999999829, 3.464101615137757051 ) ) ;
#28733 = CARTESIAN_POINT ( 'NONE',  ( 19.80074372294634344, 5.630122097104456991, -7.999999999999998224 ) ) ;
#28734 = CARTESIAN_POINT ( 'NONE',  ( 10.69584247140445221, 71.64768628210146062, -6.932735513423970097 ) ) ;
#28735 = VERTEX_POINT ( 'NONE', #20426 ) ;
#28736 = ORIENTED_EDGE ( 'NONE', *, *, #16456, .F. ) ;
#28737 = CARTESIAN_POINT ( 'NONE',  ( 15.00000000000000355, 7.347880794884112834E-16, -8.000000000000000000 ) ) ;
#28738 = CARTESIAN_POINT ( 'NONE',  ( -1.909035429704832693E-15, 195.9500000012290002, -31.17691453623979214 ) ) ;
#28739 = CARTESIAN_POINT ( 'NONE',  ( 23.99999999999999645, 5.196152422706631135, -5.043749998770941545 ) ) ;
#28740 = CARTESIAN_POINT ( 'NONE',  ( -13.04141134922778456, 33.22731371789855359, 8.927990412390377273 ) ) ;
#28741 = DIRECTION ( 'NONE',  ( 0.08715574274765150453, 0.000000000000000000, 0.9961946980917461003 ) ) ;
#28742 = CARTESIAN_POINT ( 'NONE',  ( 26.75643035624999655, 243.3718750006145228, -3.323476615752271712 ) ) ;
#28743 = CARTESIAN_POINT ( 'NONE',  ( -40.30580436395490551, 214.5000000000000284, 0.1155267958017899832 ) ) ;
#28744 = FACE_OUTER_BOUND ( 'NONE', #2218, .T. ) ;
#28745 = CARTESIAN_POINT ( 'NONE',  ( 24.59419801886489054, 0.000000000000000000, 162.7187990638720976 ) ) ;
#28746 = CARTESIAN_POINT ( 'NONE',  ( -3.474262827703527901, 13.96481371789853831, 8.843639120294245259 ) ) ;
#28747 = CARTESIAN_POINT ( 'NONE',  ( 28.11058759660888740, 5.196152422706636465, 165.6955278696240725 ) ) ;
#28748 = VECTOR ( 'NONE', #36335, 1000.000000000000000 ) ;
#28749 = AXIS2_PLACEMENT_3D ( 'NONE', #21946, #1462, #15505 ) ;
#28750 = DIRECTION ( 'NONE',  ( 0.000000000000000000, 0.000000000000000000, 1.000000000000000000 ) ) ;
#28751 = CARTESIAN_POINT ( 'NONE',  ( 21.07789340583945403, 194.9999999999999716, 17.32733911463861887 ) ) ;
#28752 = CARTESIAN_POINT ( 'NONE',  ( -27.24356964375000345, 196.7093750006145569, 0.000000000000000000 ) ) ;
#28753 = CARTESIAN_POINT ( 'NONE',  ( 10.83675517735179206, 129.5398137178985678, -11.08355503943118769 ) ) ;
#28754 = EDGE_LOOP ( 'NONE', ( #4086, #25797, #15928, #11102, #2168, #24089, #15300, #27767, #22300, #24911, #27125, #395, #13470, #792, #8772, #23299, #33822, #35634, #22413, #18784, #20505, #2856, #1900, #34093, #16776, #30995, #23253, #30325, #33871, #34536, #2522, #24363, #21120, #19497, #3616, #10200, #32380, #24882, #17520, #14578, #17854, #15233, #22709, #15447, #6743, #22209, #29042, #25873 ) ) ;
#28755 = CARTESIAN_POINT ( 'NONE',  ( 10.49813415415989581, 45.77268628210144641, 7.228626920339068285 ) ) ;
#28756 = FACE_OUTER_BOUND ( 'NONE', #8021, .T. ) ;
#28757 = ADVANCED_FACE ( 'NONE', ( #20053 ), #8482, .T. ) ;
#28758 = CARTESIAN_POINT ( 'NONE',  ( 10.56230152254410903, 0.000000000000000000, -6.187499998771023080 ) ) ;
#28759 = CARTESIAN_POINT ( 'NONE',  ( 29.49486222041940664, 6.148715791637009431, 159.5363414366720178 ) ) ;
#28760 = CARTESIAN_POINT ( 'NONE',  ( 24.00000000000000000, -5.196152422706629359, -1.593749998770960241 ) ) ;
#28761 = CARTESIAN_POINT ( 'NONE',  ( 10.31873187879410558, -3.604726614523244610, -9.159374999385507365 ) ) ;
#28762 = CARTESIAN_POINT ( 'NONE',  ( 13.50000000000001421, 197.1125000012290513, 23.38268590217984055 ) ) ;
#28763 = CARTESIAN_POINT ( 'NONE',  ( 1.715153634034233487, 74.52268628210144641, 9.534712964251941258 ) ) ;
#28764 = CARTESIAN_POINT ( 'NONE',  ( 22.56230152254244814, -3.464101615138709178, -1.049999998771002474 ) ) ;
#28765 = CARTESIAN_POINT ( 'NONE',  ( -12.46528703574805697, 95.79768628210143788, -2.660918448318280838 ) ) ;
#28766 = CARTESIAN_POINT ( 'NONE',  ( 1.120210788295102201E-13, 197.1875000000000568, -27.00000000000000711 ) ) ;
#28767 = CARTESIAN_POINT ( 'NONE',  ( 10.31873187879411091, 0.000000000000000000, -0.1406249993855246405 ) ) ;
#28768 = VERTEX_POINT ( 'NONE', #8303 ) ;
#28769 = CARTESIAN_POINT ( 'NONE',  ( 27.66324925258708589, 5.407089921784856479, 161.9797513242927209 ) ) ;
#28770 = CARTESIAN_POINT ( 'NONE',  ( 26.75643035624999655, -3.323476615752267715, -6.703124999385464911 ) ) ;
#28771 = CARTESIAN_POINT ( 'NONE',  ( 26.99999999999999645, 196.2125000000000057, -15.58845726811990495 ) ) ;
#28772 = CARTESIAN_POINT ( 'NONE',  ( 25.06483902970220967, 0.000000000000000000, 168.0982504335675287 ) ) ;
#28773 = CARTESIAN_POINT ( 'NONE',  ( 25.20371201115956694, 3.464101615137757051, 166.8909276273280682 ) ) ;
#28774 = CARTESIAN_POINT ( 'NONE',  ( 15.00000000000000000, 3.464101615137752610, -0.03749999999999697325 ) ) ;
#28775 = CARTESIAN_POINT ( 'NONE',  ( 21.00000000000000000, 241.4218750006145626, 6.646953231504538984 ) ) ;
#28776 = CARTESIAN_POINT ( 'NONE',  ( 27.24356964374999279, 198.2656250006145058, -15.72908226750539207 ) ) ;
#28777 = ADVANCED_FACE ( 'NONE', ( #6191 ), #14358, .F. ) ;
#28778 = AXIS2_PLACEMENT_3D ( 'NONE', #1695, #13083, #1509 ) ;
#28779 = CARTESIAN_POINT ( 'NONE',  ( -10.69584247140429412, 126.9523137178985621, -6.932735513424201024 ) ) ;
#28780 = CARTESIAN_POINT ( 'NONE',  ( 11.61527771782819940, 117.9351862821014549, -4.622313124798573369 ) ) ;
#28781 = ADVANCED_FACE ( 'NONE', ( #28935 ), #12061, .T. ) ;
#28783 = ORIENTED_EDGE ( 'NONE', *, *, #1506, .T. ) ;
#28782 = ORIENTED_EDGE ( 'NONE', *, *, #17481, .F. ) ;
#28784 = CARTESIAN_POINT ( 'NONE',  ( 13.62178482187501416, 197.2531250006145456, 23.59362340125806767 ) ) ;
#28785 = CARTESIAN_POINT ( 'NONE',  ( 26.75643035624999655, 242.7343750006145342, 3.323476615752267715 ) ) ;
#28786 = FACE_OUTER_BOUND ( 'NONE', #33622, .T. ) ;
#28787 = CARTESIAN_POINT ( 'NONE',  ( 11.08355503943118769, 95.03981371789855359, 10.83675517735179028 ) ) ;
#28788 = CARTESIAN_POINT ( 'NONE',  ( 21.00000000000000000, 6.646953231504538984, -1.715624999385482852 ) ) ;
#28789 = CARTESIAN_POINT ( 'NONE',  ( 13.49999999999999645, 195.9125000012290343, -23.38268590217984766 ) ) ;
#28790 = CARTESIAN_POINT ( 'NONE',  ( -3.796722387233185003, 81.81481371789855928, -8.710071997420207879 ) ) ;
#28791 = CARTESIAN_POINT ( 'NONE',  ( 16.56230152254410726, -7.209453229046475009, -3.178124999385525395 ) ) ;
#28792 = CARTESIAN_POINT ( 'NONE',  ( 15.24356964374999990, 242.5093750006145115, -3.323476615752268604 ) ) ;
#28793 = CARTESIAN_POINT ( 'NONE',  ( 11.48171059495408208, 74.91481371789855359, -4.944772684328420986 ) ) ;
#28794 = DIRECTION ( 'NONE',  ( 0.000000000000000000, 0.000000000000000000, 1.000000000000000000 ) ) ;
#28795 = CARTESIAN_POINT ( 'NONE',  ( -2.660918448318275509, 111.8976862821014606, 12.46528703574805874 ) ) ;
#28796 = CARTESIAN_POINT ( 'NONE',  ( 22.56230152254411081, -3.464101615137751278, -4.649999998770979914 ) ) ;
#28797 = ADVANCED_FACE ( 'NONE', ( #28744 ), #31417, .F. ) ;
#28798 = VECTOR ( 'NONE', #22030, 1000.000000000000000 ) ;
#28799 = CARTESIAN_POINT ( 'NONE',  ( -44.65997103062156981, 215.5714017266979852, 3.350049139982118618 ) ) ;
#28800 = CARTESIAN_POINT ( 'NONE',  ( 26.99999999999999645, 239.9312500012290457, -7.347880794884117764E-16 ) ) ;
#28801 = DIRECTION ( 'NONE',  ( 0.000000000000000000, 0.000000000000000000, -1.000000000000000000 ) ) ;
#28802 = CARTESIAN_POINT ( 'NONE',  ( -15.46528703574804986, 95.79768628210145209, -3.257655550457287497 ) ) ;
#28803 = CARTESIAN_POINT ( 'NONE',  ( -11.61527771782819940, 12.13518628210144534, 4.622313124798574258 ) ) ;
#28804 = CARTESIAN_POINT ( 'NONE',  ( 19.56230152254411792, 5.196152422706637353, -8.250000000000062172 ) ) ;
#28805 = CARTESIAN_POINT ( 'NONE',  ( 26.99999999999999645, 244.4312500012290457, -7.347880794884117764E-16 ) ) ;
#28806 = CARTESIAN_POINT ( 'NONE',  ( 9.465287035748067623, 127.9976862821014265, 2.064181346179272847 ) ) ;
#28807 = CARTESIAN_POINT ( 'NONE',  ( 26.99999999999999645, 245.7812500012290400, -7.347880794884117764E-16 ) ) ;
#28808 = VERTEX_POINT ( 'NONE', #17580 ) ;
#28809 = CARTESIAN_POINT ( 'NONE',  ( 31.35818766391586365, 7.209453229046475009, 168.3946267603846820 ) ) ;
#28810 = CARTESIAN_POINT ( 'NONE',  ( 6.594114490232313663, 55.26018628210144357, 6.840914352312096547 ) ) ;
#28811 = CARTESIAN_POINT ( 'NONE',  ( 15.24356964374999990, 0.000000000000000000, -1.040624999385481031 ) ) ;
#28812 = AXIS2_PLACEMENT_3D ( 'NONE', #35936, #32533, #9609 ) ;
#28813 = CARTESIAN_POINT ( 'NONE',  ( 24.00000000000000000, 241.1500000000000057, 5.196152422706629359 ) ) ;
#28814 = CARTESIAN_POINT ( 'NONE',  ( 19.39230484541324273, 242.4986538117967427, 5.999999999999987566 ) ) ;
#28815 = DIRECTION ( 'NONE',  ( 1.000000000000000000, 0.000000000000000000, 2.312964634635742957E-16 ) ) ;
#28816 = CARTESIAN_POINT ( 'NONE',  ( 0.000000000000000000, 195.0000000000000000, 0.000000000000000000 ) ) ;
#28817 = ADVANCED_FACE ( 'NONE', ( #9039 ), #25725, .F. ) ;
#28818 = CARTESIAN_POINT ( 'NONE',  ( 16.56230152254410726, -6.928203230275506996, -5.624999998770996434 ) ) ;
#28819 = CARTESIAN_POINT ( 'NONE',  ( 6.594114490232462877, 37.53981371789855359, -6.840914352311949109 ) ) ;
#28820 = CARTESIAN_POINT ( 'NONE',  ( -27.24356964375000345, 198.4718750006145171, -15.72908226750537786 ) ) ;
#28821 = ORIENTED_EDGE ( 'NONE', *, *, #26044, .T. ) ;
#28822 = ORIENTED_EDGE ( 'NONE', *, *, #2652, .T. ) ;
#28823 = CARTESIAN_POINT ( 'NONE',  ( 15.24356964374999990, 248.3968750006145285, 0.000000000000000000 ) ) ;
#28824 = CARTESIAN_POINT ( 'NONE',  ( 8.962234695871567070, 39.83981371789855075, 8.715434833792127023 ) ) ;
#28825 = CARTESIAN_POINT ( 'NONE',  ( 22.80587116629412492, 3.604726614523243278, -8.484374999385497773 ) ) ;
#28826 = CARTESIAN_POINT ( 'NONE',  ( 26.75643035624999655, 3.323476615752271712, -0.3281249993854667424 ) ) ;
#28827 = CARTESIAN_POINT ( 'NONE',  ( 8.962234695871567070, 12.23981371789853512, 8.715434833792127023 ) ) ;
#28828 = VECTOR ( 'NONE', #16818, 1000.000000000000000 ) ;
#28829 = EDGE_LOOP ( 'NONE', ( #31045, #26169, #9894, #25984 ) ) ;
#28830 = CARTESIAN_POINT ( 'NONE',  ( 22.80587116629411426, 7.646167579472024665E-16, -2.671874999385509319 ) ) ;
#28831 = CARTESIAN_POINT ( 'NONE',  ( 27.24356964374999635, 198.7156250006145513, -15.72908226750539029 ) ) ;
#28832 = CARTESIAN_POINT ( 'NONE',  ( 25.02235060511272735, 3.604726614523240613, 167.6126055182478183 ) ) ;
#28833 = CARTESIAN_POINT ( 'NONE',  ( -36.14211230271182984, 203.5309553116391612, 1.857196546604092280 ) ) ;
#28834 = DIRECTION ( 'NONE',  ( 0.000000000000000000, 0.000000000000000000, -1.000000000000000000 ) ) ;
#28835 = AXIS2_PLACEMENT_3D ( 'NONE', #28612, #14226, #25777 ) ;
#28836 = EDGE_CURVE ( 'NONE', #25022, #5908, #31316, .T. ) ;
#28837 = CARTESIAN_POINT ( 'NONE',  ( -26.27693753440958702, 194.9999999999998863, 6.788958541037892758 ) ) ;
#28838 = CARTESIAN_POINT ( 'NONE',  ( -60.09002896937850124, 206.1606490808709111, 2.350049139982143931 ) ) ;
#28839 = CARTESIAN_POINT ( 'NONE',  ( -40.10788769728823411, 216.4690446883607535, 1.857196546604031662 ) ) ;
#28840 = CARTESIAN_POINT ( 'NONE',  ( 37.30839204460733782, 7.347880794884117764E-16, 167.5634945697888440 ) ) ;
#28841 = VERTEX_POINT ( 'NONE', #8666 ) ;
#28842 = FACE_OUTER_BOUND ( 'NONE', #319, .T. ) ;
#28843 = CARTESIAN_POINT ( 'NONE',  ( 10.56230152254410726, 0.000000000000000000, -1.350000000000045608 ) ) ;
#28844 = CARTESIAN_POINT ( 'NONE',  ( -3.257655550456946880, 26.90231371789854364, -15.46528703574811736 ) ) ;
#28845 = CARTESIAN_POINT ( 'NONE',  ( -61.08705436395490551, 203.8621396198270475, -6.307003348497942419 ) ) ;
#28846 = CARTESIAN_POINT ( 'NONE',  ( 2.660918448318279950, 6.097686282101443922, -12.46528703574805697 ) ) ;
#28847 =( BOUNDED_CURVE ( )  B_SPLINE_CURVE ( 2, ( #35206, #1091, #35392, #18171, #21208, #9441, #9255 ),
 .UNSPECIFIED., .F., .F. ) 
 B_SPLINE_CURVE_WITH_KNOTS ( ( 3, 2, 2, 3 ),
 ( 0.04347826086956516067, 0.05072463768115926391, 0.05797101449275336715, 0.06521739130434746345 ),
 .UNSPECIFIED. ) 
 CURVE ( )  GEOMETRIC_REPRESENTATION_ITEM ( )  RATIONAL_B_SPLINE_CURVE ( ( 1.000000000000000888, 0.8660254037844375974, 1.000000000000000000, 0.8660254037844387076, 1.000000000000000000, 0.8660254037844453689, 0.9999999999999933387 ) ) 
 REPRESENTATION_ITEM ( '' )  );
#28848 = CARTESIAN_POINT ( 'NONE',  ( -2.660918448318275509, 47.49768628210144783, 12.46528703574805874 ) ) ;
#28849 = CARTESIAN_POINT ( 'NONE',  ( 10.56230152254410903, 0.000000000000000000, -4.950000000000037481 ) ) ;
#28850 = ORIENTED_EDGE ( 'NONE', *, *, #30011, .F. ) ;
#28851 = CARTESIAN_POINT ( 'NONE',  ( -38.92038769728823411, 208.1428034533959703, 6.469044688360771289 ) ) ;
#28852 = CARTESIAN_POINT ( 'NONE',  ( 7.234628195640363302, 195.3674038105676800, -26.99999999999996803 ) ) ;
#28853 = AXIS2_PLACEMENT_3D ( 'NONE', #2509, #26003, #25630 ) ;
#28854 = CARTESIAN_POINT ( 'NONE',  ( -13.62178482187498396, 196.3343750006145285, 23.59362340125808188 ) ) ;
#28855 = FACE_OUTER_BOUND ( 'NONE', #22920, .T. ) ;
#28856 = CARTESIAN_POINT ( 'NONE',  ( 5.438367727407757144E-14, 198.5374999999999943, -27.00000000000000000 ) ) ;
#28857 = CARTESIAN_POINT ( 'NONE',  ( -47.00000000000000711, 244.5000000000000000, 5.000000000000000888 ) ) ;
#28858 = CARTESIAN_POINT ( 'NONE',  ( 10.49999999999999645, 252.0000000000000000, -5.000000000000000000 ) ) ;
#28859 = CARTESIAN_POINT ( 'NONE',  ( 18.12178482187500350, 246.3343750006145285, 4.985214923628407568 ) ) ;
#28860 = CARTESIAN_POINT ( 'NONE',  ( -5.529263428287297444, 90.72731371789855359, -7.954856959092311719 ) ) ;
#28861 = CARTESIAN_POINT ( 'NONE',  ( 26.75643035624999655, 240.6718750006145910, -3.323476615752271268 ) ) ;
#28862 = ORIENTED_EDGE ( 'NONE', *, *, #4553, .F. ) ;
#28863 = CARTESIAN_POINT ( 'NONE',  ( -56.93080436395490551, 203.5000000000000000, -0.1155267958017335561 ) ) ;
#28864 = CARTESIAN_POINT ( 'NONE',  ( 20.99999999999999645, 250.0000000000000000, 0.000000000000000000 ) ) ;
#28865 = AXIS2_PLACEMENT_3D ( 'NONE', #14682, #31743, #25869 ) ;
#28866 = CARTESIAN_POINT ( 'NONE',  ( 23.99999999999999645, 246.7562500012290627, -5.196152422706631135 ) ) ;
#28867 = ORIENTED_EDGE ( 'NONE', *, *, #10856, .T. ) ;
#28868 = CARTESIAN_POINT ( 'NONE',  ( -7.228626920338836470, 99.92731371789857064, -10.49813415416005213 ) ) ;
#28869 = CARTESIAN_POINT ( 'NONE',  ( 13.44051670066911264, -5.407089921784865361, -2.371874999385514826 ) ) ;
#28870 = CARTESIAN_POINT ( 'NONE',  ( 24.40300010821222898, 0.000000000000000000, 160.5333969449332869 ) ) ;
#28871 = CARTESIAN_POINT ( 'NONE',  ( 26.75643035624999655, 3.323476615752271712, -3.140624999385464022 ) ) ;
#28872 = CARTESIAN_POINT ( 'NONE',  ( -10.69584247140429412, 62.55231371789856354, -6.932735513424201024 ) ) ;
#28873 = CARTESIAN_POINT ( 'NONE',  ( -26.99999999999998934, 195.5374999999999943, 15.58845726811991561 ) ) ;
#28874 = VERTEX_POINT ( 'NONE', #20235 ) ;
#28875 = ORIENTED_EDGE ( 'NONE', *, *, #15193, .F. ) ;
#28876 =( BOUNDED_CURVE ( )  B_SPLINE_CURVE ( 2, ( #29362, #23500, #15347, #32019, #26901, #6050, #12115 ),
 .UNSPECIFIED., .F., .F. ) 
 B_SPLINE_CURVE_WITH_KNOTS ( ( 3, 2, 2, 3 ),
 ( 0.6521739130434789367, 0.6594202898550732828, 0.6666666666666675178, 0.6739130434782618639 ),
 .UNSPECIFIED. ) 
 CURVE ( )  GEOMETRIC_REPRESENTATION_ITEM ( )  RATIONAL_B_SPLINE_CURVE ( ( 0.9999999999999876765, 0.8660254037844510311, 1.000000000000000000, 0.8660254037844387076, 1.000000000000000000, 0.8660254037844202779, 1.000000000000018430 ) ) 
 REPRESENTATION_ITEM ( '' )  );
#28877 = VERTEX_POINT ( 'NONE', #31778 ) ;
#28878 = CARTESIAN_POINT ( 'NONE',  ( 26.99999999999999645, 3.464101615137755275, -6.881249998770976539 ) ) ;
#28879 = CARTESIAN_POINT ( 'NONE',  ( 15.24356964374999990, 0.000000000000000000, -3.290624999385455496 ) ) ;
#28880 = CARTESIAN_POINT ( 'NONE',  ( 20.99999999999999289, 241.8437500012290400, -5.999999999999997335 ) ) ;
#28881 = CARTESIAN_POINT ( 'NONE',  ( 18.12178482187499640, 246.5218750006145001, -4.985214923628404904 ) ) ;
#28882 = CARTESIAN_POINT ( 'NONE',  ( 11.48171059495397728, 45.48518628210145209, 4.944772684328674117 ) ) ;
#28883 = CARTESIAN_POINT ( 'NONE',  ( -53.55877896937849414, 211.6261429550004891, -6.530955311639245586 ) ) ;
#28884 = B_SPLINE_CURVE_WITH_KNOTS ( 'NONE', 3,
 ( #11040, #34163, #16925, #23169, #5714, #14264, #17861, #219, #29, #26000, #2688, #8571, #11414, #25815, #31873, #17295, #14444, #35086, #34902, #22982, #17484, #28837, #3437, #5904, #29016, #34532, #2871, #3062, #15006, #11594, #34712, #26181, #11968, #9136, #3250, #35267, #19960, #14631, #11783, #31503, #8758, #20331 ),
 .UNSPECIFIED., .F., .F.,
 ( 4, 2, 2, 2, 2, 2, 2, 2, 2, 2, 2, 2, 2, 2, 2, 2, 2, 2, 2, 2, 4 ),
 ( 0.000000000000000000, 0.003356155942727553562, 0.006712311885455107124, 0.01006846782818265548, 0.01174654579954642966, 0.01342462377091020211, 0.01678077971363774179, 0.02013693565636528321, 0.02349309159909282116, 0.02517116957045658840, 0.02684924754182035564, 0.03020540348454789359, 0.03188348145591166777, 0.03356155942727542807, 0.03691771537000296949, 0.03859579334136674367, 0.04027387131273051091, 0.04363002725545805233, 0.04530810522682182651, 0.04698618319818559375, 0.05369849508364069046 ),
 .UNSPECIFIED. ) ;
#28885 = LINE ( 'NONE', #14865, #11150 ) ;
#28886 = CARTESIAN_POINT ( 'NONE',  ( -36.14211230271182984, 205.5309553116392465, 1.321298161741817356 ) ) ;
#28887 =( LENGTH_UNIT ( ) NAMED_UNIT ( * ) SI_UNIT ( .MILLI., .METRE. ) );
#28888 = CARTESIAN_POINT ( 'NONE',  ( 27.80663194388356629, 5.196152422706630247, 162.2212988612534730 ) ) ;
#28889 = CARTESIAN_POINT ( 'NONE',  ( -8.962234695871565293, 99.63981371789856212, -8.715434833792128799 ) ) ;
#28890 = CARTESIAN_POINT ( 'NONE',  ( -59.89955436395489841, 213.3788001182225003, -3.209657149897400252 ) ) ;
#28891 = CARTESIAN_POINT ( 'NONE',  ( -41.09747103062157692, 214.3500491399821044, -7.303452534266878793 ) ) ;
#28892 = CARTESIAN_POINT ( 'NONE',  ( 15.24356964374999990, 3.323476615752268604, -5.240624999385486760 ) ) ;
#28893 = DIRECTION ( 'NONE',  ( 0.000000000000000000, 0.000000000000000000, 1.000000000000000000 ) ) ;
#28894 = CARTESIAN_POINT ( 'NONE',  ( -2.908627838312453306, 78.07731371789854791, 15.53471296425188797 ) ) ;
#28895 = CARTESIAN_POINT ( 'NONE',  ( -62.66294563604517265, 216.1378603801729241, -6.307003348498026796 ) ) ;
#28896 = ORIENTED_EDGE ( 'NONE', *, *, #1013, .T. ) ;
#28897 = CARTESIAN_POINT ( 'NONE',  ( 14.99999999999968203, -3.464101615137573198, -6.712500000000007461 ) ) ;
#28898 = CARTESIAN_POINT ( 'NONE',  ( 0.1745138560725515708, 107.0101862821014578, -12.50000000000000355 ) ) ;
#28899 = CARTESIAN_POINT ( 'NONE',  ( -15.53471296425195369, 40.02268628210144641, 2.908627838312118019 ) ) ;
#28900 = CARTESIAN_POINT ( 'NONE',  ( 23.35209618661503583, -3.999999999999909850, 50.00000000000000000 ) ) ;
#28901 = CARTESIAN_POINT ( 'NONE',  ( 34.02850137456756130, 5.407089921784862696, 163.0979882770355971 ) ) ;
#28902 = CARTESIAN_POINT ( 'NONE',  ( 10.83675517735155225, 73.66018628210144925, 11.08355503943142573 ) ) ;
#28903 = CARTESIAN_POINT ( 'NONE',  ( 13.62178482187499640, 199.2031250006145342, -23.59362340125807123 ) ) ;
#28904 = CARTESIAN_POINT ( 'NONE',  ( 10.31873187879410914, 0.000000000000000000, -8.690624999385526905 ) ) ;
#28905 = CARTESIAN_POINT ( 'NONE',  ( 36.56321044411491528, 7.347880794884117764E-16, 159.0460299011043901 ) ) ;
#28906 = CARTESIAN_POINT ( 'NONE',  ( -50.39955436395490551, 214.8429017333601792, -4.673758765035196383 ) ) ;
#28907 = CARTESIAN_POINT ( 'NONE',  ( 15.52041717089296213, 5.908847349338256727, -9.999738233010948107 ) ) ;
#28908 = CARTESIAN_POINT ( 'NONE',  ( -8.962234695871760692, 39.16018628210144215, 8.715434833791933400 ) ) ;
#28909 = CARTESIAN_POINT ( 'NONE',  ( 27.24356964375000345, 199.6343750006145399, -3.336375036156643733E-15 ) ) ;
#28910 = CARTESIAN_POINT ( 'NONE',  ( -6.000000000000000888, -30.00000000000000000, 20.00000000000000711 ) ) ;
#28911 = CARTESIAN_POINT ( 'NONE',  ( 8.152565276336714462, 7.247686282101430066, -5.233372021372432847 ) ) ;
#28912 = CARTESIAN_POINT ( 'NONE',  ( 18.12178482187499640, 249.7843750006145456, -4.985214923628404904 ) ) ;
#28913 = ORIENTED_EDGE ( 'NONE', *, *, #37247, .T. ) ;
#28914 = CARTESIAN_POINT ( 'NONE',  ( 24.00000000000000000, -5.196152422706629359, -5.250000000000004441 ) ) ;
#28916 = CYLINDRICAL_SURFACE ( 'NONE', #20325, 6.000000000000001776 ) ;
#28915 = PRODUCT ( 'head', 'head', '', ( #13016 ) ) ;
#28917 = EDGE_CURVE ( 'NONE', #32942, #10334, #34807, .T. ) ;
#28918 = CARTESIAN_POINT ( 'NONE',  ( 24.93897644267032732, 3.464101615137538115, 163.8649862330987332 ) ) ;
#28919 = CARTESIAN_POINT ( 'NONE',  ( 22.80587116629410360, 3.604726614523238837, -4.828124999385519978 ) ) ;
#28920 = CARTESIAN_POINT ( 'NONE',  ( 30.62526233969377998, 6.928203230275514990, 160.0172519705072318 ) ) ;
#28921 = CARTESIAN_POINT ( 'NONE',  ( 18.00000000000000355, 241.0750000000000171, 5.196152422706632912 ) ) ;
#28922 = EDGE_CURVE ( 'NONE', #13615, #17372, #14727, .T. ) ;
#28923 = CARTESIAN_POINT ( 'NONE',  ( -12.46528703574805874, 58.99768628210144783, -2.660918448318280838 ) ) ;
#28924 = EDGE_LOOP ( 'NONE', ( #3165, #1181, #30336, #30179 ) ) ;
#28925 = ORIENTED_EDGE ( 'NONE', *, *, #33554, .T. ) ;
#28926 = FACE_OUTER_BOUND ( 'NONE', #19819, .T. ) ;
#28927 = CARTESIAN_POINT ( 'NONE',  ( -13.49999999999998401, 195.2375000012290229, 23.38268590217985476 ) ) ;
#28928 = CARTESIAN_POINT ( 'NONE',  ( 15.24356964375000167, -3.323476615752272600, -5.503124999385465621 ) ) ;
#28929 = AXIS2_PLACEMENT_3D ( 'NONE', #29076, #26235, #9001 ) ;
#28930 = CARTESIAN_POINT ( 'NONE',  ( -11.08355503943118592, 35.23981371789855643, -10.83675517735179383 ) ) ;
#28931 = PLANE ( 'NONE',  #27869 ) ;
#28932 = ADVANCED_FACE ( 'NONE', ( #11874 ), #20798, .T. ) ;
#28933 = CARTESIAN_POINT ( 'NONE',  ( 23.87821517812499650, 240.7093750006145285, -4.985214923628404904 ) ) ;
#28934 = CARTESIAN_POINT ( 'NONE',  ( -39.71205436395491262, 213.2096571498974242, 3.378800118222489601 ) ) ;
#28935 = FACE_OUTER_BOUND ( 'NONE', #7777, .T. ) ;
#28936 = CARTESIAN_POINT ( 'NONE',  ( 31.39985900347063819, -6.928203230275506996, 168.8709323510220202 ) ) ;
#28937 = CARTESIAN_POINT ( 'NONE',  ( 5.529263428287300108, 21.72731371789853938, 7.954856959092309943 ) ) ;
#28938 = CARTESIAN_POINT ( 'NONE',  ( -58.71205436395488420, 214.6737587650352168, 4.842901733360204908 ) ) ;
#28939 = DIRECTION ( 'NONE',  ( 1.000000000000000000, 0.000000000000000000, 0.000000000000000000 ) ) ;
#28940 = LINE ( 'NONE', #11695, #17338 ) ;
#28941 = CARTESIAN_POINT ( 'NONE',  ( -13.62178482187500528, 195.7343750006145626, -23.59362340125807123 ) ) ;
#28942 = CARTESIAN_POINT ( 'NONE',  ( 14.25334919248795451, 139.3148137178985451, -6.092822981423661410 ) ) ;
#28943 = ORIENTED_EDGE ( 'NONE', *, *, #37043, .T. ) ;
#28944 = CARTESIAN_POINT ( 'NONE',  ( 12.53471296425194836, 53.82268628210144357, -2.311890736173178418 ) ) ;
#28945 = CARTESIAN_POINT ( 'NONE',  ( 10.56230152254411259, 3.464101615137752166, -9.824999998771010823 ) ) ;
#28946 = DIRECTION ( 'NONE',  ( 0.000000000000000000, 1.000000000000000000, 0.000000000000000000 ) ) ;
#28947 = AXIS2_PLACEMENT_3D ( 'NONE', #21696, #20956, #21516 ) ;
#28948 = CARTESIAN_POINT ( 'NONE',  ( 33.70656984979341786, -5.407089921784855591, 159.4182941109592093 ) ) ;
#28949 = CARTESIAN_POINT ( 'NONE',  ( 15.00000000000000000, 3.464101615137752166, -1.331249998770975163 ) ) ;
#28950 = CARTESIAN_POINT ( 'NONE',  ( 19.68408634441910721, 5.407089921784862696, -9.346874999385523353 ) ) ;
#28951 = CARTESIAN_POINT ( 'NONE',  ( -4.694659320240884604E-14, 197.0750000012290570, 27.00000000000000000 ) ) ;
#28952 = CARTESIAN_POINT ( 'NONE',  ( 0.1745138560725194299, 70.21018628210144641, -9.500000000000005329 ) ) ;
#28953 = CARTESIAN_POINT ( 'NONE',  ( 2.999999999999997335, 244.5000000000000000, 2.500000000000000000 ) ) ;
#28954 = CARTESIAN_POINT ( 'NONE',  ( -11.48171059495397373, 86.88518628210145778, -4.944772684328680334 ) ) ;
#28955 = CARTESIAN_POINT ( 'NONE',  ( 18.06230152254410726, 1.836970198721029441E-16, 10.00000000000000000 ) ) ;
#28956 = DIRECTION ( 'NONE',  ( 0.000000000000000000, 0.000000000000000000, 1.000000000000000000 ) ) ;
#28957 = EDGE_LOOP ( 'NONE', ( #4510, #3285, #35914 ) ) ;
#28958 = CARTESIAN_POINT ( 'NONE',  ( 24.52392870127459901, -3.604726614523240613, 161.9156170885355834 ) ) ;
#28959 = CARTESIAN_POINT ( 'NONE',  ( 15.24356964375000167, -3.323476615752272600, -8.203124999385472904 ) ) ;
#28960 = CARTESIAN_POINT ( 'NONE',  ( 13.62178482187501416, 195.5093750006145399, 23.59362340125806767 ) ) ;
#28961 = CARTESIAN_POINT ( 'NONE',  ( 37.60251119283397259, 7.646167579472024665E-16, 168.1306435695252901 ) ) ;
#28962 = CARTESIAN_POINT ( 'NONE',  ( 37.14170668649535401, 7.347880794884125653E-16, 165.6582722084640125 ) ) ;
#28963 = CARTESIAN_POINT ( 'NONE',  ( 26.99999999999999645, 248.8374999999999773, 3.464101615137751278 ) ) ;
#28964 = CARTESIAN_POINT ( 'NONE',  ( -1.926257025242585782E-15, 198.3406250006145228, -31.45816453501076637 ) ) ;
#28965 = CARTESIAN_POINT ( 'NONE',  ( 4.944772684328420986, 123.2148137178985650, 11.48171059495408208 ) ) ;
#28966 = CARTESIAN_POINT ( 'NONE',  ( -0.1745138560725500443, 130.0101862821014436, 12.50000000000000355 ) ) ;
#28968 = VERTEX_POINT ( 'NONE', #24384 ) ;
#28967 = ORIENTED_EDGE ( 'NONE', *, *, #30342, .F. ) ;
#28969 = CARTESIAN_POINT ( 'NONE',  ( -27.24356964374999990, 197.0656250006145171, -15.72908226750537786 ) ) ;
#28970 = CARTESIAN_POINT ( 'NONE',  ( 15.24356964375000167, 242.1343750006145399, 3.323476615752272600 ) ) ;
#28971 = CARTESIAN_POINT ( 'NONE',  ( -15.53471296425188442, 89.57731371789856212, -2.908627838312459080 ) ) ;
#28972 = CARTESIAN_POINT ( 'NONE',  ( 18.12178482187500350, -4.985214923628407568, -4.228124999385491023 ) ) ;
#28973 = CARTESIAN_POINT ( 'NONE',  ( 18.12178482187500350, 248.5843750006145285, 4.985214923628407568 ) ) ;
#28974 = CARTESIAN_POINT ( 'NONE',  ( -27.00000000000000355, 195.5750000012290286, -15.58845726811989429 ) ) ;
#28975 = CARTESIAN_POINT ( 'NONE',  ( 3.796722387233182339, 68.01481371789854791, 8.710071997420207879 ) ) ;
#28976 = CARTESIAN_POINT ( 'NONE',  ( 13.44051670066911264, -5.407089921784859143, -3.215624999385519267 ) ) ;
#28977 =( BOUNDED_SURFACE ( )  B_SPLINE_SURFACE ( 1, 2, ( 
 ( #13923, #25473, #19255, #31530, #19812, #13358, #7675, #22086, #36840, #16952, #2538, #33636, #17140, #28495, #10695, #30794, #8417, #5373, #37024, #5555, #11256, #5003, #1974, #16585, #1790, #11070, #7862, #31170, #4817, #19986, #16397, #19436, #27943, #8237, #22644, #14104, #30985, #13546, #34190, #25099, #28130, #25656, #22272, #33825, #2159, #16767, #31346, #13742, #34003, #25288, #37209, #22828, #34376, #10883, #22456, #26209, #23008, #17510, #9161, #31716, #17697, #14850, #35113, #432, #17887, #34744, #6504, #26399, #17323, #5931, #29432, #2900, #28676, #11621, #32087, #6119, #28866, #23379, #14473, #3468, #20729, #32272, #6315, #11997, #245, #34558, #29046, #15037, #5743, #29237, #23568, #32461, #26026, #23756, #34928, #20544, #26585, #23196, #8787, #8973, #54, #20359, #31902, #14658, #3090, #2714, #11809, #14290, #614, #3277, #12183, #35295, #9351, #25842, #20922, #37391, #11441, #8597, #20168, #36239, #6693, #21668, #15419, #15603, #35679, #10281, #15795, #35489, #4217, #36055, #21492, #21855, #27534, #10098, #18264, #4031, #26965, #33222, #27159, #806, #7261, #18836, #12946, #30382, #27345, #18650, #3841, #21303, #1182, #30002, #12756, #1376, #994, #24324, #7082, #24507, #33408, #35866, #4403, #23947, #9539, #15226, #9908, #1559, #15986, #12570, #24137, #30191, #13131, #21113, #24685, #18079, #9731, #12377, #29620, #29808, #32652, #32839, #6884, #3655, #18459, #33032, #26775, #13883, #5146, #34147, #27901, #33782, #28453, #22602, #1932, #7820, #2490, #8194, #36984, #22414, #5335, #2119, #19397, #19211, #19577, #28087, #13500, #7446, #14065, #16727, #30940, #30756, #4779, #25058, #19770, #7634, #16170, #36797, #22231, #27719, #13696, #10841, #4959, #36423, #1749, #28273, #16352, #33595, #16541, #31307, #16913, #11027, #25614, #36611, #8004, #10466, #2309, #25247, #22784, #37171, #33962, #31129, #30577, #25431, #11212, #13316, #10652, #19020, #22044, #4593, #24874, #25986, #11956, #9121, #3424, #8559, #23526, #11772, #6272, #34333, #17659, #26170, #8746, #32043, #20317, #14992, #29194, #17849, #29005, #37348, #16, #3236, #35072 ),
 ( #29387, #34889, #8929, #572, #20687, #32233, #26543, #206, #23157, #11582, #17098, #34699, #23338, #20506, #14250, #12139, #14809, #8378, #2675, #31489, #31858, #19949, #5513, #28637, #25799, #11400, #5702, #22971, #34518, #390, #6073, #20126, #31673, #5892, #17282, #17470, #28823, #26354, #2858, #14618, #14432, #3048, #21260, #9683, #3617, #33180, #24281, #35825, #27493, #36014, #12902, #1333, #15561, #12528, #953, #6464, #24091, #12710, #9866, #15183, #15942, #4179, #35255, #29579, #20881, #32799, #24467, #10053, #32420, #1516, #21629, #32611, #26730, #30338, #27301, #21447, #23714, #7224, #26923, #23906, #35636, #9310, #32987, #29765, #3987, #18035, #4362, #764, #3796, #12332, #30151, #7040, #18797, #15374, #35448, #18607, #9496, #6835, #21072, #6649, #18225, #18413, #27118, #1141, #29959, #15751, #36382, #25390, #31086, #5110, #16689, #36760, #10612, #7404, #1892, #28235, #16127, #2082, #10801, #16875, #10429, #8157, #19357, #4919, #22375, #7593, #33552, #7779, #24830, #19167, #30717, #36570, #4737, #28411, #22191, #24645, #19539, #30898, #13655, #16500, #28048, #10239, #31268, #13463, #2264, #13843, #33738, #5294, #1704, #36941, #22002, #25207, #16313, #13090, #33923, #30532, #7965, #10986, #22558, #36195, #34105, #19731, #13276, #21815, #27860, #33367, #18975, #4552, #27678, #25015, #17431, #11916, #2451, #23302, #31817, #14393, #164, #25950, #20650, #34849, #23483, #34659, #5475, #5663, #8887, #29152, #35035, #28785, #11363, #32196, #32006, #20466, #14769, #11730, #3010, #25760, #17243, #37493, #11544, #23116, #6036, #37312, #8704, #28970, #17623, #6230, #20278, #3193, #8340, #19910, #37128, #5853, #9080, #26132, #22934, #8522, #14580, #26314, #31451, #351, #17804, #20089, #34297, #14025, #2632, #17057, #22748, #34479, #25574, #31633, #2822, #28595, #11174, #14211, #18568, #12292, #18182, #12858, #6998, #21404, #6794, #27263, #24051, #29723, #3577, #3947, #12483, #23864, #29346, #24426, #27077, #3757, #15137, #26690, #35403, #4140, #29537, #532, #21218, #6607, #12099, #35597, #32758, #15331, #20839, #23673, #1103, #719, #17993 ) ),
 .UNSPECIFIED., .F., .F., .T. ) 
 B_SPLINE_SURFACE_WITH_KNOTS ( ( 2, 2 ),
 ( 3, 2, 2, 2, 2, 2, 2, 2, 2, 2, 2, 2, 2, 2, 2, 2, 2, 2, 2, 2, 2, 2, 2, 2, 2, 2, 2, 2, 2, 2, 2, 2, 2, 2, 2, 2, 2, 2, 2, 2, 2, 2, 2, 2, 2, 2, 2, 2, 2, 2, 2, 2, 2, 2, 2, 2, 2, 2, 2, 2, 2, 2, 2, 2, 2, 2, 2, 2, 2, 2, 2, 2, 2, 2, 2, 2, 2, 2, 2, 2, 2, 2, 2, 2, 2, 2, 2, 2, 2, 2, 2, 2, 2, 2, 2, 2, 2, 2, 2, 2, 2, 2, 2, 2, 2, 2, 2, 2, 2, 2, 2, 2, 2, 2, 2, 2, 2, 2, 2, 2, 2, 2, 2, 2, 2, 2, 2, 2, 2, 2, 2, 2, 2, 2, 3 ),
 ( 0.000000000000000000, 1.000000000000000000 ),
 ( 0.000000000000000000, 0.007246376811594202987, 0.01449275362318840597, 0.02173913043478260809, 0.02898550724637681195, 0.03623188405797101580, 0.04347826086956521618, 0.05072463768115942351, 0.05797101449275362389, 0.06521739130434782428, 0.07246376811594203160, 0.07971014492753622505, 0.08695652173913043237, 0.09420289855072463969, 0.1014492753623188470, 0.1086956521739130405, 0.1159420289855072478, 0.1231884057971014551, 0.1304347826086956486, 0.1376811594202898559, 0.1449275362318840632, 0.1521739130434782705, 0.1594202898550724501, 0.1666666666666666574, 0.1739130434782608647, 0.1811594202898550721, 0.1884057971014492794, 0.1956521739130434867, 0.2028985507246376940, 0.2101449275362318736, 0.2173913043478260809, 0.2246376811594202882, 0.2318840579710144956, 0.2391304347826087029, 0.2463768115942029102, 0.2536231884057971175, 0.2608695652173912971, 0.2681159420289855322, 0.2753623188405797118, 0.2826086956521738913, 0.2898550724637681264, 0.2971014492753623060, 0.3043478260869565410, 0.3115942028985507206, 0.3188405797101449002, 0.3260869565217391353, 0.3333333333333333148, 0.3405797101449275499, 0.3478260869565217295, 0.3550724637681159646, 0.3623188405797101441, 0.3695652173913043237, 0.3768115942028985588, 0.3840579710144927383, 0.3913043478260869734, 0.3985507246376811530, 0.4057971014492753881, 0.4130434782608695676, 0.4202898550724637472, 0.4275362318840579823, 0.4347826086956521618, 0.4420289855072463969, 0.4492753623188405765, 0.4565217391304347561, 0.4637681159420289911, 0.4710144927536231707, 0.4782608695652174058, 0.4855072463768115854, 0.4927536231884058204, 0.5000000000000000000, 0.5072463768115942351, 0.5144927536231883591, 0.5217391304347825942, 0.5289855072463768293, 0.5362318840579710644, 0.5434782608695651884, 0.5507246376811594235, 0.5579710144927536586, 0.5652173913043477826, 0.5724637681159420177, 0.5797101449275362528, 0.5869565217391304879, 0.5942028985507246119, 0.6014492753623188470, 0.6086956521739130821, 0.6159420289855072062, 0.6231884057971014412, 0.6304347826086956763, 0.6376811594202898004, 0.6449275362318840354, 0.6521739130434782705, 0.6594202898550725056, 0.6666666666666666297, 0.6739130434782608647, 0.6811594202898550998, 0.6884057971014492239, 0.6956521739130434590, 0.7028985507246376940, 0.7101449275362319291, 0.7173913043478260532, 0.7246376811594202882, 0.7318840579710145233, 0.7391304347826086474, 0.7463768115942028825, 0.7536231884057971175, 0.7608695652173913526, 0.7681159420289854767, 0.7753623188405797118, 0.7826086956521739468, 0.7898550724637680709, 0.7971014492753623060, 0.8043478260869565410, 0.8115942028985507761, 0.8188405797101449002, 0.8260869565217391353, 0.8333333333333333703, 0.8405797101449274944, 0.8478260869565217295, 0.8550724637681159646, 0.8623188405797101996, 0.8695652173913043237, 0.8768115942028985588, 0.8840579710144927938, 0.8913043478260869179, 0.8985507246376811530, 0.9057971014492753881, 0.9130434782608695121, 0.9202898550724637472, 0.9275362318840579823, 0.9347826086956522174, 0.9420289855072463414, 0.9492753623188405765, 0.9565217391304348116, 0.9637681159420289356, 0.9662082966761270653 ),
 .UNSPECIFIED. ) 
 GEOMETRIC_REPRESENTATION_ITEM ( )  RATIONAL_B_SPLINE_SURFACE ( (
 ( 1.000000000000000000, 0.8660254037844387076, 1.000000000000000000, 0.8660254037844387076, 1.000000000000000000, 0.8660254037844387076, 1.000000000000000000, 0.8660254037844387076, 1.000000000000000000, 0.8660254037844387076, 1.000000000000000000, 0.8660254037844387076, 1.000000000000000000, 0.8660254037844387076, 1.000000000000000000, 0.8660254037844387076, 1.000000000000000000, 0.8660254037844387076, 1.000000000000000000, 0.8660254037844387076, 1.000000000000000000, 0.8660254037844387076, 1.000000000000000000, 0.8660254037844387076, 1.000000000000000000, 0.8660254037844387076, 1.000000000000000000, 0.8660254037844387076, 1.000000000000000000, 0.8660254037844387076, 1.000000000000000000, 0.8660254037844387076, 1.000000000000000000, 0.8660254037844387076, 1.000000000000000000, 0.8660254037844387076, 1.000000000000000000, 0.8660254037844387076, 1.000000000000000000, 0.8660254037844387076, 1.000000000000000000, 0.8660254037844387076, 1.000000000000000000, 0.8660254037844387076, 1.000000000000000000, 0.8660254037844387076, 1.000000000000000000, 0.8660254037844387076, 1.000000000000000000, 0.8660254037844387076, 1.000000000000000000, 0.8660254037844387076, 1.000000000000000000, 0.8660254037844387076, 1.000000000000000000, 0.8660254037844387076, 1.000000000000000000, 0.8660254037844387076, 1.000000000000000000, 0.8660254037844387076, 1.000000000000000000, 0.8660254037844387076, 1.000000000000000000, 0.8660254037844387076, 1.000000000000000000, 0.8660254037844387076, 1.000000000000000000, 0.8660254037844387076, 1.000000000000000000, 0.8660254037844387076, 1.000000000000000000, 0.8660254037844387076, 1.000000000000000000, 0.8660254037844387076, 1.000000000000000000, 0.8660254037844387076, 1.000000000000000000, 0.8660254037844387076, 1.000000000000000000, 0.8660254037844387076, 1.000000000000000000, 0.8660254037844387076, 1.000000000000000000, 0.8660254037844387076, 1.000000000000000000, 0.8660254037844387076, 1.000000000000000000, 0.8660254037844387076, 1.000000000000000000, 0.8660254037844387076, 1.000000000000000000, 0.8660254037844387076, 1.000000000000000000, 0.8660254037844387076, 1.000000000000000000, 0.8660254037844387076, 1.000000000000000000, 0.8660254037844387076, 1.000000000000000000, 0.8660254037844387076, 1.000000000000000000, 0.8660254037844387076, 1.000000000000000000, 0.8660254037844387076, 1.000000000000000000, 0.8660254037844387076, 1.000000000000000000, 0.8660254037844387076, 1.000000000000000000, 0.8660254037844387076, 1.000000000000000000, 0.8660254037844387076, 1.000000000000000000, 0.8660254037844387076, 1.000000000000000000, 0.8660254037844387076, 1.000000000000000000, 0.8660254037844387076, 1.000000000000000000, 0.8660254037844387076, 1.000000000000000000, 0.8660254037844387076, 1.000000000000000000, 0.8660254037844387076, 1.000000000000000000, 0.8660254037844387076, 1.000000000000000000, 0.8660254037844387076, 1.000000000000000000, 0.8660254037844387076, 1.000000000000000000, 0.8660254037844387076, 1.000000000000000000, 0.8660254037844387076, 1.000000000000000000, 0.8660254037844387076, 1.000000000000000000, 0.8660254037844387076, 1.000000000000000000, 0.8660254037844387076, 1.000000000000000000, 0.8660254037844387076, 1.000000000000000000, 0.8660254037844387076, 1.000000000000000000, 0.8660254037844387076, 1.000000000000000000, 0.8660254037844387076, 1.000000000000000000, 0.8660254037844387076, 1.000000000000000000, 0.8660254037844387076, 1.000000000000000000, 0.8660254037844387076, 1.000000000000000000, 0.8660254037844387076, 1.000000000000000000, 0.8660254037844387076, 1.000000000000000000, 0.8660254037844387076, 1.000000000000000000, 0.8660254037844387076, 1.000000000000000000, 0.8660254037844387076, 1.000000000000000000, 0.8660254037844387076, 1.000000000000000000, 0.8660254037844387076, 1.000000000000000000, 0.8660254037844387076, 1.000000000000000000, 0.8660254037844387076, 1.000000000000000000, 0.8660254037844387076, 1.000000000000000000, 0.8660254037844387076, 1.000000000000000000, 0.8660254037844387076, 1.000000000000000000, 0.8660254037844387076, 1.000000000000000000, 0.8660254037844387076, 1.000000000000000000, 0.8660254037844387076, 1.000000000000000000, 0.8660254037844387076, 1.000000000000000000, 0.8660254037844387076, 1.000000000000000000, 0.8660254037844387076, 1.000000000000000000, 0.8660254037844387076, 1.000000000000000000, 0.8660254037844387076, 1.000000000000000000, 0.8660254037844387076, 1.000000000000000000, 0.8660254037844387076, 1.000000000000000000, 0.8660254037844387076, 1.000000000000000000, 0.8660254037844387076, 1.000000000000000000, 0.8660254037844387076, 1.000000000000000000, 0.8660254037844387076, 1.000000000000000000, 0.8660254037844387076, 1.000000000000000000, 0.8660254037844387076, 1.000000000000000000, 0.8660254037844387076, 1.000000000000000000, 0.8660254037844387076, 1.000000000000000000, 0.8660254037844387076, 1.000000000000000000, 0.8660254037844387076, 1.000000000000000000, 0.8660254037844387076, 1.000000000000000000, 0.8660254037844387076, 1.000000000000000000, 0.8660254037844387076, 1.000000000000000000, 0.8660254037844387076, 1.000000000000000000, 0.8660254037844387076, 1.000000000000000000, 0.8660254037844387076, 1.000000000000000000, 0.8660254037844387076, 1.000000000000000000, 0.8660254037844387076, 1.000000000000000000, 0.8660254037844387076, 1.000000000000000000, 0.8660254037844387076, 1.000000000000000000, 0.8660254037844387076, 1.000000000000000000, 0.8660254037844387076, 1.000000000000000000, 0.8660254037844387076, 1.000000000000000000, 0.8660254037844387076, 1.000000000000000000, 0.8660254037844387076, 1.000000000000000000, 0.8660254037844387076, 1.000000000000000000, 0.8660254037844387076, 1.000000000000000000, 0.8660254037844387076, 1.000000000000000000, 0.8660254037844387076, 1.000000000000000000, 0.8660254037844387076, 1.000000000000000000, 0.8660254037844387076, 1.000000000000000000, 0.8660254037844387076, 1.000000000000000000, 0.8660254037844387076, 1.000000000000000000, 0.8660254037844387076, 1.000000000000000000, 0.9548847324609573972, 0.9401541411607521326),
 ( 1.000000000000000000, 0.8660254037844387076, 1.000000000000000000, 0.8660254037844387076, 1.000000000000000000, 0.8660254037844387076, 1.000000000000000000, 0.8660254037844387076, 1.000000000000000000, 0.8660254037844387076, 1.000000000000000000, 0.8660254037844387076, 1.000000000000000000, 0.8660254037844387076, 1.000000000000000000, 0.8660254037844387076, 1.000000000000000000, 0.8660254037844387076, 1.000000000000000000, 0.8660254037844387076, 1.000000000000000000, 0.8660254037844387076, 1.000000000000000000, 0.8660254037844387076, 1.000000000000000000, 0.8660254037844387076, 1.000000000000000000, 0.8660254037844387076, 1.000000000000000000, 0.8660254037844387076, 1.000000000000000000, 0.8660254037844387076, 1.000000000000000000, 0.8660254037844387076, 1.000000000000000000, 0.8660254037844387076, 1.000000000000000000, 0.8660254037844387076, 1.000000000000000000, 0.8660254037844387076, 1.000000000000000000, 0.8660254037844387076, 1.000000000000000000, 0.8660254037844387076, 1.000000000000000000, 0.8660254037844387076, 1.000000000000000000, 0.8660254037844387076, 1.000000000000000000, 0.8660254037844387076, 1.000000000000000000, 0.8660254037844387076, 1.000000000000000000, 0.8660254037844387076, 1.000000000000000000, 0.8660254037844387076, 1.000000000000000000, 0.8660254037844387076, 1.000000000000000000, 0.8660254037844387076, 1.000000000000000000, 0.8660254037844387076, 1.000000000000000000, 0.8660254037844387076, 1.000000000000000000, 0.8660254037844387076, 1.000000000000000000, 0.8660254037844387076, 1.000000000000000000, 0.8660254037844387076, 1.000000000000000000, 0.8660254037844387076, 1.000000000000000000, 0.8660254037844387076, 1.000000000000000000, 0.8660254037844387076, 1.000000000000000000, 0.8660254037844387076, 1.000000000000000000, 0.8660254037844387076, 1.000000000000000000, 0.8660254037844387076, 1.000000000000000000, 0.8660254037844387076, 1.000000000000000000, 0.8660254037844387076, 1.000000000000000000, 0.8660254037844387076, 1.000000000000000000, 0.8660254037844387076, 1.000000000000000000, 0.8660254037844387076, 1.000000000000000000, 0.8660254037844387076, 1.000000000000000000, 0.8660254037844387076, 1.000000000000000000, 0.8660254037844387076, 1.000000000000000000, 0.8660254037844387076, 1.000000000000000000, 0.8660254037844387076, 1.000000000000000000, 0.8660254037844387076, 1.000000000000000000, 0.8660254037844387076, 1.000000000000000000, 0.8660254037844387076, 1.000000000000000000, 0.8660254037844387076, 1.000000000000000000, 0.8660254037844387076, 1.000000000000000000, 0.8660254037844387076, 1.000000000000000000, 0.8660254037844387076, 1.000000000000000000, 0.8660254037844387076, 1.000000000000000000, 0.8660254037844387076, 1.000000000000000000, 0.8660254037844387076, 1.000000000000000000, 0.8660254037844387076, 1.000000000000000000, 0.8660254037844387076, 1.000000000000000000, 0.8660254037844387076, 1.000000000000000000, 0.8660254037844387076, 1.000000000000000000, 0.8660254037844387076, 1.000000000000000000, 0.8660254037844387076, 1.000000000000000000, 0.8660254037844387076, 1.000000000000000000, 0.8660254037844387076, 1.000000000000000000, 0.8660254037844387076, 1.000000000000000000, 0.8660254037844387076, 1.000000000000000000, 0.8660254037844387076, 1.000000000000000000, 0.8660254037844387076, 1.000000000000000000, 0.8660254037844387076, 1.000000000000000000, 0.8660254037844387076, 1.000000000000000000, 0.8660254037844387076, 1.000000000000000000, 0.8660254037844387076, 1.000000000000000000, 0.8660254037844387076, 1.000000000000000000, 0.8660254037844387076, 1.000000000000000000, 0.8660254037844387076, 1.000000000000000000, 0.8660254037844387076, 1.000000000000000000, 0.8660254037844387076, 1.000000000000000000, 0.8660254037844387076, 1.000000000000000000, 0.8660254037844387076, 1.000000000000000000, 0.8660254037844387076, 1.000000000000000000, 0.8660254037844387076, 1.000000000000000000, 0.8660254037844387076, 1.000000000000000000, 0.8660254037844387076, 1.000000000000000000, 0.8660254037844387076, 1.000000000000000000, 0.8660254037844387076, 1.000000000000000000, 0.8660254037844387076, 1.000000000000000000, 0.8660254037844387076, 1.000000000000000000, 0.8660254037844387076, 1.000000000000000000, 0.8660254037844387076, 1.000000000000000000, 0.8660254037844387076, 1.000000000000000000, 0.8660254037844387076, 1.000000000000000000, 0.8660254037844387076, 1.000000000000000000, 0.8660254037844387076, 1.000000000000000000, 0.8660254037844387076, 1.000000000000000000, 0.8660254037844387076, 1.000000000000000000, 0.8660254037844387076, 1.000000000000000000, 0.8660254037844387076, 1.000000000000000000, 0.8660254037844387076, 1.000000000000000000, 0.8660254037844387076, 1.000000000000000000, 0.8660254037844387076, 1.000000000000000000, 0.8660254037844387076, 1.000000000000000000, 0.8660254037844387076, 1.000000000000000000, 0.8660254037844387076, 1.000000000000000000, 0.8660254037844387076, 1.000000000000000000, 0.8660254037844387076, 1.000000000000000000, 0.8660254037844387076, 1.000000000000000000, 0.8660254037844387076, 1.000000000000000000, 0.8660254037844387076, 1.000000000000000000, 0.8660254037844387076, 1.000000000000000000, 0.8660254037844387076, 1.000000000000000000, 0.8660254037844387076, 1.000000000000000000, 0.8660254037844387076, 1.000000000000000000, 0.8660254037844387076, 1.000000000000000000, 0.8660254037844387076, 1.000000000000000000, 0.8660254037844387076, 1.000000000000000000, 0.8660254037844387076, 1.000000000000000000, 0.8660254037844387076, 1.000000000000000000, 0.8660254037844387076, 1.000000000000000000, 0.8660254037844387076, 1.000000000000000000, 0.8660254037844387076, 1.000000000000000000, 0.8660254037844387076, 1.000000000000000000, 0.8660254037844387076, 1.000000000000000000, 0.8660254037844387076, 1.000000000000000000, 0.8660254037844387076, 1.000000000000000000, 0.8660254037844387076, 1.000000000000000000, 0.8660254037844387076, 1.000000000000000000, 0.8660254037844387076, 1.000000000000000000, 0.8660254037844387076, 1.000000000000000000, 0.9548847324609573972, 0.9401541411607521326) ) ) 
 REPRESENTATION_ITEM ( '' )  SURFACE ( )  );
#28978 = CARTESIAN_POINT ( 'NONE',  ( 20.99999999999999645, 243.1093750006145342, 6.646953231504538984 ) ) ;
#28979 = CARTESIAN_POINT ( 'NONE',  ( 8.715434833792128799, 55.93981371789855217, -8.962234695871567070 ) ) ;
#28980 = CARTESIAN_POINT ( 'NONE',  ( 16.56230152254410726, 0.000000000000000000, 0.000000000000000000 ) ) ;
#28981 = CARTESIAN_POINT ( 'NONE',  ( 0.1745138560725515708, 97.81018628210144072, -12.50000000000000355 ) ) ;
#28982 = CARTESIAN_POINT ( 'NONE',  ( 16.56230152254411081, 6.928203230275506996, -2.699999998771040577 ) ) ;
#28983 = CARTESIAN_POINT ( 'NONE',  ( -35.35788769728823411, 216.4690446883607535, 1.857196546604031662 ) ) ;
#28984 = CARTESIAN_POINT ( 'NONE',  ( -29.00000000000002487, 210.0000000000000000, 8.000000000000000000 ) ) ;
#28985 = CARTESIAN_POINT ( 'NONE',  ( 15.00000000000000000, 241.0562500012290457, 0.000000000000000000 ) ) ;
#28986 = CARTESIAN_POINT ( 'NONE',  ( -6.092822981423970496, 93.78518628210144925, 14.25334919248782661 ) ) ;
#28987 = CARTESIAN_POINT ( 'NONE',  ( 8.962234695871762469, 6.960186282101432198, -8.715434833791931624 ) ) ;
#28988 = CARTESIAN_POINT ( 'NONE',  ( 0.000000000000000000, 210.0000000000000284, -27.00000000000000000 ) ) ;
#28989 = CARTESIAN_POINT ( 'NONE',  ( 16.56230152254410726, 0.000000000000000000, -10.00000000000000000 ) ) ;
#28990 = CARTESIAN_POINT ( 'NONE',  ( -6.840914352312096547, 131.1601862821014777, 6.594114490232313663 ) ) ;
#28991 = FACE_OUTER_BOUND ( 'NONE', #28410, .T. ) ;
#28992 = CARTESIAN_POINT ( 'NONE',  ( 18.12178482187500350, 242.1718750006145058, 4.985214923628407568 ) ) ;
#28993 = ORIENTED_EDGE ( 'NONE', *, *, #14737, .T. ) ;
#28994 = CARTESIAN_POINT ( 'NONE',  ( 25.15145004905768644, -3.604726614523240613, 169.0882189147961583 ) ) ;
#28995 = CARTESIAN_POINT ( 'NONE',  ( -1.715153634034234598, 69.92268628210143788, -9.534712964251941258 ) ) ;
#28996 = CARTESIAN_POINT ( 'NONE',  ( 26.75643035624999655, 3.323476615752271712, -0.3281249993854667424 ) ) ;
#28997 = CARTESIAN_POINT ( 'NONE',  ( 0.000000000000000000, 210.0000000000000284, 0.000000000000000000 ) ) ;
#28998 = CARTESIAN_POINT ( 'NONE',  ( 15.00000000000000000, 242.3687500012290741, -3.464101615137752610 ) ) ;
#28999 = DIRECTION ( 'NONE',  ( 0.000000000000000000, 0.000000000000000000, 1.000000000000000000 ) ) ;
#29000 = CARTESIAN_POINT ( 'NONE',  ( -13.49999999999998401, 197.0375000012290627, 23.38268590217985476 ) ) ;
#29001 = CARTESIAN_POINT ( 'NONE',  ( 9.465287035748106703, 47.60231371789853938, -2.064181346179063237 ) ) ;
#29002 = CARTESIAN_POINT ( 'NONE',  ( -13.62178482187498396, 199.4843750006145626, 23.59362340125808188 ) ) ;
#29003 = VERTEX_POINT ( 'NONE', #35558 ) ;
#29004 = ORIENTED_EDGE ( 'NONE', *, *, #9673, .F. ) ;
#29005 = CARTESIAN_POINT ( 'NONE',  ( 15.00000000000000000, 239.7062500012290513, 0.000000000000000000 ) ) ;
#29006 = CARTESIAN_POINT ( 'NONE',  ( 11.48171059495408208, 38.11481371789854222, -4.944772684328420986 ) ) ;
#29007 = CARTESIAN_POINT ( 'NONE',  ( 13.44051670066911264, -5.407089921784865361, -7.771874999385531169 ) ) ;
#29008 = CARTESIAN_POINT ( 'NONE',  ( 26.75643035624999655, 7.049594010296217766E-16, -9.928124999385474325 ) ) ;
#29009 = CARTESIAN_POINT ( 'NONE',  ( -12.53471296425189152, 6.777313717898553413, -2.311890736173453753 ) ) ;
#29010 = ORIENTED_EDGE ( 'NONE', *, *, #22684, .T. ) ;
#29011 = CARTESIAN_POINT ( 'NONE',  ( 22.80587116629412137, 7.646167579472024665E-16, -3.121874999385543248 ) ) ;
#29012 = CARTESIAN_POINT ( 'NONE',  ( 13.62178482187499640, 199.6531250006145228, -23.59362340125807123 ) ) ;
#29013 = CARTESIAN_POINT ( 'NONE',  ( 31.29445502703164905, -7.209453229046482114, 167.6661593874051164 ) ) ;
#29014 = CARTESIAN_POINT ( 'NONE',  ( -32.18377896937850835, 208.3738570449995109, 6.530955311639247363 ) ) ;
#29015 = CARTESIAN_POINT ( 'NONE',  ( 20.99999999999999645, 249.6343750006145399, -6.646953231504538984 ) ) ;
#29016 = CARTESIAN_POINT ( 'NONE',  ( -26.88106477066232713, 195.0000000000000568, 3.495181417218032660 ) ) ;
#29017 = CARTESIAN_POINT ( 'NONE',  ( -56.32961230271183695, 211.3212981617417938, 4.469044688360757966 ) ) ;
#29019 = EDGE_CURVE ( 'NONE', #5529, #32564, #872, .T. ) ;
#29018 = CARTESIAN_POINT ( 'NONE',  ( -38.32663769728824121, 204.3130714775002730, 3.149950860017883603 ) ) ;
#29020 = CARTESIAN_POINT ( 'NONE',  ( 37.52570519453759346, -3.604726614523235284, 167.2527469918319412 ) ) ;
#29021 = ORIENTED_EDGE ( 'NONE', *, *, #7091, .F. ) ;
#29022 = CARTESIAN_POINT ( 'NONE',  ( 25.16776026727616511, 0.000000000000000000, 166.4799973143651926 ) ) ;
#29023 = CARTESIAN_POINT ( 'NONE',  ( 36.91619120224290640, 7.347880794884117764E-16, 163.0806184283759706 ) ) ;
#29024 = VECTOR ( 'NONE', #22632, 1000.000000000000000 ) ;
#29025 = CARTESIAN_POINT ( 'NONE',  ( 2.908627838312458636, 18.27731371789853299, -15.53471296425188442 ) ) ;
#29026 = CARTESIAN_POINT ( 'NONE',  ( -58.71205436395490551, 216.1378603801730094, 6.307003348497944195 ) ) ;
#29027 = CARTESIAN_POINT ( 'NONE',  ( -10.49813415415989581, 13.57268628210145600, -7.228626920339068285 ) ) ;
#29028 = CARTESIAN_POINT ( 'NONE',  ( -4.944772684328673229, 56.98518628210144499, 11.48171059495397728 ) ) ;
#29030 = EDGE_CURVE ( 'NONE', #13411, #24114, #19685, .T. ) ;
#29029 = CARTESIAN_POINT ( 'NONE',  ( 13.56230152254411792, -5.196152422706638241, -4.425000000000068212 ) ) ;
#29031 = ORIENTED_EDGE ( 'NONE', *, *, #6641, .F. ) ;
#29032 = CARTESIAN_POINT ( 'NONE',  ( -37.13913769728823411, 206.8500491399821044, -5.686928522499717253 ) ) ;
#29033 = CARTESIAN_POINT ( 'NONE',  ( 15.00000000000000178, 242.3875000000000171, 3.464101615137757051 ) ) ;
#29034 = CARTESIAN_POINT ( 'NONE',  ( -27.24356964374999635, 195.3968750006145569, 15.72908226750539384 ) ) ;
#29035 = LINE ( 'NONE', #8776, #31682 ) ;
#29036 = FACE_OUTER_BOUND ( 'NONE', #32240, .T. ) ;
#29037 = CARTESIAN_POINT ( 'NONE',  ( 13.50000000000001421, 197.4500000000000171, 23.38268590217984055 ) ) ;
#29038 = EDGE_CURVE ( 'NONE', #14348, #33950, #9224, .T. ) ;
#29039 = CARTESIAN_POINT ( 'NONE',  ( 18.12178482187500350, 244.9843750006145342, 4.985214923628407568 ) ) ;
#29040 = CARTESIAN_POINT ( 'NONE',  ( -3.796722387233185003, 91.01481371789856212, -8.710071997420207879 ) ) ;
#29041 = LINE ( 'NONE', #21111, #19093 ) ;
#29042 = ORIENTED_EDGE ( 'NONE', *, *, #18881, .T. ) ;
#29043 = CARTESIAN_POINT ( 'NONE',  ( -56.13913769728823411, 206.8500491399821044, -5.686928522499717253 ) ) ;
#29044 = LINE ( 'NONE', #37208, #19034 ) ;
#29045 = EDGE_CURVE ( 'NONE', #5775, #2631, #27044, .T. ) ;
#29046 = CARTESIAN_POINT ( 'NONE',  ( 18.00000000000000000, 246.3812500012290343, -5.196152422706630247 ) ) ;
#29047 = CARTESIAN_POINT ( 'NONE',  ( -11.61527771782809282, 99.06481371789855928, -4.622313124798832717 ) ) ;
#29048 = CARTESIAN_POINT ( 'NONE',  ( 22.80587116629411781, 3.604726614523243278, -0.3843749993855423153 ) ) ;
#29049 = CARTESIAN_POINT ( 'NONE',  ( 10.56230152254410726, 0.000000000000000000, -1.350000000000045608 ) ) ;
#29050 = CARTESIAN_POINT ( 'NONE',  ( 21.00000000000000000, -6.646953231504538984, -1.490624999385501193 ) ) ;
#29051 = CARTESIAN_POINT ( 'NONE',  ( -8.962234695871565293, 72.03981371789855359, -8.715434833792128799 ) ) ;
#29052 = CARTESIAN_POINT ( 'NONE',  ( -1.926257025242585782E-15, 198.3968750006145285, -31.45816453501075927 ) ) ;
#29053 = ORIENTED_EDGE ( 'NONE', *, *, #8031, .F. ) ;
#29054 = ORIENTED_EDGE ( 'NONE', *, *, #21957, .F. ) ;
#29055 = AXIS2_PLACEMENT_3D ( 'NONE', #25612, #8375, #10463 ) ;
#29056 = EDGE_LOOP ( 'NONE', ( #23554, #7951, #33852, #2692 ) ) ;
#29057 = CARTESIAN_POINT ( 'NONE',  ( 26.75643035624999655, -3.323476615752267271, -4.903124999385481964 ) ) ;
#29058 = LINE ( 'NONE', #15236, #33631 ) ;
#29059 = CARTESIAN_POINT ( 'NONE',  ( 23.87821517812500005, 245.8468750006145171, 4.985214923628404016 ) ) ;
#29060 = CARTESIAN_POINT ( 'NONE',  ( 10.69584247140445221, 44.04768628210144499, -6.932735513423970097 ) ) ;
#29061 = CARTESIAN_POINT ( 'NONE',  ( -48.61086230271182984, 213.1499508600178387, -5.686928522499747451 ) ) ;
#29062 = CARTESIAN_POINT ( 'NONE',  ( 16.47967912936614709, 222.0541889883613749, -3.964960503604720632 ) ) ;
#29063 = CARTESIAN_POINT ( 'NONE',  ( -33.17336230271183695, 213.9548777149308023, 2.149950860017852960 ) ) ;
#29064 = AXIS2_PLACEMENT_3D ( 'NONE', #33049, #15434, #12769 ) ;
#29065 = CARTESIAN_POINT ( 'NONE',  ( 30.87038786627866216, 6.928203230275506996, 162.8190495601146495 ) ) ;
#29066 = CARTESIAN_POINT ( 'NONE',  ( 8.962234695871567070, 95.03981371789856780, 8.715434833792127023 ) ) ;
#29067 = CARTESIAN_POINT ( 'NONE',  ( -64.84747103062156270, 212.3500491399821613, -3.839350919129076445 ) ) ;
#29068 =( BOUNDED_CURVE ( )  B_SPLINE_CURVE ( 2, ( #5635, #27836, #1867, #34081, #3358, #25924, #29319, #23836, #23277 ),
 .UNSPECIFIED., .F., .F. ) 
 B_SPLINE_CURVE_WITH_KNOTS ( ( 3, 2, 2, 2, 3 ),
 ( 0.2500000000000000000, 0.2536231884057971175, 0.2608695652173912971, 0.2681159420289855322, 0.2717391304347825942 ),
 .UNSPECIFIED. ) 
 CURVE ( )  GEOMETRIC_REPRESENTATION_ITEM ( )  RATIONAL_B_SPLINE_CURVE ( ( 0.9330127018922194093, 0.9330127018922190762, 1.000000000000000000, 0.8660254037844387076, 1.000000000000000000, 0.8660254037844387076, 1.000000000000000000, 0.9330127018922198534, 0.9330127018922191873 ) ) 
 REPRESENTATION_ITEM ( '' )  );
#29069 = CARTESIAN_POINT ( 'NONE',  ( -39.11830436395489841, 209.8844732041983150, 8.500000000000003553 ) ) ;
#29070 = CARTESIAN_POINT ( 'NONE',  ( 26.75643035624999655, -3.323476615752267271, -3.665624999385486138 ) ) ;
#29071 = CARTESIAN_POINT ( 'NONE',  ( 26.99999999999999645, 7.347880794884117764E-16, -1.574999999999993072 ) ) ;
#29072 = CARTESIAN_POINT ( 'NONE',  ( -14.38691631536193860, 80.66481371789856780, -5.770363421894132649 ) ) ;
#29073 = CARTESIAN_POINT ( 'NONE',  ( -61.07961230271182984, 212.3930949314663792, 8.469044688360751749 ) ) ;
#29074 = EDGE_CURVE ( 'NONE', #13953, #17429, #9602, .T. ) ;
#29075 = ORIENTED_EDGE ( 'NONE', *, *, #17007, .T. ) ;
#29076 = CARTESIAN_POINT ( 'NONE',  ( 16.56230152254410726, 0.000000000000000000, 0.000000000000000000 ) ) ;
#29077 = CARTESIAN_POINT ( 'NONE',  ( -10.69584247140444866, 103.8476862821014493, 6.932735513423972762 ) ) ;
#29078 = CARTESIAN_POINT ( 'NONE',  ( 8.632099005475504683, 37.14768628210143220, 13.23911966647218996 ) ) ;
#29080 = ADVANCED_FACE ( 'NONE', ( #681 ), #30254, .T. ) ;
#29079 = CARTESIAN_POINT ( 'NONE',  ( 10.56230152254410903, 0.000000000000000000, -9.787499998771043153 ) ) ;
#29081 = CARTESIAN_POINT ( 'NONE',  ( 37.09265009776020605, 7.646167579472024665E-16, 162.3029045856885659 ) ) ;
#29082 = CARTESIAN_POINT ( 'NONE',  ( -15.53471296425195369, 67.62268628210145494, 2.908627838312118019 ) ) ;
#29083 = CARTESIAN_POINT ( 'NONE',  ( -27.24356964375000345, 198.9031250006145228, 0.000000000000000000 ) ) ;
#29084 = ADVANCED_FACE ( 'NONE', ( #1245 ), #3907, .F. ) ;
#29085 = CARTESIAN_POINT ( 'NONE',  ( 10.31873187879410914, 0.000000000000000000, -8.240624999385548932 ) ) ;
#29086 = CARTESIAN_POINT ( 'NONE',  ( 19.56230152254411792, 5.196152422706637353, -8.700000000000041922 ) ) ;
#29087 = CARTESIAN_POINT ( 'NONE',  ( -45.64955436395490551, 214.8429017333601792, -4.673758765035196383 ) ) ;
#29088 = CARTESIAN_POINT ( 'NONE',  ( -2.660918448318275509, 47.49768628210144783, 12.46528703574805874 ) ) ;
#29089 = CARTESIAN_POINT ( 'NONE',  ( -27.00000000000000355, 195.4625000000000057, -15.58845726811989429 ) ) ;
#29090 = CARTESIAN_POINT ( 'NONE',  ( -13.49999999999998401, 197.9375000012290400, 23.38268590217985476 ) ) ;
#29091 = CARTESIAN_POINT ( 'NONE',  ( 6.840914352312096547, 16.16018628210144570, -6.594114490232313663 ) ) ;
#29092 = CARTESIAN_POINT ( 'NONE',  ( 26.75643035624999655, 245.9968750006145513, 3.323476615752267271 ) ) ;
#29093 = ORIENTED_EDGE ( 'NONE', *, *, #7630, .F. ) ;
#29094 = CARTESIAN_POINT ( 'NONE',  ( 18.00000000000000355, -5.196152422706632912, -5.775000000000002132 ) ) ;
#29095 = CARTESIAN_POINT ( 'NONE',  ( 24.00000000000000000, 243.4000000000000057, 5.196152422706629359 ) ) ;
#29096 = EDGE_CURVE ( 'NONE', #8916, #18637, #14387, .T. ) ;
#29097 = CARTESIAN_POINT ( 'NONE',  ( 36.87697111800645899, 7.347880794884117764E-16, 162.6323308142347059 ) ) ;
#29098 = CARTESIAN_POINT ( 'NONE',  ( 10.31873187879411269, -3.604726614523240613, -4.603124999385506122 ) ) ;
#29099 = CARTESIAN_POINT ( 'NONE',  ( 37.37209319794485651, 7.646167579472015790E-16, 165.4969538364452148 ) ) ;
#29100 = CARTESIAN_POINT ( 'NONE',  ( 15.00000000000000178, 241.9375000000000000, 3.464101615137757051 ) ) ;
#29101 = DIRECTION ( 'NONE',  ( -0.000000000000000000, -0.000000000000000000, 1.000000000000000000 ) ) ;
#29102 = CARTESIAN_POINT ( 'NONE',  ( -11.61527771782819940, 76.53518628210146346, 4.622313124798574258 ) ) ;
#29103 = ORIENTED_EDGE ( 'NONE', *, *, #34155, .F. ) ;
#29104 = EDGE_LOOP ( 'NONE', ( #24424, #14997 ) ) ;
#29105 = CARTESIAN_POINT ( 'NONE',  ( 20.99999999999995026, 240.9437500012290911, -5.999999999999998224 ) ) ;
#29106 = CYLINDRICAL_SURFACE ( 'NONE', #30610, 5.999999999999999112 ) ;
#29107 = CARTESIAN_POINT ( 'NONE',  ( 26.75643035624999655, 3.323476615752271712, -7.528124999385462424 ) ) ;
#29108 = CARTESIAN_POINT ( 'NONE',  ( -14.25334919248795096, 42.71481371789855075, 6.092822981423662299 ) ) ;
#29109 = CARTESIAN_POINT ( 'NONE',  ( 15.00000000000000000, 0.000000000000000000, -5.343749998770963572 ) ) ;
#29110 = CARTESIAN_POINT ( 'NONE',  ( 15.24356964374999990, 241.3093750006145228, 0.000000000000000000 ) ) ;
#29111 = AXIS2_PLACEMENT_3D ( 'NONE', #12359, #20904, #24492 ) ;
#29112 = CARTESIAN_POINT ( 'NONE',  ( -37.93080436395490551, 205.4999999999999716, -0.1155267958017894420 ) ) ;
#29113 = CARTESIAN_POINT ( 'NONE',  ( 22.56230152254410370, 0.000000000000000000, -10.00000000000000000 ) ) ;
#29114 = CARTESIAN_POINT ( 'NONE',  ( 24.35887751344623098, 0.000000000000000000, 160.0290733790243962 ) ) ;
#29115 = CARTESIAN_POINT ( 'NONE',  ( 6.594114490232462877, 28.33981371789855430, -6.840914352311949109 ) ) ;
#29116 = CARTESIAN_POINT ( 'NONE',  ( -53.56622103062157692, 211.6261429550005744, 6.530955311639227823 ) ) ;
#29117 = CARTESIAN_POINT ( 'NONE',  ( -36.53794563604517265, 203.8621396198271043, 6.307003348498029460 ) ) ;
#29118 = SHAPE_DEFINITION_REPRESENTATION ( #29543, #10397 ) ;
#29119 = DIRECTION ( 'NONE',  ( 0.000000000000000000, 0.000000000000000000, -1.000000000000000000 ) ) ;
#29120 = CARTESIAN_POINT ( 'NONE',  ( 13.62178482187499640, 196.5593750006145513, -23.59362340125807123 ) ) ;
#29121 = CARTESIAN_POINT ( 'NONE',  ( -11.08355503943118592, 127.2398137178985422, -10.83675517735179383 ) ) ;
#29122 = ADVANCED_FACE ( 'NONE', ( #6755 ), #18329, .F. ) ;
#29123 = ORIENTED_EDGE ( 'NONE', *, *, #15018, .F. ) ;
#29124 = CARTESIAN_POINT ( 'NONE',  ( -12.53471296425194836, 49.22268628210144215, 2.311890736173176641 ) ) ;
#29125 = CARTESIAN_POINT ( 'NONE',  ( -4.632842373742755981, 226.1292383950976159, -2.500000000000000000 ) ) ;
#29126 = CARTESIAN_POINT ( 'NONE',  ( 23.43386378601147513, 5.229754410370055062, -8.000000000000001776 ) ) ;
#29127 = CARTESIAN_POINT ( 'NONE',  ( 28.29894145125277660, -5.407089921784865361, 169.2457464034993961 ) ) ;
#29128 = CARTESIAN_POINT ( 'NONE',  ( 15.00000000000000000, 0.000000000000000000, -2.643749998770955401 ) ) ;
#29129 =( BOUNDED_CURVE ( )  B_SPLINE_CURVE ( 2, ( #7104, #18484, #21513, #7468, #33427, #30598, #9932, #4613, #27180 ),
 .UNSPECIFIED., .F., .T. ) 
 B_SPLINE_CURVE_WITH_KNOTS ( ( 3, 2, 2, 2, 3 ),
 ( 0.02083333333333333565, 0.02777777777777777624, 0.04166666666666666435, 0.05555555555555555247, 0.06250000000000000000 ),
 .UNSPECIFIED. ) 
 CURVE ( )  GEOMETRIC_REPRESENTATION_ITEM ( )  RATIONAL_B_SPLINE_CURVE ( ( 0.9330127018922194093, 0.9330127018922194093, 1.000000000000000000, 0.8660254037844387076, 1.000000000000000000, 0.8660254037844387076, 1.000000000000000000, 0.9330127018922194093, 0.9330127018922194093 ) ) 
 REPRESENTATION_ITEM ( '' )  );
#29130 = CARTESIAN_POINT ( 'NONE',  ( 10.31873187879411091, 3.604726614523240613, -9.684374999385527261 ) ) ;
#29131 = CARTESIAN_POINT ( 'NONE',  ( -68.21205436395490551, 214.6737587650351884, 4.842901733360205796 ) ) ;
#29132 = CIRCLE ( 'NONE', #30373, 1.000000000000002220 ) ;
#29133 = CARTESIAN_POINT ( 'NONE',  ( -5.529263428287477744, 57.27268628210143220, 7.954856959092191815 ) ) ;
#29134 = DIRECTION ( 'NONE',  ( 0.000000000000000000, 0.000000000000000000, 1.000000000000000000 ) ) ;
#29135 = CARTESIAN_POINT ( 'NONE',  ( 10.49999999999999645, 244.5000000000000000, 5.000000000000000000 ) ) ;
#29136 = CARTESIAN_POINT ( 'NONE',  ( -10.49813415415989581, 96.37268628210145494, -7.228626920339068285 ) ) ;
#29137 = LINE ( 'NONE', #896, #22120 ) ;
#29138 = DIRECTION ( 'NONE',  ( 0.000000000000000000, 0.000000000000000000, -1.000000000000000000 ) ) ;
#29139 = ORIENTED_EDGE ( 'NONE', *, *, #8349, .F. ) ;
#29140 = CARTESIAN_POINT ( 'NONE',  ( 27.70246933682352974, 5.407089921784856479, 162.4280389384339855 ) ) ;
#29141 = CARTESIAN_POINT ( 'NONE',  ( 26.75643035624999655, 7.049594010296217766E-16, -8.465624999385468641 ) ) ;
#29142 = CARTESIAN_POINT ( 'NONE',  ( 28.02440086159767674, -5.407089921784865361, 166.1077331045103733 ) ) ;
#29143 = CARTESIAN_POINT ( 'NONE',  ( 25.05010001456683710, 0.000000000000000000, 165.1351344719413419 ) ) ;
#29144 = CARTESIAN_POINT ( 'NONE',  ( -27.00000000000000355, 198.1625000000000227, -15.58845726811989429 ) ) ;
#29145 = CARTESIAN_POINT ( 'NONE',  ( 26.99999999999999645, 248.4624999999999773, -3.464101615137755275 ) ) ;
#29146 = CARTESIAN_POINT ( 'NONE',  ( 27.24356964375000700, 198.6406250006145342, 15.72908226750537075 ) ) ;
#29147 = CARTESIAN_POINT ( 'NONE',  ( -11.61527771782809282, 126.6648137178985678, -4.622313124798832717 ) ) ;
#29148 = CARTESIAN_POINT ( 'NONE',  ( -8.715434833791929847, 124.2601862821014578, -8.962234695871762469 ) ) ;
#29150 = ORIENTED_EDGE ( 'NONE', *, *, #32161, .F. ) ;
#29149 = VERTEX_POINT ( 'NONE', #27034 ) ;
#29151 = CARTESIAN_POINT ( 'NONE',  ( 27.24356964375000345, 199.1281250006145171, -3.336375036156643733E-15 ) ) ;
#29152 = CARTESIAN_POINT ( 'NONE',  ( 26.75643035624999655, 242.8093750006144944, -3.323476615752271712 ) ) ;
#29153 = CARTESIAN_POINT ( 'NONE',  ( -2.908627838312453306, 87.27731371789855075, 15.53471296425188797 ) ) ;
#29154 = CARTESIAN_POINT ( 'NONE',  ( 21.00000000000000000, 6.646953231504538984, -5.315624999385480720 ) ) ;
#29155 = CARTESIAN_POINT ( 'NONE',  ( 26.75643035624999655, 246.4468750006144830, 3.323476615752267715 ) ) ;
#29156 = AXIS2_PLACEMENT_3D ( 'NONE', #12881, #9479, #18393 ) ;
#29157 = CARTESIAN_POINT ( 'NONE',  ( 5.727106289114498080E-15, 196.1750000012290513, 31.17691453623979214 ) ) ;
#29158 = CARTESIAN_POINT ( 'NONE',  ( -6.594114490232462877, 78.93981371789855928, 6.840914352311949109 ) ) ;
#29159 = CARTESIAN_POINT ( 'NONE',  ( 19.68408634441910365, -5.407089921784855591, -6.290624999385540761 ) ) ;
#29160 = EDGE_CURVE ( 'NONE', #10660, #1475, #1057, .T. ) ;
#29161 = CARTESIAN_POINT ( 'NONE',  ( 26.75643035624999655, 242.3218750006145399, -7.049594010296217766E-16 ) ) ;
#29162 = CARTESIAN_POINT ( 'NONE',  ( 6.932735513424201024, 55.65231371789855785, -10.69584247140429412 ) ) ;
#29163 = EDGE_CURVE ( 'NONE', #9189, #33064, #9787, .T. ) ;
#29164 = DIRECTION ( 'NONE',  ( 1.000000000000000000, 0.000000000000000000, 0.000000000000000000 ) ) ;
#29165 = CARTESIAN_POINT ( 'NONE',  ( 4.622313124798573369, 92.63518628210145778, 11.61527771782819940 ) ) ;
#29166 = CARTESIAN_POINT ( 'NONE',  ( 10.56230152254411081, 0.000000000000000000, -2.587499998771031429 ) ) ;
#29167 = ADVANCED_FACE ( 'NONE', ( #6957 ), #18525, .F. ) ;
#29168 = CARTESIAN_POINT ( 'NONE',  ( -64.25372103062157692, 214.5309553116392749, -1.090244570138262148 ) ) ;
#29169 = CARTESIAN_POINT ( 'NONE',  ( 26.99999999999999645, 7.347880794884117764E-16, -2.024999999999999023 ) ) ;
#29170 = CARTESIAN_POINT ( 'NONE',  ( 15.00000000000000178, 241.0937500012290400, 3.464101615137757051 ) ) ;
#29171 = CARTESIAN_POINT ( 'NONE',  ( 15.50000000000000533, 100.1101862821014521, 0.1745138560725827404 ) ) ;
#29172 = CARTESIAN_POINT ( 'NONE',  ( 25.22417062191275861, 0.000000000000000000, 169.9194188660164571 ) ) ;
#29173 = CARTESIAN_POINT ( 'NONE',  ( 18.00000000000000355, -5.196152422706632912, -0.3749999999999864553 ) ) ;
#29174 =( BOUNDED_CURVE ( )  B_SPLINE_CURVE ( 2, ( #14526, #26082, #5249, #8840, #23250, #34796, #20412 ),
 .UNSPECIFIED., .F., .F. ) 
 B_SPLINE_CURVE_WITH_KNOTS ( ( 3, 2, 2, 3 ),
 ( 0.04347826086956579211, 0.05072463768116009658, 0.05797101449275439411, 0.06521739130434869858 ),
 .UNSPECIFIED. ) 
 CURVE ( )  GEOMETRIC_REPRESENTATION_ITEM ( )  RATIONAL_B_SPLINE_CURVE ( ( 0.9999999999999893419, 0.8660254037844493658, 1.000000000000000000, 0.8660254037844387076, 1.000000000000000000, 0.8660254037844226094, 1.000000000000016209 ) ) 
 REPRESENTATION_ITEM ( '' )  );
#29175 = CARTESIAN_POINT ( 'NONE',  ( 0.000000000000000000, 148.0000000000000000, -24.80000000000000426 ) ) ;
#29176 = CARTESIAN_POINT ( 'NONE',  ( 9.534712964251941258, 118.2226862821014493, -1.715153634034235708 ) ) ;
#29177 = DIRECTION ( 'NONE',  ( 0.000000000000000000, 0.000000000000000000, 1.000000000000000000 ) ) ;
#29178 = CARTESIAN_POINT ( 'NONE',  ( 3.257655550457285720, 15.29768628210142722, -15.46528703574804986 ) ) ;
#29179 = CARTESIAN_POINT ( 'NONE',  ( 27.24356964374999635, 195.1718750006145342, -15.72908226750539029 ) ) ;
#29180 = CARTESIAN_POINT ( 'NONE',  ( 18.12178482187499640, 241.5718750006145399, -4.985214923628404904 ) ) ;
#29181 = VERTEX_POINT ( 'NONE', #27220 ) ;
#29182 = CYLINDRICAL_SURFACE ( 'NONE', #15516, 5.999999999999994671 ) ;
#29183 = CARTESIAN_POINT ( 'NONE',  ( 2.064181346179272847, 70.49768628210145494, -9.465287035748065847 ) ) ;
#29184 = CARTESIAN_POINT ( 'NONE',  ( 26.75643035624999655, 3.323476615752271712, -0.7781249993854945091 ) ) ;
#29185 = CARTESIAN_POINT ( 'NONE',  ( 20.99999999999999289, 241.7874999999999659, -5.999999999999997335 ) ) ;
#29186 = CARTESIAN_POINT ( 'NONE',  ( 20.99999999999995026, 243.1375000000000455, -5.999999999999998224 ) ) ;
#29187 = CARTESIAN_POINT ( 'NONE',  ( 5.778771075727756162E-15, 195.4718750006145456, 31.45816453501075927 ) ) ;
#29188 = CARTESIAN_POINT ( 'NONE',  ( -6.245661213598732608, 195.0000000000000853, 26.53257588854514637 ) ) ;
#29189 = CARTESIAN_POINT ( 'NONE',  ( -4.694659320240884604E-14, 197.0750000012290570, 27.00000000000000000 ) ) ;
#29190 = CARTESIAN_POINT ( 'NONE',  ( 6.594114490232462877, 46.73981371789855643, -6.840914352311949109 ) ) ;
#29191 = CARTESIAN_POINT ( 'NONE',  ( -13.62178482187500528, 199.3343750006145569, -23.59362340125807123 ) ) ;
#29192 = VERTEX_POINT ( 'NONE', #34531 ) ;
#29193 = ORIENTED_EDGE ( 'NONE', *, *, #5043, .F. ) ;
#29194 = CARTESIAN_POINT ( 'NONE',  ( 18.00000000000000355, 239.7812500012290400, 5.196152422706632912 ) ) ;
#29195 = CARTESIAN_POINT ( 'NONE',  ( -10.69584247140429412, 34.95231371789854791, -6.932735513424201024 ) ) ;
#29196 = CARTESIAN_POINT ( 'NONE',  ( 19.68408634441912142, -5.407089921784861808, -8.146874999385516958 ) ) ;
#29197 = CARTESIAN_POINT ( 'NONE',  ( 18.12178482187500350, -4.985214923628407568, -9.178124999385472549 ) ) ;
#29198 = CARTESIAN_POINT ( 'NONE',  ( 0.1745138560722779009, 13.38981371789854613, 12.50000000000000355 ) ) ;
#29199 =( BOUNDED_CURVE ( )  B_SPLINE_CURVE ( 2, ( #22520, #33884, #19500, #28006, #16649, #13422, #16276 ),
 .UNSPECIFIED., .F., .F. ) 
 B_SPLINE_CURVE_WITH_KNOTS ( ( 3, 2, 2, 3 ),
 ( 0.2391304347826079535, 0.2463768115942022718, 0.2536231884057966179, 0.2608695652173909085 ),
 .UNSPECIFIED. ) 
 CURVE ( )  GEOMETRIC_REPRESENTATION_ITEM ( )  RATIONAL_B_SPLINE_CURVE ( ( 1.000000000000013989, 0.8660254037844249408, 1.000000000000000000, 0.8660254037844387076, 1.000000000000000000, 0.8660254037844459241, 0.9999999999999927836 ) ) 
 REPRESENTATION_ITEM ( '' )  );
#29200 = CARTESIAN_POINT ( 'NONE',  ( 21.00000000000000000, 247.8624999999999545, 5.999999999999998224 ) ) ;
#29201 = ORIENTED_EDGE ( 'NONE', *, *, #1909, .F. ) ;
#29202 = CARTESIAN_POINT ( 'NONE',  ( 13.44051670066911086, -5.407089921784865361, -2.821874999385520777 ) ) ;
#29203 = ORIENTED_EDGE ( 'NONE', *, *, #33700, .T. ) ;
#29204 = CARTESIAN_POINT ( 'NONE',  ( -27.24356964375000345, 198.9031250006145228, 0.000000000000000000 ) ) ;
#29205 = CARTESIAN_POINT ( 'NONE',  ( 28.06362094583411704, -5.407089921784865361, 166.5560207186516664 ) ) ;
#29206 = CARTESIAN_POINT ( 'NONE',  ( -67.80877896937849414, 212.1620413398627534, -8.530955311639255356 ) ) ;
#29207 = CARTESIAN_POINT ( 'NONE',  ( 26.75643035624999655, 248.6218750006145228, -7.049594010296217766E-16 ) ) ;
#29208 = FILL_AREA_STYLE ('',( #14823 ) ) ;
#29209 = DIRECTION ( 'NONE',  ( 0.000000000000000000, 0.000000000000000000, -1.000000000000000000 ) ) ;
#29210 = CARTESIAN_POINT ( 'NONE',  ( -52.17336230271184405, 213.9548777149308023, 2.149950860017852960 ) ) ;
#29211 = DIRECTION ( 'NONE',  ( 0.08715574274765150453, 0.000000000000000000, 0.9961946980917461003 ) ) ;
#29212 = CARTESIAN_POINT ( 'NONE',  ( 37.64336544724691436, -3.604726614523235284, 168.5976098342557918 ) ) ;
#29213 = ORIENTED_EDGE ( 'NONE', *, *, #36432, .F. ) ;
#29214 = CARTESIAN_POINT ( 'NONE',  ( 22.60769515458672885, 241.6388461906613259, 5.999999999999997335 ) ) ;
#29215 = CARTESIAN_POINT ( 'NONE',  ( 13.04141134922778988, 19.42731371789854933, -8.927990412390371944 ) ) ;
#29216 = CARTESIAN_POINT ( 'NONE',  ( -62.67038769728824121, 207.6069050685337913, 8.469044688360781947 ) ) ;
#29217 = PRODUCT_DEFINITION_SHAPE ( 'NONE', 'NONE',  #37507 ) ;
#29218 = CARTESIAN_POINT ( 'NONE',  ( 9.534712964251941258, 136.6226862821014549, -1.715153634034235708 ) ) ;
#29219 = CARTESIAN_POINT ( 'NONE',  ( 10.49813415415989581, 45.77268628210144641, 7.228626920339068285 ) ) ;
#29220 = CARTESIAN_POINT ( 'NONE',  ( 10.56230152254411436, -3.464101615137761048, -3.562500000000032863 ) ) ;
#29221 = ORIENTED_EDGE ( 'NONE', *, *, #29782, .F. ) ;
#29222 = CARTESIAN_POINT ( 'NONE',  ( -47.43080436395489841, 203.5000000000000000, -0.1155267958017335561 ) ) ;
#29223 = MECHANICAL_DESIGN_GEOMETRIC_PRESENTATION_REPRESENTATION (  '', ( #30481 ), #3830 ) ;
#29224 = CARTESIAN_POINT ( 'NONE',  ( -69.00000000000002842, 214.0000000000000000, -2.499999999999998668 ) ) ;
#29225 = CARTESIAN_POINT ( 'NONE',  ( 3.474262827703335166, 28.23518628210144854, 8.843639120294326972 ) ) ;
#29226 = CARTESIAN_POINT ( 'NONE',  ( 27.24356964374999635, 196.9718750006145456, -15.72908226750539029 ) ) ;
#29227 = CARTESIAN_POINT ( 'NONE',  ( 26.99999999999999645, 195.8750000012290400, -15.58845726811990495 ) ) ;
#29228 = VECTOR ( 'NONE', #13580, 1000.000000000000000 ) ;
#29229 = CARTESIAN_POINT ( 'NONE',  ( 20.99999999999999645, 192.3000000000000398, 8.000000000000000000 ) ) ;
#29230 = CARTESIAN_POINT ( 'NONE',  ( 28.23805287048444512, 5.196152422706630247, 167.1524626168076111 ) ) ;
#29231 = CARTESIAN_POINT ( 'NONE',  ( 25.33444562538816669, 0.000000000000000000, 168.3852196756899957 ) ) ;
#29232 = CARTESIAN_POINT ( 'NONE',  ( 15.24356964374999990, 244.8718750006145513, -3.323476615752268604 ) ) ;
#29233 = CARTESIAN_POINT ( 'NONE',  ( -6.594114490232462877, 88.13981371789856212, 6.840914352311949109 ) ) ;
#29234 = PLANE ( 'NONE',  #14314 ) ;
#29235 = ORIENTED_EDGE ( 'NONE', *, *, #10261, .F. ) ;
#29236 = CARTESIAN_POINT ( 'NONE',  ( -53.17038769728823411, 208.1428034533959703, 6.469044688360770401 ) ) ;
#29237 = CARTESIAN_POINT ( 'NONE',  ( 26.99999999999999645, 246.2687500012290513, -3.464101615137755275 ) ) ;
#29238 = CARTESIAN_POINT ( 'NONE',  ( 12.46528703574811558, 93.60231371789856780, -2.660918448318005947 ) ) ;
#29239 = CARTESIAN_POINT ( 'NONE',  ( 22.80587116629411426, 3.604726614523243278, -2.634374999385520777 ) ) ;
#29240 = CARTESIAN_POINT ( 'NONE',  ( 28.41594069642870579, 5.957546110389989380, 159.6438081731886314 ) ) ;
#29241 = CARTESIAN_POINT ( 'NONE',  ( 18.12178482187500350, -4.985214923628407568, -2.428124999385494753 ) ) ;
#29242 = CARTESIAN_POINT ( 'NONE',  ( 12.53471296425189330, 66.57731371789856212, 2.311890736173451977 ) ) ;
#29243 = CARTESIAN_POINT ( 'NONE',  ( -27.24356964374999990, 198.0218750006145569, -15.72908226750537786 ) ) ;
#29244 = ADVANCED_FACE ( 'NONE', ( #8570 ), #17294, .T. ) ;
#29245 = ORIENTED_EDGE ( 'NONE', *, *, #36523, .F. ) ;
#29246 = EDGE_LOOP ( 'NONE', ( #29957, #23925, #23206, #29584, #24758, #3944, #14902, #35657 ) ) ;
#29247 = CARTESIAN_POINT ( 'NONE',  ( 26.75643035624999655, 7.049594010296217766E-16, -6.215624999385465976 ) ) ;
#29248 = CYLINDRICAL_SURFACE ( 'NONE', #23954, 2.649999999999991029 ) ;
#29249 = CARTESIAN_POINT ( 'NONE',  ( 15.24356964374999990, 246.5593750006144944, -3.323476615752268604 ) ) ;
#29250 = CARTESIAN_POINT ( 'NONE',  ( -2.660918448318275509, 47.49768628210144783, 12.46528703574805874 ) ) ;
#29251 = CARTESIAN_POINT ( 'NONE',  ( -46.63169563604516554, 210.1155267958017703, 6.500000000000000888 ) ) ;
#29252 = CARTESIAN_POINT ( 'NONE',  ( -65.82961230271179431, 211.8571965466040297, 6.469044688360755302 ) ) ;
#29253 =( NAMED_UNIT ( * ) SI_UNIT ( $, .STERADIAN. ) SOLID_ANGLE_UNIT ( ) );
#29254 = CARTESIAN_POINT ( 'NONE',  ( 30.73311757145110690, -6.928203230275506996, 161.2500429106201523 ) ) ;
#29255 = CARTESIAN_POINT ( 'NONE',  ( 10.49813415416005213, 102.2273137178985536, -7.228626920338837358 ) ) ;
#29256 = CARTESIAN_POINT ( 'NONE',  ( -63.06622103062156270, 211.0902445701382533, 4.530955311639240257 ) ) ;
#29257 = VECTOR ( 'NONE', #13362, 1000.000000000000000 ) ;
#29258 = CARTESIAN_POINT ( 'NONE',  ( -64.45163769728823411, 215.6869285224996986, -3.149950860017881382 ) ) ;
#29259 = EDGE_CURVE ( 'NONE', #9546, #11516, #31139, .T. ) ;
#29260 = CARTESIAN_POINT ( 'NONE',  ( 26.75643035624999655, 7.049594010296217766E-16, -4.528124999385485516 ) ) ;
#29261 = CARTESIAN_POINT ( 'NONE',  ( -27.24356964375001056, 194.8294844423495533, -9.915847621322177119 ) ) ;
#29262 = CARTESIAN_POINT ( 'NONE',  ( -6.092822981423666739, 72.61481371789855643, -14.25334919248795096 ) ) ;
#29263 = CARTESIAN_POINT ( 'NONE',  ( -63.65252896937850124, 205.6499508600178103, -7.303452534266820173 ) ) ;
#29264 = EDGE_LOOP ( 'NONE', ( #23254, #32180, #4766, #22071 ) ) ;
#29265 = CARTESIAN_POINT ( 'NONE',  ( 27.85892538953216757, -5.196152422706632912, 162.8190156801084925 ) ) ;
#29266 = CARTESIAN_POINT ( 'NONE',  ( 11.61527771782819940, 99.53518628210144925, -4.622313124798573369 ) ) ;
#29267 = CARTESIAN_POINT ( 'NONE',  ( 8.927990412390657937, 43.47268628210144215, -13.04141134922759804 ) ) ;
#29268 = EDGE_CURVE ( 'NONE', #17429, #8055, #10731, .T. ) ;
#29269 = FACE_OUTER_BOUND ( 'NONE', #14816, .T. ) ;
#29270 = CARTESIAN_POINT ( 'NONE',  ( 28.41103595111929536, 5.957544813848101306, 159.5877724440177303 ) ) ;
#29271 = CARTESIAN_POINT ( 'NONE',  ( -8.927990412390661490, 66.47268628210146346, 13.04141134922759804 ) ) ;
#29272 = CARTESIAN_POINT ( 'NONE',  ( -13.62178482187498396, 198.9781250006145399, 23.59362340125808188 ) ) ;
#29273 = CARTESIAN_POINT ( 'NONE',  ( 19.68408634441910721, -5.407089921784855591, -8.540624999385542537 ) ) ;
#29274 = CARTESIAN_POINT ( 'NONE',  ( 24.00000000000000000, -5.196152422706629359, -1.143749998770954290 ) ) ;
#29275 = CARTESIAN_POINT ( 'NONE',  ( -52.57663769728823411, 204.3130714775002730, 3.149950860017883603 ) ) ;
#29276 = CARTESIAN_POINT ( 'NONE',  ( 37.34107544803033107, 3.464101615137920032, 167.9370675803488950 ) ) ;
#29277 = CARTESIAN_POINT ( 'NONE',  ( 12.53471296425194836, 35.42268628210144499, -2.311890736173178418 ) ) ;
#29278 = CARTESIAN_POINT ( 'NONE',  ( 27.00000000000001066, 196.1375000000000171, 15.58845726811988897 ) ) ;
#29279 = CARTESIAN_POINT ( 'NONE',  ( 15.00000000000000000, 0.000000000000000000, -7.593749998770965348 ) ) ;
#29280 = CARTESIAN_POINT ( 'NONE',  ( 9.465287035748067623, 8.397686282101439303, 2.064181346179272847 ) ) ;
#29281 = CARTESIAN_POINT ( 'NONE',  ( 15.24356964374999990, 245.7718750006145001, -3.323476615752268604 ) ) ;
#29282 = CIRCLE ( 'NONE', #1450, 3.500000000000002665 ) ;
#29283 = ORIENTED_EDGE ( 'NONE', *, *, #25320, .T. ) ;
#29284 = CARTESIAN_POINT ( 'NONE',  ( 15.00000000000000000, 0.000000000000000000, -6.299999999999999822 ) ) ;
#29285 = FACE_OUTER_BOUND ( 'NONE', #21834, .T. ) ;
#29286 = DIRECTION ( 'NONE',  ( 0.000000000000000000, 0.000000000000000000, 1.000000000000000000 ) ) ;
#29287 = CARTESIAN_POINT ( 'NONE',  ( 19.68408634441911076, 5.407089921784857367, -4.790624999385539873 ) ) ;
#29288 = CARTESIAN_POINT ( 'NONE',  ( 34.30794447475221176, 5.407089921784857367, 166.2920375277922460 ) ) ;
#29289 = CARTESIAN_POINT ( 'NONE',  ( 18.91622499444735084, 240.0135471875693725, -5.725135169889072451 ) ) ;
#29290 = CARTESIAN_POINT ( 'NONE',  ( 36.60243052835136268, 7.347880794884117764E-16, 159.4943175152456831 ) ) ;
#29291 = AXIS2_PLACEMENT_3D ( 'NONE', #14095, #13914, #1782 ) ;
#29292 = CARTESIAN_POINT ( 'NONE',  ( 8.715434833791931624, 73.66018628210144925, 8.962234695871760692 ) ) ;
#29293 = ORIENTED_EDGE ( 'NONE', *, *, #10802, .T. ) ;
#29294 = ORIENTED_EDGE ( 'NONE', *, *, #547, .T. ) ;
#29295 = CARTESIAN_POINT ( 'NONE',  ( 27.60072650153512441, 5.196152422706636465, 159.8677888857873768 ) ) ;
#29296 = CYLINDRICAL_SURFACE ( 'NONE', #4572, 3.999999999999996447 ) ;
#29297 = CARTESIAN_POINT ( 'NONE',  ( 26.99999999999999645, 195.3125000000000000, -15.58845726811990495 ) ) ;
#29298 = CARTESIAN_POINT ( 'NONE',  ( 26.75643035624999655, 3.323476615752271712, -6.178124999385475213 ) ) ;
#29299 = CARTESIAN_POINT ( 'NONE',  ( 12.53471296425194836, 99.82268628210144357, -2.311890736173178418 ) ) ;
#29300 = CARTESIAN_POINT ( 'NONE',  ( 15.50000000000000533, 29.48981371789855288, -0.1745138560722452326 ) ) ;
#29301 = CARTESIAN_POINT ( 'NONE',  ( -77.35272773637332477, 226.7246823105297153, 5.000000000000000000 ) ) ;
#29302 = CARTESIAN_POINT ( 'NONE',  ( 18.12178482187500350, 240.0343750006145171, 4.985214923628407568 ) ) ;
#29303 = CARTESIAN_POINT ( 'NONE',  ( -62.66294563604517265, 213.2096571498974527, -3.378800118222469617 ) ) ;
#29304 = LINE ( 'NONE', #14912, #36128 ) ;
#29305 = CARTESIAN_POINT ( 'NONE',  ( 31.41946904558886544, 6.928203230275506996, 169.0950761580926383 ) ) ;
#29306 = CARTESIAN_POINT ( 'NONE',  ( -8.710071997420207879, 15.11481371789854933, 3.796722387233182339 ) ) ;
#29307 = EDGE_CURVE ( 'NONE', #6128, #17802, #18497, .T. ) ;
#29308 = CARTESIAN_POINT ( 'NONE',  ( -64.64955436395490551, 214.8429017333601792, -4.673758765035196383 ) ) ;
#29309 = CARTESIAN_POINT ( 'NONE',  ( -31.78794563604516910, 203.8621396198271043, 6.307003348498029460 ) ) ;
#29310 = CARTESIAN_POINT ( 'NONE',  ( -50.00000000000000000, 0.000000000000000000, 5.000000000000000000 ) ) ;
#29311 = CARTESIAN_POINT ( 'NONE',  ( 13.56230152254410548, 5.196152422706630247, -4.462499998771018994 ) ) ;
#29312 = CARTESIAN_POINT ( 'NONE',  ( -27.24356964375000345, 195.3593750006145342, 0.000000000000000000 ) ) ;
#29313 = CARTESIAN_POINT ( 'NONE',  ( 10.83675517735179206, 138.7398137178985564, -11.08355503943118769 ) ) ;
#29314 = CARTESIAN_POINT ( 'NONE',  ( -52.56919563604516554, 216.5000000000000000, -0.1155267958017906493 ) ) ;
#29315 = ADVANCED_FACE ( 'NONE', ( #31684 ), #28650, .T. ) ;
#29316 = ORIENTED_EDGE ( 'NONE', *, *, #34329, .F. ) ;
#29317 = CARTESIAN_POINT ( 'NONE',  ( 2.311890736173175753, 46.92268628210145209, 12.53471296425194836 ) ) ;
#29318 = CARTESIAN_POINT ( 'NONE',  ( -5.327872176777560753, 223.7027713702217113, -2.499999999999999112 ) ) ;
#29319 = CARTESIAN_POINT ( 'NONE',  ( 18.00000000000000000, 247.2249999999999943, -5.196152422706630247 ) ) ;
#29320 = CARTESIAN_POINT ( 'NONE',  ( 24.98313052087628350, 3.604726614523240613, 167.1643179041065252 ) ) ;
#29321 = CARTESIAN_POINT ( 'NONE',  ( 15.00000000000000000, 0.000000000000000000, -3.093749998770961795 ) ) ;
#29322 = VERTEX_POINT ( 'NONE', #31501 ) ;
#29323 = CARTESIAN_POINT ( 'NONE',  ( -63.06622103062156981, 211.6261429550005744, 6.530955311639228711 ) ) ;
#29324 = CARTESIAN_POINT ( 'NONE',  ( 10.31873187879410914, 0.000000000000000000, -1.040624999385536542 ) ) ;
#29325 = CARTESIAN_POINT ( 'NONE',  ( 8.152565276336714462, 53.24768628210144783, -5.233372021372432847 ) ) ;
#29326 = CARTESIAN_POINT ( 'NONE',  ( 2.999999999999997335, 252.0000000000000000, -5.000000000000000000 ) ) ;
#29327 = CARTESIAN_POINT ( 'NONE',  ( -44.35000000000001563, 244.5000000000000000, 5.000000000000000000 ) ) ;
#29328 = EDGE_CURVE ( 'NONE', #25480, #24534, #14075, .T. ) ;
#29329 = CARTESIAN_POINT ( 'NONE',  ( -12.50000000000000355, 95.51018628210144357, -0.1745138560725492671 ) ) ;
#29330 = FACE_OUTER_BOUND ( 'NONE', #6941, .T. ) ;
#29331 = CARTESIAN_POINT ( 'NONE',  ( -27.00000000000000355, 195.1625000012290343, 0.000000000000000000 ) ) ;
#29332 = VERTEX_POINT ( 'NONE', #19959 ) ;
#29333 = CARTESIAN_POINT ( 'NONE',  ( 22.60769515458672529, 244.9736538117967370, -6.000000000000004441 ) ) ;
#29334 = CARTESIAN_POINT ( 'NONE',  ( 24.00000000000000000, -5.196152422706629359, -0.2999999999999947153 ) ) ;
#29335 = CARTESIAN_POINT ( 'NONE',  ( 0.000000000000000000, 150.0000000000000000, 0.000000000000000000 ) ) ;
#29336 = CARTESIAN_POINT ( 'NONE',  ( 31.13757469008587719, -7.209453229046482114, 165.8730089308399442 ) ) ;
#29337 = CARTESIAN_POINT ( 'NONE',  ( 36.90311784072365242, -3.464101615137755275, 162.9311892224378369 ) ) ;
#29338 = CARTESIAN_POINT ( 'NONE',  ( 13.49999999999999645, 196.7000000000000171, -23.38268590217984766 ) ) ;
#29339 = CARTESIAN_POINT ( 'NONE',  ( 15.00000000000000178, 249.1374999999999886, 3.464101615137757051 ) ) ;
#29340 = CARTESIAN_POINT ( 'NONE',  ( 27.24356964375000700, 196.8406250006145228, 15.72908226750537075 ) ) ;
#29341 = CARTESIAN_POINT ( 'NONE',  ( 10.49813415416005213, 111.4273137178985564, -7.228626920338837358 ) ) ;
#29342 = CARTESIAN_POINT ( 'NONE',  ( -8.715434833791929847, 115.0601862821014549, -8.962234695871762469 ) ) ;
#29344 = ORIENTED_EDGE ( 'NONE', *, *, #8449, .T. ) ;
#29343 = EDGE_LOOP ( 'NONE', ( #1800, #13283, #3382, #15681 ) ) ;
#29345 = CARTESIAN_POINT ( 'NONE',  ( 5.778771075727756162E-15, 194.9656250006145228, 31.45816453501075927 ) ) ;
#29346 = CARTESIAN_POINT ( 'NONE',  ( 23.87821517812500005, 240.4468750006145115, 4.985214923628404016 ) ) ;
#29347 = EDGE_CURVE ( 'NONE', #19776, #19019, #2131, .T. ) ;
#29348 = CARTESIAN_POINT ( 'NONE',  ( -15.53471296425188442, 98.77731371789855075, -2.908627838312459080 ) ) ;
#29349 = CARTESIAN_POINT ( 'NONE',  ( 26.75643035624999655, 3.323476615752271712, -4.490624999385484095 ) ) ;
#29350 = CARTESIAN_POINT ( 'NONE',  ( 23.87821517812500005, 248.6593750006145171, 4.985214923628404016 ) ) ;
#29351 = CARTESIAN_POINT ( 'NONE',  ( -1.715153634034234598, 106.7226862821014635, -9.534712964251941258 ) ) ;
#29352 = CARTESIAN_POINT ( 'NONE',  ( 26.99999999999999645, 196.3250000012290570, -15.58845726811990495 ) ) ;
#29353 = CARTESIAN_POINT ( 'NONE',  ( 9.534712964251900402, 84.97731371789856780, 1.715153634034445540 ) ) ;
#29354 = CARTESIAN_POINT ( 'NONE',  ( 16.56230152254411081, 7.209453229046475009, -6.553124999385508964 ) ) ;
#29355 = CARTESIAN_POINT ( 'NONE',  ( 18.12178482187500350, 241.7218750006145171, 4.985214923628407568 ) ) ;
#29356 = CARTESIAN_POINT ( 'NONE',  ( -0.1745138560722763466, 54.78981371789855359, -12.50000000000000355 ) ) ;
#29357 =( BOUNDED_CURVE ( )  B_SPLINE_CURVE ( 2, ( #26613, #457, #31930, #17724, #6343 ),
 .UNSPECIFIED., .F., .F. ) 
 B_SPLINE_CURVE_WITH_KNOTS ( ( 3, 2, 3 ),
 ( 0.9565217391304342565, 0.9637681159420288246, 0.9662082966761268432 ),
 .UNSPECIFIED. ) 
 CURVE ( )  GEOMETRIC_REPRESENTATION_ITEM ( )  RATIONAL_B_SPLINE_CURVE ( ( 1.000000000000010214, 0.8660254037844284936, 1.000000000000000000, 0.9548847324609615050, 0.9401541411607547971 ) ) 
 REPRESENTATION_ITEM ( '' )  );
#29358 = CARTESIAN_POINT ( 'NONE',  ( 24.90302469878729141, 0.000000000000000000, 163.4540559201358576 ) ) ;
#29359 = CARTESIAN_POINT ( 'NONE',  ( -10.69584247140444866, 103.8476862821014493, 6.932735513423972762 ) ) ;
#29360 = CARTESIAN_POINT ( 'NONE',  ( 22.56230152254410370, 7.347880794884117764E-16, -5.962499998771020771 ) ) ;
#29361 = CARTESIAN_POINT ( 'NONE',  ( -32.19122103062156981, 208.3738570449993404, -6.530955311639226935 ) ) ;
#29362 = CARTESIAN_POINT ( 'NONE',  ( 15.00000000000000000, 0.000000000000000000, -7.143749998770959841 ) ) ;
#29363 = FACE_OUTER_BOUND ( 'NONE', #35497, .T. ) ;
#29364 = CARTESIAN_POINT ( 'NONE',  ( -13.04141134922759804, 77.97268628210142083, -8.927990412390657937 ) ) ;
#29365 = SURFACE_STYLE_USAGE ( .BOTH. , #21051 ) ;
#29366 = CARTESIAN_POINT ( 'NONE',  ( -77.00000000000002842, 206.0000000000000000, -2.499999999999998668 ) ) ;
#29367 = CARTESIAN_POINT ( 'NONE',  ( 13.50000000000001421, 198.3499999999999943, 23.38268590217984055 ) ) ;
#29368 = CARTESIAN_POINT ( 'NONE',  ( 2.064181346179272847, 116.4976862821014549, -9.465287035748065847 ) ) ;
#29369 = CARTESIAN_POINT ( 'NONE',  ( 7.234628195640318005, 199.0799038117967541, -26.99999999999999645 ) ) ;
#29370 = VECTOR ( 'NONE', #22881, 1000.000000000000000 ) ;
#29371 = CARTESIAN_POINT ( 'NONE',  ( -6.092822981423970496, 20.18518628210144783, 14.25334919248782661 ) ) ;
#29372 = CARTESIAN_POINT ( 'NONE',  ( -27.24356964375000345, 196.7093750006145569, 0.000000000000000000 ) ) ;
#29373 = CARTESIAN_POINT ( 'NONE',  ( 15.24356964375000167, 242.1343750006145399, 3.323476615752272600 ) ) ;
#29374 = ORIENTED_EDGE ( 'NONE', *, *, #36354, .T. ) ;
#29375 = CARTESIAN_POINT ( 'NONE',  ( 31.16208724273364439, 7.209453229046475009, 166.1531886896782737 ) ) ;
#29376 = CARTESIAN_POINT ( 'NONE',  ( 23.87821517812499650, 4.985214923628404904, -1.640624999385470462 ) ) ;
#29378 = ADVANCED_FACE ( 'NONE', ( #13709 ), #31318, .F. ) ;
#29377 = CYLINDRICAL_SURFACE ( 'NONE', #34395, 27.00000000000000000 ) ;
#29379 = CARTESIAN_POINT ( 'NONE',  ( 23.99999999999999645, 5.196152422706631135, -3.750000000000003553 ) ) ;
#29380 = CARTESIAN_POINT ( 'NONE',  ( 15.02283181144952628, 7.347880794884122694E-16, 50.52293445648592751 ) ) ;
#29381 = EDGE_CURVE ( 'NONE', #36867, #22329, #22370, .T. ) ;
#29382 = CARTESIAN_POINT ( 'NONE',  ( 25.14161354455920261, -3.464101615137879620, 166.1811389061619764 ) ) ;
#29383 = CARTESIAN_POINT ( 'NONE',  ( 13.50000000000001421, 198.3499999999999943, 23.38268590217984055 ) ) ;
#29384 = CARTESIAN_POINT ( 'NONE',  ( 9.465287035748106703, 29.20231371789855501, -2.064181346179063237 ) ) ;
#29385 = CARTESIAN_POINT ( 'NONE',  ( 5.778771075727756162E-15, 199.0718750006145399, 31.45816453501076637 ) ) ;
#29386 = ORIENTED_EDGE ( 'NONE', *, *, #17949, .T. ) ;
#29387 = CARTESIAN_POINT ( 'NONE',  ( 15.24356964374999990, 249.7468750006145228, 0.000000000000000000 ) ) ;
#29388 = CARTESIAN_POINT ( 'NONE',  ( -2.311890736173447980, 50.47731371789855359, 12.53471296425189330 ) ) ;
#29389 = EDGE_CURVE ( 'NONE', #12997, #29586, #26217, .T. ) ;
#29390 = CARTESIAN_POINT ( 'NONE',  ( 23.87821517812500005, -4.985214923628404016, -8.653124999385475746 ) ) ;
#29391 = CARTESIAN_POINT ( 'NONE',  ( -2.660918448318004614, 8.502313717898557499, -12.46528703574811558 ) ) ;
#29392 = ADVANCED_FACE ( 'NONE', ( #14262 ), #25261, .F. ) ;
#29393 = DIRECTION ( 'NONE',  ( 0.000000000000000000, 0.000000000000000000, 1.000000000000000000 ) ) ;
#29394 = ORIENTED_EDGE ( 'NONE', *, *, #34206, .T. ) ;
#29395 = CARTESIAN_POINT ( 'NONE',  ( 22.80587116629412137, 7.646167579472024665E-16, -4.021874999385527616 ) ) ;
#29396 = AXIS2_PLACEMENT_3D ( 'NONE', #26077, #8464, #34427 ) ;
#29397 = ORIENTED_EDGE ( 'NONE', *, *, #25579, .T. ) ;
#29398 = CARTESIAN_POINT ( 'NONE',  ( -27.24356964374999635, 198.0406250006145399, 15.72908226750539384 ) ) ;
#29399 = CARTESIAN_POINT ( 'NONE',  ( 30.88264414254898682, 7.209453229046482114, 162.9591394389216532 ) ) ;
#29400 = AXIS2_PLACEMENT_3D ( 'NONE', #24274, #27111, #26348 ) ;
#29401 = APPLICATION_CONTEXT ( 'automotive_design' ) ;
#29402 = CARTESIAN_POINT ( 'NONE',  ( -30.60044563604515488, 205.1570982666397072, -4.673758765035155527 ) ) ;
#29403 = CARTESIAN_POINT ( 'NONE',  ( 18.12178482187500350, 248.9218750006145342, 4.985214923628407568 ) ) ;
#29404 = SURFACE_STYLE_USAGE ( .BOTH. , #26745 ) ;
#29405 = CARTESIAN_POINT ( 'NONE',  ( 17.00000000000000000, 4.898587196589404940E-16, -8.000000000000000000 ) ) ;
#29406 = CARTESIAN_POINT ( 'NONE',  ( -63.45461230271184405, 208.6787018382582346, -4.469044688360757966 ) ) ;
#29407 =( BOUNDED_CURVE ( )  B_SPLINE_CURVE ( 2, ( #8969, #3085, #26022, #23192, #26205, #34740, #242 ),
 .UNSPECIFIED., .F., .F. ) 
 B_SPLINE_CURVE_WITH_KNOTS ( ( 3, 2, 2, 3 ),
 ( 0.7173913043478246099, 0.7246376811594190670, 0.7318840579710134131, 0.7391304347826077592 ),
 .UNSPECIFIED. ) 
 CURVE ( )  GEOMETRIC_REPRESENTATION_ITEM ( )  RATIONAL_B_SPLINE_CURVE ( ( 1.000000000000026645, 0.8660254037844120623, 1.000000000000000000, 0.8660254037844387076, 1.000000000000000000, 0.8660254037844551389, 0.9999999999999835687 ) ) 
 REPRESENTATION_ITEM ( '' )  );
#29408 = CARTESIAN_POINT ( 'NONE',  ( -36.94122103062157692, 208.3738570449993404, -6.530955311639226935 ) ) ;
#29409 = CARTESIAN_POINT ( 'NONE',  ( 37.32960477335537774, -3.604726614523235284, 165.0113089211254760 ) ) ;
#29410 = VERTEX_POINT ( 'NONE', #37359 ) ;
#29411 = CARTESIAN_POINT ( 'NONE',  ( -27.90475745684348752, 208.6802886524470750, 7.894770873222196172 ) ) ;
#29412 = CARTESIAN_POINT ( 'NONE',  ( -15.50000000000000533, 6.489813717898557321, 0.1745138560722471477 ) ) ;
#29413 = CARTESIAN_POINT ( 'NONE',  ( -54.35788769728822700, 218.4690446883607535, 2.393094931466250408 ) ) ;
#29414 = CARTESIAN_POINT ( 'NONE',  ( 9.465287035748067623, 127.9976862821014265, 2.064181346179272847 ) ) ;
#29415 = CARTESIAN_POINT ( 'NONE',  ( -4.944772684328673229, 38.58518628210144641, 11.48171059495397728 ) ) ;
#29416 = CARTESIAN_POINT ( 'NONE',  ( 10.56230152254410903, 3.464101615137757051, -8.137500000000047251 ) ) ;
#29417 = VERTEX_POINT ( 'NONE', #7323 ) ;
#29418 = CARTESIAN_POINT ( 'NONE',  ( -48.81622103062156981, 211.6261429550005744, 6.530955311639228711 ) ) ;
#29419 = CARTESIAN_POINT ( 'NONE',  ( -11.08355503943142573, 131.1601862821014777, 10.83675517735155402 ) ) ;
#29420 = CARTESIAN_POINT ( 'NONE',  ( -26.99999999999999645, 198.8000000012290513, 15.58845726811991561 ) ) ;
#29421 = CARTESIAN_POINT ( 'NONE',  ( 3.796722387233379514, 6.385186282101440902, -8.710071997420127943 ) ) ;
#29422 = CARTESIAN_POINT ( 'NONE',  ( 27.24356964374999635, 195.1718750006145342, -15.72908226750539029 ) ) ;
#29423 = LINE ( 'NONE', #17879, #6536 ) ;
#29424 = DIRECTION ( 'NONE',  ( -0.8083506638593008775, -0.5887012860850803220, 0.000000000000000000 ) ) ;
#29425 = CARTESIAN_POINT ( 'NONE',  ( 33.80667851479820030, 5.196152422706637353, 161.9598655117922874 ) ) ;
#29426 =( BOUNDED_CURVE ( )  B_SPLINE_CURVE ( 2, ( #13847, #19543, #31091, #25395, #27682, #28415, #36945 ),
 .UNSPECIFIED., .F., .F. ) 
 B_SPLINE_CURVE_WITH_KNOTS ( ( 3, 2, 2, 3 ),
 ( 0.9347826086956513292, 0.9420289855072455643, 0.9492753623188399104, 0.9565217391304342565 ),
 .UNSPECIFIED. ) 
 CURVE ( )  GEOMETRIC_REPRESENTATION_ITEM ( )  RATIONAL_B_SPLINE_CURVE ( ( 1.000000000000016431, 0.8660254037844222763, 1.000000000000000000, 0.8660254037844387076, 1.000000000000000000, 0.8660254037844489217, 0.9999999999999897859 ) ) 
 REPRESENTATION_ITEM ( '' )  );
#29427 = CARTESIAN_POINT ( 'NONE',  ( 23.87821517812499650, 243.8593750006145342, -4.985214923628404904 ) ) ;
#29428 = CARTESIAN_POINT ( 'NONE',  ( 7.954856959092311719, 93.02731371789853654, -5.529263428287300108 ) ) ;
#29429 = DIRECTION ( 'NONE',  ( -0.9925324990730154395, 0.1219804832088915297, 0.000000000000000000 ) ) ;
#29430 = ORIENTED_EDGE ( 'NONE', *, *, #33045, .T. ) ;
#29431 = CARTESIAN_POINT ( 'NONE',  ( -60.29538769728823411, 211.8571965466039444, -6.469044688360768625 ) ) ;
#29432 = CARTESIAN_POINT ( 'NONE',  ( 18.00000000000000355, 246.9812500012290570, 5.196152422706632912 ) ) ;
#29433 = CARTESIAN_POINT ( 'NONE',  ( 4.622313124798831829, 92.16481371789855359, -11.61527771782809282 ) ) ;
#29434 = CARTESIAN_POINT ( 'NONE',  ( 19.68408634441912142, -5.407089921784861808, -1.846874999385544891 ) ) ;
#29435 = CARTESIAN_POINT ( 'NONE',  ( 36.85896376251805151, -3.604726614523235284, 159.6318575514300449 ) ) ;
#29436 = CARTESIAN_POINT ( 'NONE',  ( 26.75643035624999655, 7.049594010296217766E-16, -1.828124999385477567 ) ) ;
#29437 = CARTESIAN_POINT ( 'NONE',  ( -4.622313124798826500, 59.96481371789855075, 11.61527771782809637 ) ) ;
#29438 = CARTESIAN_POINT ( 'NONE',  ( -13.62178482187498396, 197.6843750006145228, 23.59362340125808188 ) ) ;
#29439 = ORIENTED_EDGE ( 'NONE', *, *, #21502, .T. ) ;
#29440 = EDGE_LOOP ( 'NONE', ( #14667, #29474, #37286, #13230 ) ) ;
#29441 = CARTESIAN_POINT ( 'NONE',  ( 18.12178482187499640, 4.985214923628404904, -4.265624999385458693 ) ) ;
#29442 = CARTESIAN_POINT ( 'NONE',  ( -47.00000000000000711, 252.0000000000000000, 5.000000000000000000 ) ) ;
#29443 = CARTESIAN_POINT ( 'NONE',  ( 21.00000000000000000, 246.4843750006145058, -6.646953231504538984 ) ) ;
#29444 = AXIS2_PLACEMENT_3D ( 'NONE', #35091, #12161, #20899 ) ;
#29445 = CARTESIAN_POINT ( 'NONE',  ( 12.50000000000000355, 35.71018628210144641, 0.1745138560725507937 ) ) ;
#29446 = CARTESIAN_POINT ( 'NONE',  ( -50.78794563604516554, 205.3262412349648116, 4.842901733360249317 ) ) ;
#29447 = CARTESIAN_POINT ( 'NONE',  ( 15.80103094669413366, 223.8639174754800365, -3.001545256183639321 ) ) ;
#29448 = CARTESIAN_POINT ( 'NONE',  ( -30.20461230271183339, 208.6787018382582346, -4.469044688360757966 ) ) ;
#29449 = CARTESIAN_POINT ( 'NONE',  ( 27.85892538953216757, -5.196152422706632912, 162.8190156801084925 ) ) ;
#29450 = CARTESIAN_POINT ( 'NONE',  ( 6.932735513424201024, 83.25231371789857349, -10.69584247140429412 ) ) ;
#29451 = CARTESIAN_POINT ( 'NONE',  ( -62.07663769728824121, 206.0451222850691408, 2.149950860017832532 ) ) ;
#29452 = CARTESIAN_POINT ( 'NONE',  ( -64.25372103062154849, 216.5309553116391612, -1.626142955000564383 ) ) ;
#29453 = CARTESIAN_POINT ( 'NONE',  ( 18.12178482187500350, -4.985214923628407568, -7.828124999385482674 ) ) ;
#29454 = CARTESIAN_POINT ( 'NONE',  ( 10.56230152254347487, 3.464101615137389345, -7.237500000000049560 ) ) ;
#29455 = CARTESIAN_POINT ( 'NONE',  ( 0.1745138560722461762, 68.58981371789855075, 15.50000000000000533 ) ) ;
#29456 = CARTESIAN_POINT ( 'NONE',  ( -57.31919563604516554, 218.5000000000000000, -0.1155267958018185298 ) ) ;
#29457 = ORIENTED_EDGE ( 'NONE', *, *, #35891, .F. ) ;
#29458 = CARTESIAN_POINT ( 'NONE',  ( 24.86707295490436209, -3.464101615138032830, 163.0431256071729820 ) ) ;
#29459 = CARTESIAN_POINT ( 'NONE',  ( 4.944772684328679446, 79.98518628210145209, -11.48171059495397373 ) ) ;
#29460 = CARTESIAN_POINT ( 'NONE',  ( 15.46528703574804986, 45.19768628210142225, 3.257655550457285720 ) ) ;
#29461 = CARTESIAN_POINT ( 'NONE',  ( 20.99999999999999645, 0.000000000000000000, -8.000000000000000000 ) ) ;
#29462 = CARTESIAN_POINT ( 'NONE',  ( 24.47980610650859390, -3.604726614523244610, 161.4112935226266359 ) ) ;
#29463 = CARTESIAN_POINT ( 'NONE',  ( -8.632099005475501130, 50.94768628210145067, -13.23911966647218996 ) ) ;
#29464 = VECTOR ( 'NONE', #12444, 1000.000000000000000 ) ;
#29465 = CARTESIAN_POINT ( 'NONE',  ( -13.62178482187498396, 199.4281250006145569, 23.59362340125808188 ) ) ;
#29466 = CARTESIAN_POINT ( 'NONE',  ( 22.80587116629411426, -3.604726614523235284, -8.053124999385516958 ) ) ;
#29467 = CARTESIAN_POINT ( 'NONE',  ( -70.65404437008254490, 216.5466800865261234, -7.500000000000000000 ) ) ;
#29468 = CARTESIAN_POINT ( 'NONE',  ( -50.79538769728821990, 211.8571965466039444, -6.469044688360768625 ) ) ;
#29469 = CARTESIAN_POINT ( 'NONE',  ( 22.60769515458671108, 241.1888461906613657, 6.000000000000010658 ) ) ;
#29470 = CARTESIAN_POINT ( 'NONE',  ( -8.715434833791929847, 32.26018628210145067, -8.962234695871762469 ) ) ;
#29471 = CARTESIAN_POINT ( 'NONE',  ( 34.05180404138307182, 5.196152422706631135, 164.7616631013996766 ) ) ;
#29472 = CARTESIAN_POINT ( 'NONE',  ( -5.233372021372612259, 143.0523137178985280, 8.152565276336593669 ) ) ;
#29473 = CARTESIAN_POINT ( 'NONE',  ( 15.24356964374999990, 245.8093750006145228, 0.000000000000000000 ) ) ;
#29474 = ORIENTED_EDGE ( 'NONE', *, *, #8947, .T. ) ;
#29475 = CARTESIAN_POINT ( 'NONE',  ( 24.00000000000000000, -5.196152422706629359, -6.599999999999994316 ) ) ;
#29476 = CARTESIAN_POINT ( 'NONE',  ( 15.00000000000000000, 245.0687500012290343, -3.464101615137752610 ) ) ;
#29477 = CARTESIAN_POINT ( 'NONE',  ( 10.49999999999999822, 210.0000000000000284, -2.500000000000000000 ) ) ;
#29478 = CARTESIAN_POINT ( 'NONE',  ( 22.80587116629410716, 3.604726614523238837, -5.278124999385515714 ) ) ;
#29479 = CARTESIAN_POINT ( 'NONE',  ( 28.10774354060011504, -5.407089921784859143, 167.0603442845606139 ) ) ;
#29480 = CARTESIAN_POINT ( 'NONE',  ( 18.00000000000000000, 240.4749999999999943, -5.196152422706630247 ) ) ;
#29481 = CARTESIAN_POINT ( 'NONE',  ( 20.99999999999999645, 185.0294372515228645, 5.999999999999999112 ) ) ;
#29482 = CARTESIAN_POINT ( 'NONE',  ( -4.622313124798576922, 42.03518628210144215, -11.61527771782819762 ) ) ;
#29483 = ORIENTED_EDGE ( 'NONE', *, *, #1751, .F. ) ;
#29484 = ORIENTED_EDGE ( 'NONE', *, *, #9132, .T. ) ;
#29485 = CARTESIAN_POINT ( 'NONE',  ( 24.61541074761229098, 3.464101615137389345, 160.1666134152088148 ) ) ;
#29486 = B_SPLINE_CURVE_WITH_KNOTS ( 'NONE', 1,
 ( #31296, #32031 ),
 .UNSPECIFIED., .F., .F.,
 ( 2, 2 ),
 ( 0.000000000000000000, 1.000000000000000000 ),
 .UNSPECIFIED. ) ;
#29487 = CARTESIAN_POINT ( 'NONE',  ( 15.00000000000000000, 243.6999999999999886, 0.000000000000000000 ) ) ;
#29488 = CARTESIAN_POINT ( 'NONE',  ( 20.99999999999997513, 246.7375000000000114, -5.999999999999999112 ) ) ;
#29489 = CARTESIAN_POINT ( 'NONE',  ( 20.99999999999998579, 248.0875000000000057, -5.999999999999997335 ) ) ;
#29490 = CARTESIAN_POINT ( 'NONE',  ( 26.75643035624999655, -3.323476615752267715, -5.803124999385441463 ) ) ;
#29491 = CARTESIAN_POINT ( 'NONE',  ( -4.944772684328673229, 102.9851862821014663, 11.48171059495397728 ) ) ;
#29492 = CARTESIAN_POINT ( 'NONE',  ( 5.770363421894130873, 18.56481371789855928, -14.38691631536193860 ) ) ;
#29493 = CARTESIAN_POINT ( 'NONE',  ( 25.05336835492019176, -3.464101615137944457, 165.1724917731197024 ) ) ;
#29494 = CARTESIAN_POINT ( 'NONE',  ( 15.24356964374999990, 239.9218750006145626, -3.323476615752268604 ) ) ;
#29495 = CARTESIAN_POINT ( 'NONE',  ( -34.76413769728823411, 212.1499508600178387, 3.954877714930865817 ) ) ;
#29496 = DIRECTION ( 'NONE',  ( 1.000000000000000000, 0.000000000000000000, 0.000000000000000000 ) ) ;
#29497 = CARTESIAN_POINT ( 'NONE',  ( 27.46224632087531958, 5.407089921784862696, 159.6822773018186297 ) ) ;
#29498 = CARTESIAN_POINT ( 'NONE',  ( -5.529263428287297444, 26.32731371789854791, -7.954856959092311719 ) ) ;
#29499 = CARTESIAN_POINT ( 'NONE',  ( -59.70163769728823411, 215.6869285224996986, -3.149950860017881382 ) ) ;
#29500 = CARTESIAN_POINT ( 'NONE',  ( -66.62872103062156270, 201.4690446883607819, 2.162041339862843525 ) ) ;
#29501 = CARTESIAN_POINT ( 'NONE',  ( 0.000000000000000000, 0.000000000000000000, 0.000000000000000000 ) ) ;
#29502 = CARTESIAN_POINT ( 'NONE',  ( 18.00000000000000000, 240.9250000000000114, -5.196152422706630247 ) ) ;
#29503 = CARTESIAN_POINT ( 'NONE',  ( -27.24356964375000345, 197.1593750006145456, 0.000000000000000000 ) ) ;
#29504 = CARTESIAN_POINT ( 'NONE',  ( 15.53471296425188797, 140.1773137178985564, 2.908627838312457747 ) ) ;
#29505 = CARTESIAN_POINT ( 'NONE',  ( -57.51711230271181563, 216.4690446883607535, -1.857196546604089393 ) ) ;
#29506 = ORIENTED_EDGE ( 'NONE', *, *, #31547, .F. ) ;
#29507 = CARTESIAN_POINT ( 'NONE',  ( -12.46528703574805697, 49.79768628210145209, -2.660918448318280838 ) ) ;
#29508 = CARTESIAN_POINT ( 'NONE',  ( 26.99999999999999645, 245.3312500012290513, -7.347880794884117764E-16 ) ) ;
#29509 = EDGE_CURVE ( 'NONE', #14348, #21823, #25841, .T. ) ;
#29510 = CARTESIAN_POINT ( 'NONE',  ( 13.50000000000001421, 198.8000000000000114, 23.38268590217984055 ) ) ;
#29511 = CARTESIAN_POINT ( 'NONE',  ( 31.19640481644053409, 7.209453229046482114, 166.5454403520519122 ) ) ;
#29512 = CARTESIAN_POINT ( 'NONE',  ( 26.99999999999999645, 3.464101615137755275, -2.381249998770954779 ) ) ;
#29513 = CARTESIAN_POINT ( 'NONE',  ( -67.81622103062156270, 211.6261429550005744, 6.530955311639228711 ) ) ;
#29514 = CARTESIAN_POINT ( 'NONE',  ( 22.80587116629410360, -3.604726614523235284, -1.753124999385512028 ) ) ;
#29515 = CARTESIAN_POINT ( 'NONE',  ( -1.715153634034234598, 51.52268628210144641, -9.534712964251941258 ) ) ;
#29516 = CARTESIAN_POINT ( 'NONE',  ( 26.97716818855048260, 0.000000000000000000, 49.47706554351410801 ) ) ;
#29517 = CARTESIAN_POINT ( 'NONE',  ( 26.99999999999999645, 244.8625000000000114, -3.464101615137755275 ) ) ;
#29518 = EDGE_CURVE ( 'NONE', #32797, #36568, #35266, .T. ) ;
#29519 = CARTESIAN_POINT ( 'NONE',  ( -8.715434833791929847, 87.46018628210144641, -8.962234695871762469 ) ) ;
#29520 = CARTESIAN_POINT ( 'NONE',  ( 10.56230152254336474, 3.464101615137328505, -4.987500000000038014 ) ) ;
#29521 = CARTESIAN_POINT ( 'NONE',  ( 36.95541128647934670, 7.347880794884117764E-16, 163.5289060425172636 ) ) ;
#29522 = CARTESIAN_POINT ( 'NONE',  ( -42.15435043487492095, 254.8329415120769283, -2.500000000000000000 ) ) ;
#29523 = CARTESIAN_POINT ( 'NONE',  ( -35.67863628793906372, 245.9410842096246199, 2.500000000000000000 ) ) ;
#29524 = CARTESIAN_POINT ( 'NONE',  ( 18.12178482187499640, 4.985214923628404904, -10.11562499938548143 ) ) ;
#29525 = AXIS2_PLACEMENT_3D ( 'NONE', #4662, #16245, #37422 ) ;
#29526 = CARTESIAN_POINT ( 'NONE',  ( 26.99999999999999645, 7.347880794884117764E-16, -0.6750000000000089262 ) ) ;
#29527 = CARTESIAN_POINT ( 'NONE',  ( 37.20704201011650269, -3.604726614523238837, 163.6104101269339424 ) ) ;
#29528 = CARTESIAN_POINT ( 'NONE',  ( 28.07136751237244354, 5.196152422706636465, 165.2472402554827795 ) ) ;
#29529 = CARTESIAN_POINT ( 'NONE',  ( 26.99999999999983658, -3.464101615137843648, -6.956249998770940302 ) ) ;
#29530 = CARTESIAN_POINT ( 'NONE',  ( 18.00000000000000355, 248.2750000000000057, 5.196152422706632912 ) ) ;
#29531 = CARTESIAN_POINT ( 'NONE',  ( 27.24356964374999279, 196.0156250006145342, -15.72908226750539207 ) ) ;
#29532 = CARTESIAN_POINT ( 'NONE',  ( 12.46528703574811558, 102.8023137178985422, -2.660918448318005503 ) ) ;
#29533 = CARTESIAN_POINT ( 'NONE',  ( -12.50000000000000355, 113.9101862821014493, -0.1745138560725492671 ) ) ;
#29534 = VECTOR ( 'NONE', #14612, 1000.000000000000000 ) ;
#29535 = ORIENTED_EDGE ( 'NONE', *, *, #425, .T. ) ;
#29536 = CARTESIAN_POINT ( 'NONE',  ( -1.926257025242585782E-15, 195.6406250006145058, -31.45816453501075927 ) ) ;
#29537 = CARTESIAN_POINT ( 'NONE',  ( 23.87821517812499650, 240.1468750006145285, -4.985214923628404904 ) ) ;
#29538 = EDGE_CURVE ( 'NONE', #12071, #7872, #30114, .T. ) ;
#29539 = CARTESIAN_POINT ( 'NONE',  ( 0.1745138560722461762, 77.78981371789853938, 15.50000000000000533 ) ) ;
#29540 = CARTESIAN_POINT ( 'NONE',  ( 23.87821517812499650, 4.985214923628404904, -4.453124999385494220 ) ) ;
#29541 = CARTESIAN_POINT ( 'NONE',  ( 26.75643035624999655, 248.2843750006145456, -7.049594010296217766E-16 ) ) ;
#29542 = CARTESIAN_POINT ( 'NONE',  ( 6.594114490232313663, 92.06018628210145494, 6.840914352312096547 ) ) ;
#29543 = PRODUCT_DEFINITION_SHAPE ( 'NONE', 'NONE',  #32183 ) ;
#29544 = FACE_OUTER_BOUND ( 'NONE', #9580, .T. ) ;
#29545 = CARTESIAN_POINT ( 'NONE',  ( 3.474262827703532341, 73.76481371789856212, -8.843639120294245259 ) ) ;
#29546 = CARTESIAN_POINT ( 'NONE',  ( 13.44051670066911619, -5.407089921784859143, -5.465624999385548577 ) ) ;
#29547 = CLOSED_SHELL ( 'NONE', ( #8091, #3941, #22800, #15207, #21428, #21752, #8564, #36028, #27481, #25810, #28932, #3386, #8941, #30685, #34180, #36449, #5715, #11344, #7413, #31595, #5182, #32376, #11296, #29244, #26940, #31005, #11792, #15982, #24521, #8955, #1791, #26877, #1242, #12964, #23491, #28186 ) ) ;
#29548 = CARTESIAN_POINT ( 'NONE',  ( 18.12178482187499640, 242.0218750006145001, -4.985214923628404904 ) ) ;
#29549 = CARTESIAN_POINT ( 'NONE',  ( 12.53471296425189330, 57.37731371789855928, 2.311890736173451977 ) ) ;
#29550 = DIRECTION ( 'NONE',  ( 0.000000000000000000, 1.000000000000000000, 0.000000000000000000 ) ) ;
#29551 = CARTESIAN_POINT ( 'NONE',  ( 11.48171059495397728, 100.6851862821014691, 4.944772684328674117 ) ) ;
#29552 = CARTESIAN_POINT ( 'NONE',  ( 10.56230152254410903, 0.000000000000000000, -5.737499998771017573 ) ) ;
#29553 = CARTESIAN_POINT ( 'NONE',  ( -69.20163769728823411, 213.9548777149308592, -2.149950860017830756 ) ) ;
#29554 = DIRECTION ( 'NONE',  ( 0.9961946980917462113, 0.000000000000000000, -0.08715574274765118534 ) ) ;
#29555 = CARTESIAN_POINT ( 'NONE',  ( 37.09755260828975310, 7.646167579472015790E-16, 162.3589405374562205 ) ) ;
#29556 = CARTESIAN_POINT ( 'NONE',  ( 10.83675517735155225, 92.06018628210145494, 11.08355503943142573 ) ) ;
#29557 = CARTESIAN_POINT ( 'NONE',  ( 19.68408634441912142, -5.407089921784861808, -3.646874999385540939 ) ) ;
#29558 = CARTESIAN_POINT ( 'NONE',  ( 0.1745138560725515708, 5.810186282101447830, -12.50000000000000355 ) ) ;
#29559 = DIRECTION ( 'NONE',  ( -0.000000000000000000, -0.000000000000000000, 1.000000000000000000 ) ) ;
#29560 = EDGE_CURVE ( 'NONE', #6368, #11787, #32306, .T. ) ;
#29561 = CARTESIAN_POINT ( 'NONE',  ( 10.56230152254410903, 0.000000000000000000, -5.551115123125782702E-14 ) ) ;
#29562 = CARTESIAN_POINT ( 'NONE',  ( 6.594114490232313663, 110.4601862821014606, 6.840914352312096547 ) ) ;
#29563 = CARTESIAN_POINT ( 'NONE',  ( 2.999999999999997335, 252.0000000000000000, 2.500000000000000000 ) ) ;
#29564 = CARTESIAN_POINT ( 'NONE',  ( 6.092822981423978490, 6.385186282101440902, -14.25334919248782306 ) ) ;
#29565 = CARTESIAN_POINT ( 'NONE',  ( 13.62178482187499640, 195.6593750006145456, -23.59362340125807123 ) ) ;
#29566 = CARTESIAN_POINT ( 'NONE',  ( 26.75643035624999655, 241.3843750006145399, 3.323476615752267715 ) ) ;
#29567 = EDGE_LOOP ( 'NONE', ( #25459, #14112, #1664, #29506 ) ) ;
#29568 = CARTESIAN_POINT ( 'NONE',  ( 34.33409119757650529, -5.407089921784855591, 166.5908959372197558 ) ) ;
#29569 = CARTESIAN_POINT ( 'NONE',  ( 23.87821517812500005, -4.985214923628404016, -3.140624999385472016 ) ) ;
#29570 = CARTESIAN_POINT ( 'NONE',  ( 22.56230152254376975, -3.464101615137950230, -5.099999998771011178 ) ) ;
#29571 = DIRECTION ( 'NONE',  ( -0.000000000000000000, 0.000000000000000000, 1.000000000000000000 ) ) ;
#29572 = CARTESIAN_POINT ( 'NONE',  ( 25.01527935017339033, 0.000000000000000000, 50.00000000000000000 ) ) ;
#29573 = CARTESIAN_POINT ( 'NONE',  ( 25.08932009880328096, 0.000000000000000000, 165.5834220860826349 ) ) ;
#29574 = CARTESIAN_POINT ( 'NONE',  ( 22.80587116629410716, 7.646167579472015790E-16, -0.3656249993855553715 ) ) ;
#29575 = CARTESIAN_POINT ( 'NONE',  ( -1.715153634034442431, 22.87731371789854151, 9.534712964251900402 ) ) ;
#29576 = CARTESIAN_POINT ( 'NONE',  ( 27.24356964375000345, 197.3843750006145399, -3.336375036156643733E-15 ) ) ;
#29578 = ORIENTED_EDGE ( 'NONE', *, *, #908, .T. ) ;
#29577 = VERTEX_POINT ( 'NONE', #13252 ) ;
#29579 = CARTESIAN_POINT ( 'NONE',  ( 21.00000000000000000, 247.3843750006145399, -6.646953231504538984 ) ) ;
#29580 = CARTESIAN_POINT ( 'NONE',  ( -6.932735513424201912, 32.65231371789855075, 10.69584247140429412 ) ) ;
#29581 = CARTESIAN_POINT ( 'NONE',  ( 15.24356964375000167, -3.323476615752272600, -1.453124999385472016 ) ) ;
#29582 = CARTESIAN_POINT ( 'NONE',  ( 2.908627838312458636, 137.8773137178985735, -15.53471296425188442 ) ) ;
#29583 = CARTESIAN_POINT ( 'NONE',  ( 18.00000000000000000, 5.196152422706630247, -7.668749998770957532 ) ) ;
#29584 = ORIENTED_EDGE ( 'NONE', *, *, #26971, .F. ) ;
#29585 = CARTESIAN_POINT ( 'NONE',  ( 10.31873187879410558, 0.000000000000000000, -4.246874999385502392 ) ) ;
#29586 = VERTEX_POINT ( 'NONE', #18578 ) ;
#29587 = CARTESIAN_POINT ( 'NONE',  ( 27.24356964375000700, 197.7406250006145285, 15.72908226750537075 ) ) ;
#29588 = CARTESIAN_POINT ( 'NONE',  ( 31.03952447949476223, 7.209453229046482114, 164.7522898954867401 ) ) ;
#29589 = ADVANCED_FACE ( 'NONE', ( #24061 ), #12680, .T. ) ;
#29590 = CARTESIAN_POINT ( 'NONE',  ( -63.85044563604516554, 203.6929966515019430, -6.137860380172892150 ) ) ;
#29591 = CARTESIAN_POINT ( 'NONE',  ( 18.12178482187499640, 249.2218750006145171, -4.985214923628404904 ) ) ;
#29592 = SHAPE_REPRESENTATION_RELATIONSHIP ( 'NONE' , 'NONE' ,  #10397, #3821 ) ;
#29593 = CARTESIAN_POINT ( 'NONE',  ( 0.000000000000000000, 195.0000000000000000, -27.00000000000000000 ) ) ;
#29594 = CARTESIAN_POINT ( 'NONE',  ( -44.25669563604517265, 209.8844732041982297, -4.499999999999996447 ) ) ;
#29595 = CARTESIAN_POINT ( 'NONE',  ( 27.00000000000001421, 197.0374999999999943, 15.58845726811988897 ) ) ;
#29596 = CARTESIAN_POINT ( 'NONE',  ( 28.09467017918796472, 5.407089921784856479, 166.9109150798468306 ) ) ;
#29597 = EDGE_LOOP ( 'NONE', ( #30845, #6930, #37021, #6201 ) ) ;
#29598 = CARTESIAN_POINT ( 'NONE',  ( -27.87851222004085017, 209.4701072313699797, 7.986820506746719950 ) ) ;
#29599 = CARTESIAN_POINT ( 'NONE',  ( -0.1745138560722442889, 8.789813717898553591, -15.50000000000000533 ) ) ;
#29600 = CARTESIAN_POINT ( 'NONE',  ( -59.70163769728823411, 217.4189793300686233, -4.149950860017907139 ) ) ;
#29601 = CARTESIAN_POINT ( 'NONE',  ( 8.710071997420127943, 128.2851862821014493, 3.796722387233375073 ) ) ;
#29602 = EDGE_CURVE ( 'NONE', #12569, #190, #5185, .T. ) ;
#29603 = DIRECTION ( 'NONE',  ( 0.000000000000000000, -0.000000000000000000, 1.000000000000000000 ) ) ;
#29604 = CARTESIAN_POINT ( 'NONE',  ( -2.660918448318275509, 29.09768628210144925, 12.46528703574805874 ) ) ;
#29605 = CARTESIAN_POINT ( 'NONE',  ( 13.56230152254410726, 5.196152422706636465, -5.925000000000041567 ) ) ;
#29607 = ADVANCED_FACE ( 'NONE', ( #21228 ), #3958, .T. ) ;
#29606 = ORIENTED_EDGE ( 'NONE', *, *, #22014, .T. ) ;
#29608 = CARTESIAN_POINT ( 'NONE',  ( -27.87471972953270338, 210.0000000000000284, -8.000000000000000000 ) ) ;
#29609 = CARTESIAN_POINT ( 'NONE',  ( 8.927990412390657937, 126.2726862821014464, -13.04141134922759804 ) ) ;
#29610 = CARTESIAN_POINT ( 'NONE',  ( 21.00000000000000355, 0.000000000000000000, 50.00000000000001421 ) ) ;
#29611 = CARTESIAN_POINT ( 'NONE',  ( -6.594114490232462877, 143.3398137178985507, 6.840914352311949109 ) ) ;
#29612 = CARTESIAN_POINT ( 'NONE',  ( -27.24356964375000345, 198.4531250006145342, 0.000000000000000000 ) ) ;
#29613 = CARTESIAN_POINT ( 'NONE',  ( 1.069080835302379631E-14, 197.9750000012290343, 27.00000000000000000 ) ) ;
#29614 = CARTESIAN_POINT ( 'NONE',  ( 10.56230152254410903, 0.000000000000000000, -1.237499998771041110 ) ) ;
#29615 = CARTESIAN_POINT ( 'NONE',  ( 28.29894145125277660, -5.407089921784865361, 169.2457464034993961 ) ) ;
#29616 = CYLINDRICAL_SURFACE ( 'NONE', #31462, 6.000000000000001776 ) ;
#29617 = CARTESIAN_POINT ( 'NONE',  ( 2.064181346179061460, 77.50231371789855928, 9.465287035748106703 ) ) ;
#29618 = LINE ( 'NONE', #3274, #33691 ) ;
#29619 = VERTEX_POINT ( 'NONE', #35414 ) ;
#29620 = CARTESIAN_POINT ( 'NONE',  ( 26.99999999999999645, 243.0812500012290513, -7.347880794884117764E-16 ) ) ;
#29621 = CARTESIAN_POINT ( 'NONE',  ( 10.69584247140429589, 103.9523137178985621, 6.932735513424201024 ) ) ;
#29622 = CARTESIAN_POINT ( 'NONE',  ( 10.31873187879411091, -3.604726614523244610, -3.759374999385526106 ) ) ;
#29623 = DIRECTION ( 'NONE',  ( -0.000000000000000000, 1.000000000000000000, -0.000000000000000000 ) ) ;
#29624 = CARTESIAN_POINT ( 'NONE',  ( 15.24356964375000167, -3.323476615752272600, -5.615624999385488536 ) ) ;
#29625 = CARTESIAN_POINT ( 'NONE',  ( -10.69584247140429412, 53.35231371789855359, -6.932735513424201024 ) ) ;
#29626 = CARTESIAN_POINT ( 'NONE',  ( -13.62178482187498396, 197.2343750006145626, 23.59362340125808188 ) ) ;
#29627 = ORIENTED_EDGE ( 'NONE', *, *, #13611, .F. ) ;
#29628 = ORIENTED_EDGE ( 'NONE', *, *, #6337, .T. ) ;
#29629 = CARTESIAN_POINT ( 'NONE',  ( 26.75643035624999655, 3.323476615752271268, -5.728124999385479477 ) ) ;
#29630 = CARTESIAN_POINT ( 'NONE',  ( 22.56230152254411792, 7.347880794884125653E-16, -1.125000000000042633 ) ) ;
#29631 = CARTESIAN_POINT ( 'NONE',  ( 21.00000000000000000, 246.2593750006145115, 6.646953231504538984 ) ) ;
#29632 = CARTESIAN_POINT ( 'NONE',  ( -4.622313124798576922, 32.83518628210143930, -11.61527771782819762 ) ) ;
#29633 =( BOUNDED_CURVE ( )  B_SPLINE_CURVE ( 2, ( #16036, #27023, #29862, #20980, #18320, #7131, #1233, #33088, #3898 ),
 .UNSPECIFIED., .F., .F. ) 
 B_SPLINE_CURVE_WITH_KNOTS ( ( 3, 2, 2, 2, 3 ),
 ( 0.7291666666666667407, 0.7361111111111111605, 0.7500000000000000000, 0.7638888888888888395, 0.7708333333333333703 ),
 .UNSPECIFIED. ) 
 CURVE ( )  GEOMETRIC_REPRESENTATION_ITEM ( )  RATIONAL_B_SPLINE_CURVE ( ( 0.9330127018922192983, 0.9330127018922198534, 1.000000000000000000, 0.8660254037844387076, 1.000000000000000000, 0.8660254037844387076, 1.000000000000000000, 0.9330127018922187432, 0.9330127018922192983 ) ) 
 REPRESENTATION_ITEM ( '' )  );
#29634 = CARTESIAN_POINT ( 'NONE',  ( -33.56919563604517265, 216.5000000000000000, -0.1155267958017906493 ) ) ;
#29635 = CARTESIAN_POINT ( 'NONE',  ( 22.80587116629410360, 7.646167579472015790E-16, -1.715624999385545468 ) ) ;
#29636 = CARTESIAN_POINT ( 'NONE',  ( -33.76711230271183695, 214.4690446883608104, -1.321298161741814914 ) ) ;
#29637 = CARTESIAN_POINT ( 'NONE',  ( 30.77233765568754720, -6.928203230275506996, 161.6983305247614453 ) ) ;
#29638 = CARTESIAN_POINT ( 'NONE',  ( -4.622313124798826500, 87.56481371789855928, 11.61527771782809637 ) ) ;
#29639 = CARTESIAN_POINT ( 'NONE',  ( -62.47247103062156981, 207.6499508600178387, 3.839350919129076445 ) ) ;
#29640 = EDGE_CURVE ( 'NONE', #14469, #7496, #33338, .T. ) ;
#29641 = CARTESIAN_POINT ( 'NONE',  ( -38.12872103062156270, 201.4690446883607819, 2.162041339862843525 ) ) ;
#29642 = CARTESIAN_POINT ( 'NONE',  ( 26.75643035624999655, -3.323476615752267271, -6.365624999385492089 ) ) ;
#29643 = CARTESIAN_POINT ( 'NONE',  ( 2.908627838312458636, 55.07731371789854080, -15.53471296425188442 ) ) ;
#29644 = CARTESIAN_POINT ( 'NONE',  ( -54.54836230271183695, 202.5810206699313767, -4.149950860017804111 ) ) ;
#29645 = AXIS2_PLACEMENT_3D ( 'NONE', #26579, #4214, #12566 ) ;
#29646 = DIRECTION ( 'NONE',  ( 0.7660444769304640689, 0.000000000000000000, 0.6427875693915772182 ) ) ;
#29647 = CARTESIAN_POINT ( 'NONE',  ( -2.660918448318275509, 93.49768628210145494, 12.46528703574805874 ) ) ;
#29648 = ADVANCED_FACE ( 'NONE', ( #33151 ), #10067, .T. ) ;
#29649 = CARTESIAN_POINT ( 'NONE',  ( 5.770363421893814682, 28.23518628210144854, 14.38691631536207183 ) ) ;
#29650 = CARTESIAN_POINT ( 'NONE',  ( 10.56230152254410903, 7.347880794884117764E-16, -10.00000000000000000 ) ) ;
#29651 =( BOUNDED_CURVE ( )  B_SPLINE_CURVE ( 2, ( #2968, #14538, #678, #3155, #123, #32147, #20988 ),
 .UNSPECIFIED., .F., .F. ) 
 B_SPLINE_CURVE_WITH_KNOTS ( ( 3, 2, 2, 3 ),
 ( 0.3043478260869560970, 0.3115942028985501100, 0.3188405797101441785, 0.3260869565217382471 ),
 .UNSPECIFIED. ) 
 CURVE ( )  GEOMETRIC_REPRESENTATION_ITEM ( )  RATIONAL_B_SPLINE_CURVE ( ( 1.000000000000008216, 0.8660254037844304920, 1.000000000000000000, 0.8660254037844387076, 1.000000000000000000, 0.8660254037844551389, 0.9999999999999835687 ) ) 
 REPRESENTATION_ITEM ( '' )  );
#29652 = CARTESIAN_POINT ( 'NONE',  ( 30.70615376348499836, -7.209453229046482114, 160.9418451752858346 ) ) ;
#29653 = CARTESIAN_POINT ( 'NONE',  ( 15.46528703574804986, 45.19768628210142225, 3.257655550457285720 ) ) ;
#29654 = DIRECTION ( 'NONE',  ( -0.8083506638593008775, -0.5887012860850803220, 0.000000000000000000 ) ) ;
#29655 = FACE_OUTER_BOUND ( 'NONE', #14624, .T. ) ;
#29656 = CARTESIAN_POINT ( 'NONE',  ( -43.47247103062156981, 206.6499508600178672, 5.571401726697986057 ) ) ;
#29657 = CARTESIAN_POINT ( 'NONE',  ( 27.00000000000000355, 195.7250000000000227, -3.306546357697854128E-15 ) ) ;
#29658 = CARTESIAN_POINT ( 'NONE',  ( 8.715434833791931624, 18.46018628210144286, 8.962234695871760692 ) ) ;
#29659 = CARTESIAN_POINT ( 'NONE',  ( 18.12178482187500350, 249.4843750006145342, 4.985214923628407568 ) ) ;
#29660 = CARTESIAN_POINT ( 'NONE',  ( 3.796722387233182339, 123.2148137178985792, 8.710071997420207879 ) ) ;
#29661 = CARTESIAN_POINT ( 'NONE',  ( 26.75643035624999655, 245.5468750006145342, 3.323476615752267271 ) ) ;
#29662 = AXIS2_PLACEMENT_3D ( 'NONE', #35618, #27281, #6815 ) ;
#29663 = VERTEX_POINT ( 'NONE', #8625 ) ;
#29664 = CARTESIAN_POINT ( 'NONE',  ( 15.00000000000000000, 3.464101615137752166, -6.787499999999996092 ) ) ;
#29665 = CARTESIAN_POINT ( 'NONE',  ( 26.99999999999991118, -3.464101615137797463, -4.312500000000005329 ) ) ;
#29666 = CARTESIAN_POINT ( 'NONE',  ( 27.00000000000000355, 197.5250000000000057, -3.306546357697854128E-15 ) ) ;
#29667 = CARTESIAN_POINT ( 'NONE',  ( 19.68408634441910721, 5.407089921784857367, -7.490624999385548044 ) ) ;
#29668 = CARTESIAN_POINT ( 'NONE',  ( 37.48975345065418452, 7.646167579472015790E-16, 166.8418166788690655 ) ) ;
#29669 = DIRECTION ( 'NONE',  ( -0.000000000000000000, -1.000000000000000000, -0.000000000000000000 ) ) ;
#29670 = CARTESIAN_POINT ( 'NONE',  ( -13.66537537263149282, 216.1427711317592752, 5.155187915310053270 ) ) ;
#29671 = CARTESIAN_POINT ( 'NONE',  ( 11.48171059495397728, 54.68518628210144783, 4.944772684328674117 ) ) ;
#29672 = ORIENTED_EDGE ( 'NONE', *, *, #30455, .T. ) ;
#29673 = ORIENTED_EDGE ( 'NONE', *, *, #10728, .T. ) ;
#29674 = CARTESIAN_POINT ( 'NONE',  ( 20.99999999999997868, 204.0000000000000000, 0.000000000000000000 ) ) ;
#29675 = CARTESIAN_POINT ( 'NONE',  ( 21.00000000000000355, 0.000000000000000000, 50.00000000000001421 ) ) ;
#29676 = CARTESIAN_POINT ( 'NONE',  ( 1.120210788295102201E-13, 195.3875000000000455, -27.00000000000000711 ) ) ;
#29677 = CARTESIAN_POINT ( 'NONE',  ( 15.24356964374999990, 0.000000000000000000, -5.540624999385457272 ) ) ;
#29678 = AXIS2_PLACEMENT_3D ( 'NONE', #28101, #7832, #36438 ) ;
#29679 = CARTESIAN_POINT ( 'NONE',  ( 2.660918448318279950, 88.89768628210146062, -12.46528703574805697 ) ) ;
#29680 = CARTESIAN_POINT ( 'NONE',  ( 6.092822981423662299, 12.81481371789855217, 14.25334919248795096 ) ) ;
#29681 = DIRECTION ( 'NONE',  ( -0.000000000000000000, -1.000000000000000000, -0.000000000000000000 ) ) ;
#29682 = CARTESIAN_POINT ( 'NONE',  ( -6.000000000000000888, -20.00000000000000000, 20.00000000000000711 ) ) ;
#29683 = CARTESIAN_POINT ( 'NONE',  ( -32.19122103062156270, 208.9097554298617752, -4.530955311639240257 ) ) ;
#29684 = CARTESIAN_POINT ( 'NONE',  ( -4.605287895664654130, 226.1383394588005444, 2.499999999999999556 ) ) ;
#29685 = CARTESIAN_POINT ( 'NONE',  ( 28.40800656884236730, -5.196152422706632912, 169.0950422780865097 ) ) ;
#29686 = CARTESIAN_POINT ( 'NONE',  ( 4.944772684328420986, 132.4148137178985678, 11.48171059495408208 ) ) ;
#29687 = CARTESIAN_POINT ( 'NONE',  ( -55.14955436395487709, 214.8429017333601792, -4.673758765035196383 ) ) ;
#29688 = CARTESIAN_POINT ( 'NONE',  ( -35.94419563604516554, 201.5000000000000000, 0.1155267958018195706 ) ) ;
#29689 = AXIS2_PLACEMENT_3D ( 'NONE', #7811, #25047, #28265 ) ;
#29690 = CARTESIAN_POINT ( 'NONE',  ( 10.56230152254410726, 0.000000000000000000, -4.387499998770999277 ) ) ;
#29691 = CARTESIAN_POINT ( 'NONE',  ( 27.24356964375000700, 199.0906250006145228, 15.72908226750537075 ) ) ;
#29692 = CARTESIAN_POINT ( 'NONE',  ( 11.08355503943118769, 113.4398137178985593, 10.83675517735179028 ) ) ;
#29693 = CARTESIAN_POINT ( 'NONE',  ( -61.27752896937850124, 213.3500491399821613, 5.571401726697954970 ) ) ;
#29694 = VERTEX_POINT ( 'NONE', #19835 ) ;
#29695 = CARTESIAN_POINT ( 'NONE',  ( -12.50000000000000355, 31.11018628210143788, -0.1745138560725492671 ) ) ;
#29696 = CARTESIAN_POINT ( 'NONE',  ( -4.712253383274792817, 225.7113004343964349, -2.500000000000000000 ) ) ;
#29697 = CARTESIAN_POINT ( 'NONE',  ( 34.42112650116913386, -5.196152422706635576, 168.9830381333390505 ) ) ;
#29698 = CARTESIAN_POINT ( 'NONE',  ( 28.16820783713129472, 5.407089921784862696, 167.7514543563617622 ) ) ;
#29699 = CARTESIAN_POINT ( 'NONE',  ( 10.83675517735155225, 101.2601862821014436, 11.08355503943142573 ) ) ;
#29700 = CARTESIAN_POINT ( 'NONE',  ( -63.85788769728821279, 216.4690446883607535, 1.857196546604031662 ) ) ;
#29701 = CARTESIAN_POINT ( 'NONE',  ( 22.80587116629410360, 7.646167579472015790E-16, -2.615624999385557370 ) ) ;
#29702 = CARTESIAN_POINT ( 'NONE',  ( 5.529263428287477744, 52.67268628210144499, -7.954856959092191815 ) ) ;
#29703 = DIRECTION ( 'NONE',  ( 1.000000000000000000, 0.000000000000000000, 0.000000000000000000 ) ) ;
#29704 = CARTESIAN_POINT ( 'NONE',  ( 1.120210788295102201E-13, 196.7375000000000398, -27.00000000000000711 ) ) ;
#29705 = CARTESIAN_POINT ( 'NONE',  ( -12.50000000000000355, 77.11018628210145209, -0.1745138560725492671 ) ) ;
#29706 = CARTESIAN_POINT ( 'NONE',  ( 13.49999999999999645, 199.8499999999999943, -23.38268590217984766 ) ) ;
#29707 = CARTESIAN_POINT ( 'NONE',  ( 26.99999999999999645, 247.5437500012290570, 3.464101615137751278 ) ) ;
#29708 = ORIENTED_EDGE ( 'NONE', *, *, #17924, .F. ) ;
#29709 = CARTESIAN_POINT ( 'NONE',  ( 27.58480908411420529, 5.407089921784856479, 161.0831760960101349 ) ) ;
#29710 = CARTESIAN_POINT ( 'NONE',  ( 26.75643035624999655, -3.323476615752267715, -8.953124999385474680 ) ) ;
#29711 = CARTESIAN_POINT ( 'NONE',  ( -27.00000000000000355, 195.6125000012290513, 0.000000000000000000 ) ) ;
#29712 = CARTESIAN_POINT ( 'NONE',  ( 24.94391043663983965, 3.604726614523240613, 166.7160302899652322 ) ) ;
#29713 = UNCERTAINTY_MEASURE_WITH_UNIT (LENGTH_MEASURE( 1.000000000000000082E-05 ), #36211, 'distance_accuracy_value', 'NONE');
#29714 = CARTESIAN_POINT ( 'NONE',  ( 25.01087993033039325, 0.000000000000000000, 164.6868468578000488 ) ) ;
#29715 = FACE_OUTER_BOUND ( 'NONE', #24280, .T. ) ;
#29716 = CARTESIAN_POINT ( 'NONE',  ( 15.00000000000000178, 247.7874999999999943, 3.464101615137757051 ) ) ;
#29717 = CARTESIAN_POINT ( 'NONE',  ( 5.778771075727756162E-15, 195.8656250006145285, 31.45816453501076637 ) ) ;
#29718 = CARTESIAN_POINT ( 'NONE',  ( 10.49813415416005213, 102.2273137178985536, -7.228626920338837358 ) ) ;
#29719 = CARTESIAN_POINT ( 'NONE',  ( -2.660918448318275509, 111.8976862821014606, 12.46528703574805874 ) ) ;
#29720 = VECTOR ( 'NONE', #20045, 1000.000000000000000 ) ;
#29721 = ORIENTED_EDGE ( 'NONE', *, *, #21502, .F. ) ;
#29722 = CARTESIAN_POINT ( 'NONE',  ( -13.62178482187498396, 195.8281250006145342, 23.59362340125808188 ) ) ;
#29723 = CARTESIAN_POINT ( 'NONE',  ( 21.00000000000000000, 240.6343750006145115, -6.646953231504538984 ) ) ;
#29724 = CARTESIAN_POINT ( 'NONE',  ( 15.53471296425188797, 75.77731371789855075, 2.908627838312457747 ) ) ;
#29725 = EDGE_CURVE ( 'NONE', #31979, #4816, #36179, .T. ) ;
#29726 = CARTESIAN_POINT ( 'NONE',  ( 15.24356964375000167, -3.323476615752272600, -5.165624999385460825 ) ) ;
#29727 = CARTESIAN_POINT ( 'NONE',  ( 15.24356964375000167, 248.5468750006145342, 3.323476615752272600 ) ) ;
#29728 = CARTESIAN_POINT ( 'NONE',  ( 9.500000000000005329, 90.91018628210146346, 0.1745138560725188748 ) ) ;
#29729 = CARTESIAN_POINT ( 'NONE',  ( 0.000000000000000000, -20.00000000000000000, 0.000000000000000000 ) ) ;
#29730 = CARTESIAN_POINT ( 'NONE',  ( 9.465287035748106703, 56.80231371789854933, -2.064181346179063237 ) ) ;
#29731 = CARTESIAN_POINT ( 'NONE',  ( 22.80587116629411071, -3.604726614523235284, -4.453124999385550176 ) ) ;
#29732 = CARTESIAN_POINT ( 'NONE',  ( 7.954856959092311719, 120.6273137178985451, -5.529263428287300108 ) ) ;
#29733 = CARTESIAN_POINT ( 'NONE',  ( 26.75643035624999655, 240.4843750006145058, 3.323476615752267271 ) ) ;
#29734 = CARTESIAN_POINT ( 'NONE',  ( -10.69584247140429412, 44.15231371789854364, -6.932735513424201024 ) ) ;
#29735 = DIRECTION ( 'NONE',  ( 0.000000000000000000, 0.000000000000000000, -1.000000000000000000 ) ) ;
#29736 = CARTESIAN_POINT ( 'NONE',  ( -6.932735513423968321, 106.1476862821014606, -10.69584247140445221 ) ) ;
#29737 = CARTESIAN_POINT ( 'NONE',  ( 16.56230152254410015, -6.928203230275506996, -6.974999998770984533 ) ) ;
#29738 = EDGE_CURVE ( 'NONE', #10416, #4247, #14496, .T. ) ;
#29739 = CARTESIAN_POINT ( 'NONE',  ( -69.59747103062156270, 212.3500491399821613, -3.839350919129076445 ) ) ;
#29740 = DIRECTION ( 'NONE',  ( 0.000000000000000000, 0.000000000000000000, -1.000000000000000000 ) ) ;
#29741 = CARTESIAN_POINT ( 'NONE',  ( 27.85934967376930516, 5.407089921784856479, 164.2211893949991293 ) ) ;
#29742 = CARTESIAN_POINT ( 'NONE',  ( -14.38691631536207183, 85.73518628210145209, 5.770363421893814682 ) ) ;
#29743 = CARTESIAN_POINT ( 'NONE',  ( 16.56230152254411436, 7.209453229046482114, -3.459374999385518290 ) ) ;
#29744 = CARTESIAN_POINT ( 'NONE',  ( -72.05441616160760532, 219.4495263357960368, 2.500000000000000000 ) ) ;
#29745 = CYLINDRICAL_SURFACE ( 'NONE', #17043, 2.649999999999999467 ) ;
#29746 = CARTESIAN_POINT ( 'NONE',  ( 7.234628195640322446, 198.3325961894323370, 26.99999999999999645 ) ) ;
#29747 = CARTESIAN_POINT ( 'NONE',  ( -0.1745138560725182642, 111.6101862821014521, 9.500000000000005329 ) ) ;
#29748 = CARTESIAN_POINT ( 'NONE',  ( 13.49999999999999645, 199.0625000012290400, -23.38268590217984766 ) ) ;
#29749 = EDGE_CURVE ( 'NONE', #17848, #26085, #6189, .T. ) ;
#29750 = CARTESIAN_POINT ( 'NONE',  ( -15.46528703574804986, 3.797686282101448096, -3.257655550457287497 ) ) ;
#29751 = CARTESIAN_POINT ( 'NONE',  ( 13.62178482187501416, 196.4093750006145456, 23.59362340125806767 ) ) ;
#29752 = CARTESIAN_POINT ( 'NONE',  ( 15.24356964374999990, 242.5093750006144830, -3.323476615752268604 ) ) ;
#29753 = ORIENTED_EDGE ( 'NONE', *, *, #5769, .T. ) ;
#29754 = CARTESIAN_POINT ( 'NONE',  ( 37.41131328218130392, 7.646167579472015790E-16, 165.9452414505865079 ) ) ;
#29755 = CARTESIAN_POINT ( 'NONE',  ( 26.75643035624999655, -3.323476615752267715, -1.753124999385447857 ) ) ;
#29756 = CARTESIAN_POINT ( 'NONE',  ( 27.24356964375000345, 199.6343750006145399, -3.336375036156643733E-15 ) ) ;
#29757 = LINE ( 'NONE', #755, #19743 ) ;
#29758 = CARTESIAN_POINT ( 'NONE',  ( 0.000000000000000000, 210.0000000000000284, -27.00000000000000000 ) ) ;
#29759 = LINE ( 'NONE', #3789, #37386 ) ;
#29760 = LINE ( 'NONE', #32229, #32709 ) ;
#29761 = CARTESIAN_POINT ( 'NONE',  ( 8.710071997420211432, 19.71481371789854720, -3.796722387233181895 ) ) ;
#29762 = CARTESIAN_POINT ( 'NONE',  ( 13.62178482187501416, 196.8593750006145342, 23.59362340125806767 ) ) ;
#29764 = ORIENTED_EDGE ( 'NONE', *, *, #26146, .T. ) ;
#29763 = ORIENTED_EDGE ( 'NONE', *, *, #20728, .F. ) ;
#29765 = CARTESIAN_POINT ( 'NONE',  ( 15.24356964375000167, 246.6343750006145115, 3.323476615752272600 ) ) ;
#29766 = CARTESIAN_POINT ( 'NONE',  ( 10.69584247140429589, 21.15231371789855075, 6.932735513424201024 ) ) ;
#29767 = CARTESIAN_POINT ( 'NONE',  ( 26.75643035624999655, -3.323476615752267715, -0.8531249993854884694 ) ) ;
#29768 = CARTESIAN_POINT ( 'NONE',  ( -14.25334919248795096, 134.7148137178985507, 6.092822981423662299 ) ) ;
#29769 = CARTESIAN_POINT ( 'NONE',  ( 21.00000000000000000, 6.928203230275506996, -8.156249998770968901 ) ) ;
#29770 = FACE_OUTER_BOUND ( 'NONE', #36472, .T. ) ;
#29771 = ORIENTED_EDGE ( 'NONE', *, *, #21970, .F. ) ;
#29772 = CARTESIAN_POINT ( 'NONE',  ( 10.31873187879410381, 3.604726614523240613, -5.634374999385534544 ) ) ;
#29773 = VECTOR ( 'NONE', #2574, 1000.000000000000000 ) ;
#29774 = VERTEX_POINT ( 'NONE', #17166 ) ;
#29775 = CARTESIAN_POINT ( 'NONE',  ( -27.24356964374999990, 195.7156250006145513, -15.72908226750537786 ) ) ;
#29776 = EDGE_CURVE ( 'NONE', #35447, #19526, #31556, .T. ) ;
#29777 = CARTESIAN_POINT ( 'NONE',  ( -12.50000000000000355, 123.1101862821014663, -0.1745138560725492671 ) ) ;
#29778 = CARTESIAN_POINT ( 'NONE',  ( 37.28875051894242887, 7.646167579472024665E-16, 164.5443426563950027 ) ) ;
#29779 = CARTESIAN_POINT ( 'NONE',  ( -67.21502896937850835, 217.3034525342667962, -4.350049139982195001 ) ) ;
#29780 = CARTESIAN_POINT ( 'NONE',  ( 20.99999999999999645, 246.0343750006144887, -6.646953231504538984 ) ) ;
#29781 = FACE_OUTER_BOUND ( 'NONE', #37399, .T. ) ;
#29782 = EDGE_CURVE ( 'NONE', #35280, #13088, #453, .T. ) ;
#29783 = CARTESIAN_POINT ( 'NONE',  ( -49.99627896937850835, 205.4690446883607535, -1.090244570138286351 ) ) ;
#29784 = CARTESIAN_POINT ( 'NONE',  ( 7.234628195640363302, 197.1674038105676914, -26.99999999999996803 ) ) ;
#29785 = CARTESIAN_POINT ( 'NONE',  ( 24.99456971211191814, -3.604726614523240613, 167.2950684582310146 ) ) ;
#29786 = ORIENTED_EDGE ( 'NONE', *, *, #5674, .T. ) ;
#29787 = CARTESIAN_POINT ( 'NONE',  ( 22.60769515458672885, 241.8236538117967029, -5.999999999999998224 ) ) ;
#29788 = CARTESIAN_POINT ( 'NONE',  ( -6.092822981423666739, 8.214813717898532985, -14.25334919248795096 ) ) ;
#29789 = CARTESIAN_POINT ( 'NONE',  ( -52.77455436395490551, 203.6929966515020283, 6.137860380172978303 ) ) ;
#29790 = EDGE_CURVE ( 'NONE', #8565, #15992, #11351, .T. ) ;
#29791 = CARTESIAN_POINT ( 'NONE',  ( -6.594114490232312775, 124.2601862821014578, -6.840914352312096547 ) ) ;
#29792 = LINE ( 'NONE', #3824, #30866 ) ;
#29793 = CARTESIAN_POINT ( 'NONE',  ( -12.46528703574805697, 22.19768628210145067, -2.660918448318280838 ) ) ;
#29794 = CARTESIAN_POINT ( 'NONE',  ( 10.56230152254411614, -3.464101615137761048, -5.812500000000043521 ) ) ;
#29795 = ORIENTED_EDGE ( 'NONE', *, *, #26378, .T. ) ;
#29796 = CARTESIAN_POINT ( 'NONE',  ( -34.96205436395489130, 214.6737587650351884, 4.842901733360205796 ) ) ;
#29797 = CARTESIAN_POINT ( 'NONE',  ( -5.770363421893818234, 124.8351862821014748, -14.38691631536207005 ) ) ;
#29798 = DIRECTION ( 'NONE',  ( 0.08715574274765150453, 0.000000000000000000, 0.9961946980917461003 ) ) ;
#29799 = CARTESIAN_POINT ( 'NONE',  ( -3.474262827703337830, 5.235186282101429001, -8.843639120294326972 ) ) ;
#29800 = CARTESIAN_POINT ( 'NONE',  ( -13.62178482187500528, 197.9281250006145569, -23.59362340125807123 ) ) ;
#29801 = CARTESIAN_POINT ( 'NONE',  ( 20.99999999999999645, 0.000000000000000000, -8.000000000000000000 ) ) ;
#29802 = CARTESIAN_POINT ( 'NONE',  ( 15.33009822426688729, 1.665651000388348013, -7.999999999999992895 ) ) ;
#29803 = CARTESIAN_POINT ( 'NONE',  ( 36.79199426871969791, 3.464101615138157619, 161.6610409823709347 ) ) ;
#29804 = EDGE_CURVE ( 'NONE', #32564, #32162, #6143, .T. ) ;
#29805 = CARTESIAN_POINT ( 'NONE',  ( -9.534712964251895073, 71.17731371789855643, -1.715153634034446428 ) ) ;
#29806 = CARTESIAN_POINT ( 'NONE',  ( 5.499999999999994671, 244.5000000000000000, -10.00000000000000000 ) ) ;
#29807 = ORIENTED_EDGE ( 'NONE', *, *, #3451, .F. ) ;
#29808 = CARTESIAN_POINT ( 'NONE',  ( 26.99999999999999645, 243.0437500012290570, 3.464101615137751278 ) ) ;
#29809 = CARTESIAN_POINT ( 'NONE',  ( 12.53471296425189330, 84.97731371789855359, 2.311890736173451533 ) ) ;
#29810 = CARTESIAN_POINT ( 'NONE',  ( 22.80587116629412847, 3.604726614523243278, -4.884374999385531879 ) ) ;
#29811 = CARTESIAN_POINT ( 'NONE',  ( -27.24356964374999635, 199.3906250006145342, 15.72908226750539384 ) ) ;
#29812 = CARTESIAN_POINT ( 'NONE',  ( 15.24356964374999990, 0.000000000000000000, -3.403124999385470417 ) ) ;
#29813 = CARTESIAN_POINT ( 'NONE',  ( 11.48171059495408208, 56.51481371789855501, -4.944772684328420986 ) ) ;
#29814 = EDGE_LOOP ( 'NONE', ( #26129, #3449, #27288, #11587 ) ) ;
#29815 = ORIENTED_EDGE ( 'NONE', *, *, #36432, .T. ) ;
#29816 = CARTESIAN_POINT ( 'NONE',  ( 15.24356964374999990, 3.323476615752268604, -5.578124999385491556 ) ) ;
#29817 = CARTESIAN_POINT ( 'NONE',  ( 26.75643035624999655, 243.6343750006145115, 3.323476615752267715 ) ) ;
#29818 = CARTESIAN_POINT ( 'NONE',  ( -11.48171059495397373, 13.28518628210142971, -4.944772684328680334 ) ) ;
#29819 = EDGE_CURVE ( 'NONE', #15328, #13615, #15609, .T. ) ;
#29820 = VECTOR ( 'NONE', #1681, 1000.000000000000000 ) ;
#29821 = CARTESIAN_POINT ( 'NONE',  ( -43.26711230271183695, 216.4690446883607535, -1.857196546604089393 ) ) ;
#29822 = CARTESIAN_POINT ( 'NONE',  ( 19.68408634441910721, -5.407089921784855591, -1.790624999385564964 ) ) ;
#29823 = CARTESIAN_POINT ( 'NONE',  ( -61.87127896937849414, 216.5309553116391612, 1.626142955000506873 ) ) ;
#29824 = PLANE ( 'NONE',  #29064 ) ;
#29825 = CARTESIAN_POINT ( 'NONE',  ( 11.61527771782809637, 94.46481371789855075, 4.622313124798827388 ) ) ;
#29826 = CARTESIAN_POINT ( 'NONE',  ( -45.45163769728823411, 213.9548777149308592, -2.149950860017830756 ) ) ;
#29827 = CARTESIAN_POINT ( 'NONE',  ( -69.79538769728823411, 211.8571965466039444, -6.469044688360768625 ) ) ;
#29828 = CARTESIAN_POINT ( 'NONE',  ( 15.24356964374999990, 3.323476615752268604, -6.590624999385473970 ) ) ;
#29829 = CARTESIAN_POINT ( 'NONE',  ( 22.56230152254576637, 3.464101615136798262, -0.9749999987710404881 ) ) ;
#29830 = CARTESIAN_POINT ( 'NONE',  ( 15.53471296425188797, 66.57731371789853370, 2.908627838312457747 ) ) ;
#29831 = ADVANCED_FACE ( 'NONE', ( #17720 ), #28707, .T. ) ;
#29832 = CARTESIAN_POINT ( 'NONE',  ( -40.49627896937850835, 201.4690446883607251, -2.162041339862721845 ) ) ;
#29833 = FACE_OUTER_BOUND ( 'NONE', #25653, .T. ) ;
#29834 = CARTESIAN_POINT ( 'NONE',  ( -2.311890736173176641, 88.32268628210144357, -12.53471296425194836 ) ) ;
#29835 = CARTESIAN_POINT ( 'NONE',  ( -13.04141134922759804, 22.77268628210143220, -8.927990412390657937 ) ) ;
#29836 = CARTESIAN_POINT ( 'NONE',  ( 22.56230152254411792, 7.347880794884125653E-16, -0.6750000000000366818 ) ) ;
#29837 = LINE ( 'NONE', #15446, #35517 ) ;
#29838 = CARTESIAN_POINT ( 'NONE',  ( -13.04141134922759804, 50.37268628210144783, -8.927990412390657937 ) ) ;
#29839 = CARTESIAN_POINT ( 'NONE',  ( -27.24356964374999279, 197.5906250006144944, 15.72908226750539384 ) ) ;
#29840 = DIRECTION ( 'NONE',  ( -0.000000000000000000, -1.000000000000000000, -0.000000000000000000 ) ) ;
#29841 = CARTESIAN_POINT ( 'NONE',  ( 14.99999999999945111, -3.464101615137439083, -1.256249998770955889 ) ) ;
#29842 = CARTESIAN_POINT ( 'NONE',  ( -41.69122103062155560, 208.3738570449993404, -6.530955311639226935 ) ) ;
#29843 = CARTESIAN_POINT ( 'NONE',  ( 1.069080835302379631E-14, 195.6124999999999829, 27.00000000000000000 ) ) ;
#29844 = CARTESIAN_POINT ( 'NONE',  ( -11.61527771782819940, 12.13518628210144534, 4.622313124798574258 ) ) ;
#29845 = CARTESIAN_POINT ( 'NONE',  ( 21.00000000000000000, 249.7468750006145797, -6.646953231504538984 ) ) ;
#29846 = CARTESIAN_POINT ( 'NONE',  ( -1.715153634034442431, 124.0773137178985621, 9.534712964251900402 ) ) ;
#29847 = CARTESIAN_POINT ( 'NONE',  ( 15.24356964375000167, 246.2968750006145626, 3.323476615752272600 ) ) ;
#29848 = ORIENTED_EDGE ( 'NONE', *, *, #20597, .T. ) ;
#29849 = CARTESIAN_POINT ( 'NONE',  ( 21.00000000000000000, 6.928203230275506996, -6.862499999999990941 ) ) ;
#29851 = AXIS2_PLACEMENT_3D ( 'NONE', #24709, #1772, #10487 ) ;
#29850 = CARTESIAN_POINT ( 'NONE',  ( -1.045839947578415010E-13, 196.0625000000000284, 27.00000000000000355 ) ) ;
#29852 = CARTESIAN_POINT ( 'NONE',  ( -6.932735513424201912, 133.8523137178985678, 10.69584247140429412 ) ) ;
#29853 = CARTESIAN_POINT ( 'NONE',  ( 10.31873187879411091, -3.604726614523240613, -7.753124999385540228 ) ) ;
#29854 = CARTESIAN_POINT ( 'NONE',  ( 31.27974749544297595, 7.209453229046475009, 167.4980515321021244 ) ) ;
#29855 =( BOUNDED_CURVE ( )  B_SPLINE_CURVE ( 2, ( #22597, #21440, #12327, #23901, #3982, #20683, #29383, #948, #35443 ),
 .UNSPECIFIED., .F., .F. ) 
 B_SPLINE_CURVE_WITH_KNOTS ( ( 3, 2, 2, 2, 3 ),
 ( 0.2708333333333333703, 0.2777777777777777901, 0.2916666666666666852, 0.3055555555555555802, 0.3125000000000000000 ),
 .UNSPECIFIED. ) 
 CURVE ( )  GEOMETRIC_REPRESENTATION_ITEM ( )  RATIONAL_B_SPLINE_CURVE ( ( 0.9330127018922194093, 0.9330127018922196314, 1.000000000000000000, 0.8660254037844387076, 1.000000000000000000, 0.8660254037844387076, 1.000000000000000000, 0.9330127018922194093, 0.9330127018922194093 ) ) 
 REPRESENTATION_ITEM ( '' )  );
#29856 = CARTESIAN_POINT ( 'NONE',  ( 5.438367727407757775E-14, 197.7500000012290400, -27.00000000000000355 ) ) ;
#29857 = EDGE_CURVE ( 'NONE', #22453, #26550, #25775, .T. ) ;
#29858 = LINE ( 'NONE', #29481, #17267 ) ;
#29859 = CARTESIAN_POINT ( 'NONE',  ( -8.962234695871760692, 57.56018628210145494, 8.715434833791933400 ) ) ;
#29860 = EDGE_LOOP ( 'NONE', ( #28862, #18741, #20786, #17417, #272 ) ) ;
#29861 = ORIENTED_EDGE ( 'NONE', *, *, #35826, .F. ) ;
#29862 = CARTESIAN_POINT ( 'NONE',  ( -13.49999999999998401, 196.0250000000000057, 23.38268590217985476 ) ) ;
#29863 = DIRECTION ( 'NONE',  ( 0.000000000000000000, 0.000000000000000000, -1.000000000000000000 ) ) ;
#29864 = DIRECTION ( 'NONE',  ( 0.000000000000000000, 0.000000000000000000, 1.000000000000000000 ) ) ;
#29866 = CARTESIAN_POINT ( 'NONE',  ( 1.069080835302379631E-14, 195.2750000012290457, 27.00000000000000000 ) ) ;
#29865 =( GEOMETRIC_REPRESENTATION_CONTEXT ( 3 ) GLOBAL_UNCERTAINTY_ASSIGNED_CONTEXT ( ( #7068 ) ) GLOBAL_UNIT_ASSIGNED_CONTEXT ( ( #1195, #15617, #32291 ) ) REPRESENTATION_CONTEXT ( 'NONE', 'WORKASPACE' ) );
#29867 = CARTESIAN_POINT ( 'NONE',  ( 26.75643035624999655, 7.049594010296217766E-16, -8.015624999385462246 ) ) ;
#29868 = CARTESIAN_POINT ( 'NONE',  ( -7.228626920339069173, 94.07268628210145778, 10.49813415415989581 ) ) ;
#29869 = CARTESIAN_POINT ( 'NONE',  ( 11.08355503943118769, 21.43981371789854506, 10.83675517735179028 ) ) ;
#29870 = ADVANCED_FACE ( 'NONE', ( #25687 ), #34404, .T. ) ;
#29871 = LINE ( 'NONE', #27217, #17599 ) ;
#29872 = CARTESIAN_POINT ( 'NONE',  ( 10.56230152254411081, 0.000000000000000000, -4.837499998771033205 ) ) ;
#29873 = CARTESIAN_POINT ( 'NONE',  ( -63.45461230271184405, 208.6787018382582346, -4.469044688360757966 ) ) ;
#29874 = DIRECTION ( 'NONE',  ( 0.08715574274765150453, 0.000000000000000000, 0.9961946980917461003 ) ) ;
#29875 = CARTESIAN_POINT ( 'NONE',  ( 37.26590362001785905, -3.464101615137751278, 167.0778496544691052 ) ) ;
#29876 = CARTESIAN_POINT ( 'NONE',  ( -0.1745138560723084320, 8.789813717898553591, -9.500000000000005329 ) ) ;
#29877 = CARTESIAN_POINT ( 'NONE',  ( -52.57663769728823411, 204.3130714775002730, 3.149950860017883603 ) ) ;
#29878 = CARTESIAN_POINT ( 'NONE',  ( -68.01413769728823411, 214.1499508600179240, 7.418979330068584233 ) ) ;
#29879 =( BOUNDED_CURVE ( )  B_SPLINE_CURVE ( 2, ( #10483, #27919, #13151, #13718, #36074, #13335, #1950 ),
 .UNSPECIFIED., .F., .F. ) 
 B_SPLINE_CURVE_WITH_KNOTS ( ( 3, 2, 2, 3 ),
 ( 0.2391304347826092025, 0.2463768115942035208, 0.2536231884057978392, 0.2608695652173921298 ),
 .UNSPECIFIED. ) 
 CURVE ( )  GEOMETRIC_REPRESENTATION_ITEM ( )  RATIONAL_B_SPLINE_CURVE ( ( 0.9999999999999907851, 0.8660254037844479225, 1.000000000000000000, 0.8660254037844387076, 1.000000000000000000, 0.8660254037844232755, 1.000000000000015321 ) ) 
 REPRESENTATION_ITEM ( '' )  );
#29880 = CIRCLE ( 'NONE', #8699, 6.000000000000001776 ) ;
#29881 = SHAPE_DEFINITION_REPRESENTATION ( #6236, #4527 ) ;
#29882 = CARTESIAN_POINT ( 'NONE',  ( -77.00000000000002842, 210.0000000000000000, 5.000000000000000000 ) ) ;
#29883 = CARTESIAN_POINT ( 'NONE',  ( -13.62178482187498396, 198.5281250006145228, 23.59362340125808188 ) ) ;
#29884 = CARTESIAN_POINT ( 'NONE',  ( 15.53471296425188797, 112.5773137178985479, 2.908627838312457747 ) ) ;
#29885 = CARTESIAN_POINT ( 'NONE',  ( -63.65252896937849414, 206.6499508600178387, -5.571401726697954970 ) ) ;
#29886 = VERTEX_POINT ( 'NONE', #1393 ) ;
#29887 = CARTESIAN_POINT ( 'NONE',  ( 12.50000000000000355, 35.71018628210144641, 0.1745138560725507937 ) ) ;
#29888 = DIRECTION ( 'NONE',  ( 0.000000000000000000, 0.000000000000000000, 1.000000000000000000 ) ) ;
#29889 = CYLINDRICAL_SURFACE ( 'NONE', #21127, 4.000000000000003553 ) ;
#29890 = CARTESIAN_POINT ( 'NONE',  ( 37.52407102436108488, 7.646167579472024665E-16, 167.2340683412427040 ) ) ;
#29891 = AXIS2_PLACEMENT_3D ( 'NONE', #367, #34677, #32020 ) ;
#29892 = CARTESIAN_POINT ( 'NONE',  ( 2.908627838312118019, 111.3226862821014578, 15.53471296425195369 ) ) ;
#29893 = CARTESIAN_POINT ( 'NONE',  ( -65.63913769728823411, 206.8500491399821044, -5.686928522499717253 ) ) ;
#29894 = CARTESIAN_POINT ( 'NONE',  ( 16.56230152254411081, -7.209453229046475009, -3.628124999385552663 ) ) ;
#29895 = CARTESIAN_POINT ( 'NONE',  ( -2.064181346179269738, 56.69768628210144357, 9.465287035748067623 ) ) ;
#29896 = LINE ( 'NONE', #35761, #1307 ) ;
#29897 = CARTESIAN_POINT ( 'NONE',  ( -31.99330436395490196, 210.1155267958016850, -8.500000000000003553 ) ) ;
#29898 = VECTOR ( 'NONE', #20771, 1000.000000000000000 ) ;
#29899 = CARTESIAN_POINT ( 'NONE',  ( 10.31873187879410736, -3.604726614523244610, -9.609374999385535077 ) ) ;
#29900 = CARTESIAN_POINT ( 'NONE',  ( 2.311890736173175753, 74.52268628210146062, 12.53471296425194836 ) ) ;
#29901 = FACE_OUTER_BOUND ( 'NONE', #20124, .T. ) ;
#29902 = CARTESIAN_POINT ( 'NONE',  ( 26.99999999999999645, 199.3625000000000114, -15.58845726811990495 ) ) ;
#29904 = DIRECTION ( 'NONE',  ( 0.000000000000000000, 0.000000000000000000, 1.000000000000000000 ) ) ;
#29903 = CARTESIAN_POINT ( 'NONE',  ( -2.064181346179269738, 47.49768628210145494, 9.465287035748067623 ) ) ;
#29905 = LINE ( 'NONE', #12659, #11283 ) ;
#29906 = CARTESIAN_POINT ( 'NONE',  ( 18.00000000000000355, -5.196152422706632912, -0.8249999999999924061 ) ) ;
#29907 = CARTESIAN_POINT ( 'NONE',  ( 20.99999999999999645, 185.0294372515228645, -5.999999999999999112 ) ) ;
#29908 = CARTESIAN_POINT ( 'NONE',  ( 27.94596069312478903, -5.407089921784865361, 165.2111578762278157 ) ) ;
#29909 = CARTESIAN_POINT ( 'NONE',  ( 24.93243976185750554, 0.000000000000000000, 163.7902716295174912 ) ) ;
#29910 = CARTESIAN_POINT ( 'NONE',  ( 26.99999999999999645, 245.2375000000000114, 3.464101615137751278 ) ) ;
#29911 = CARTESIAN_POINT ( 'NONE',  ( -13.62178482187500528, 196.1281250006145171, -23.59362340125807123 ) ) ;
#29912 = CARTESIAN_POINT ( 'NONE',  ( -12.50000000000000355, 98.48981371789855643, 0.1745138560722786503 ) ) ;
#29913 = CARTESIAN_POINT ( 'NONE',  ( 8.715434833791931624, 110.4601862821014606, 8.962234695871760692 ) ) ;
#29914 = ORIENTED_EDGE ( 'NONE', *, *, #33945, .F. ) ;
#29915 = ORIENTED_EDGE ( 'NONE', *, *, #9631, .F. ) ;
#29916 = CARTESIAN_POINT ( 'NONE',  ( -13.62178482187500528, 196.5781250006145342, -23.59362340125807123 ) ) ;
#29917 = CARTESIAN_POINT ( 'NONE',  ( -10.83675517735179028, 78.93981371789855928, 11.08355503943118947 ) ) ;
#29918 = CARTESIAN_POINT ( 'NONE',  ( 15.24356964374999990, 0.000000000000000000, -7.003124999385490490 ) ) ;
#29919 = CARTESIAN_POINT ( 'NONE',  ( 26.75643035624999655, 245.5468750006145342, 3.323476615752267715 ) ) ;
#29920 = PRODUCT_DEFINITION ( 'UNKNOWN', '', #8734, #31963 ) ;
#29921 = CARTESIAN_POINT ( 'NONE',  ( 5.529263428287477744, 98.67268628210146630, -7.954856959092191815 ) ) ;
#29922 =( BOUNDED_CURVE ( )  B_SPLINE_CURVE ( 2, ( #33629, #30788, #4811, #16391, #8589, #26578, #14281 ),
 .UNSPECIFIED., .F., .F. ) 
 B_SPLINE_CURVE_WITH_KNOTS ( ( 3, 2, 2, 3 ),
 ( 0.8958333333333333703, 0.9027777777777777901, 0.9166666666666666297, 0.9258785565094815873 ),
 .UNSPECIFIED. ) 
 CURVE ( )  GEOMETRIC_REPRESENTATION_ITEM ( )  RATIONAL_B_SPLINE_CURVE ( ( 0.9330127018922192983, 0.9330127018922198534, 1.000000000000000000, 0.8660254037844387076, 1.000000000000000000, 0.9111405360107182050, 0.9401542295229976531 ) ) 
 REPRESENTATION_ITEM ( '' )  );
#29923 = AXIS2_PLACEMENT_3D ( 'NONE', #2892, #32080, #17503 ) ;
#29924 = FACE_OUTER_BOUND ( 'NONE', #15887, .T. ) ;
#29925 = CARTESIAN_POINT ( 'NONE',  ( -9.465287035748106703, 52.20231371789854080, 2.064181346179061460 ) ) ;
#29926 = VECTOR ( 'NONE', #15848, 1000.000000000000000 ) ;
#29927 = CARTESIAN_POINT ( 'NONE',  ( 10.31873187879410736, 3.604726614523236616, -5.578124999385555505 ) ) ;
#29928 = ADVANCED_FACE ( 'NONE', ( #35319 ), #9374, .F. ) ;
#29929 = CARTESIAN_POINT ( 'NONE',  ( 5.529263428287300108, 113.7273137178985678, 7.954856959092309943 ) ) ;
#29930 = CARTESIAN_POINT ( 'NONE',  ( 27.00000000000001421, 197.9375000000000284, 15.58845726811988897 ) ) ;
#29931 = CARTESIAN_POINT ( 'NONE',  ( -12.53471296425189152, 25.17731371789855288, -2.311890736173453753 ) ) ;
#29932 = DIRECTION ( 'NONE',  ( 1.000000000000000000, 0.000000000000000000, 0.000000000000000000 ) ) ;
#29933 = CARTESIAN_POINT ( 'NONE',  ( -8.715434833791929847, 78.26018628210144357, -8.962234695871762469 ) ) ;
#29934 = CARTESIAN_POINT ( 'NONE',  ( 22.56230152254410370, 7.347880794884117764E-16, -6.412499998770998744 ) ) ;
#29935 = CARTESIAN_POINT ( 'NONE',  ( 0.5000000000000000000, 244.5000000000000000, 0.000000000000000000 ) ) ;
#29936 = CARTESIAN_POINT ( 'NONE',  ( 34.11184405356999605, 5.407089921784857367, 164.0505994570858093 ) ) ;
#29937 = CARTESIAN_POINT ( 'NONE',  ( 0.1745138560725837118, 79.41018628210144925, -15.50000000000000533 ) ) ;
#29938 = CARTESIAN_POINT ( 'NONE',  ( 10.31873187879410558, 3.604726614523240613, -3.384374999385492355 ) ) ;
#29939 = CARTESIAN_POINT ( 'NONE',  ( 1.120210788295102201E-13, 196.4000000012290741, -27.00000000000000711 ) ) ;
#29940 = CARTESIAN_POINT ( 'NONE',  ( 20.99999999999998579, 248.0875000000000057, -5.999999999999997335 ) ) ;
#29941 = CARTESIAN_POINT ( 'NONE',  ( 7.234628195640337545, 198.5174038105677141, -26.99999999999999289 ) ) ;
#29942 = CARTESIAN_POINT ( 'NONE',  ( 9.534712964251941258, 109.0226862821014606, -1.715153634034235708 ) ) ;
#29943 = CARTESIAN_POINT ( 'NONE',  ( 21.00000000000000000, 248.3687500012290741, 5.999999999999998224 ) ) ;
#29944 = CARTESIAN_POINT ( 'NONE',  ( 7.228626920339068285, 126.2726862821014606, -10.49813415415989581 ) ) ;
#29945 = CARTESIAN_POINT ( 'NONE',  ( -13.62178482187498396, 196.7843750006145456, 23.59362340125808188 ) ) ;
#29946 = CARTESIAN_POINT ( 'NONE',  ( 21.00000000000000000, 240.1843750006145513, -6.646953231504538984 ) ) ;
#29947 = VERTEX_POINT ( 'NONE', #15439 ) ;
#29948 = CARTESIAN_POINT ( 'NONE',  ( 37.36882485759182515, -3.604726614523235284, 165.4595965352667974 ) ) ;
#29949 = CARTESIAN_POINT ( 'NONE',  ( 15.24356964374999990, 3.323476615752268604, -2.878124999385485161 ) ) ;
#29950 = CARTESIAN_POINT ( 'NONE',  ( 0.000000000000000000, 143.0000000000000000, 0.000000000000000000 ) ) ;
#29951 = CARTESIAN_POINT ( 'NONE',  ( 25.04683167421347889, 3.464101615137573198, 165.0977771707629529 ) ) ;
#29952 = DIRECTION ( 'NONE',  ( 0.000000000000000000, 0.000000000000000000, 1.000000000000000000 ) ) ;
#29953 = CARTESIAN_POINT ( 'NONE',  ( 34.11717084844381986, -5.196152422706629359, 165.5088091249684510 ) ) ;
#29954 = CARTESIAN_POINT ( 'NONE',  ( 16.56230152254411436, 7.209453229046475009, -0.2531249993855048674 ) ) ;
#29955 = CARTESIAN_POINT ( 'NONE',  ( -3.796722387233185003, 17.41481371789854649, -8.710071997420207879 ) ) ;
#29956 = CARTESIAN_POINT ( 'NONE',  ( -13.62178482187500528, 197.5343750006145456, -23.59362340125807123 ) ) ;
#29958 = ORIENTED_EDGE ( 'NONE', *, *, #22810, .T. ) ;
#29957 = ORIENTED_EDGE ( 'NONE', *, *, #32309, .T. ) ;
#29959 = CARTESIAN_POINT ( 'NONE',  ( 23.87821517812500005, 245.8468750006145171, 4.985214923628404016 ) ) ;
#29960 = CARTESIAN_POINT ( 'NONE',  ( -8.962234695871565293, 16.83981371789855430, -8.715434833792128799 ) ) ;
#29961 = CARTESIAN_POINT ( 'NONE',  ( 21.00000000000000000, 6.646953231504538984, -2.053124999385488092 ) ) ;
#29962 = CARTESIAN_POINT ( 'NONE',  ( -15.50000000000000533, 126.0898137178985650, 0.1745138560722471477 ) ) ;
#29963 = CARTESIAN_POINT ( 'NONE',  ( 24.00000000000000000, -5.196152422706629359, -8.793749998770945098 ) ) ;
#29964 = CARTESIAN_POINT ( 'NONE',  ( 22.56230152254511268, 3.464101615137172629, -8.174999998770994480 ) ) ;
#29965 = ORIENTED_EDGE ( 'NONE', *, *, #21678, .F. ) ;
#29966 = CARTESIAN_POINT ( 'NONE',  ( 19.68408634441911431, 5.407089921784862696, -6.646874999385543603 ) ) ;
#29967 = CARTESIAN_POINT ( 'NONE',  ( -13.62178482187498396, 195.3781250006145171, 23.59362340125808188 ) ) ;
#29968 = CARTESIAN_POINT ( 'NONE',  ( 10.49813415415989581, 137.7726862821014606, 7.228626920339068285 ) ) ;
#29969 = CARTESIAN_POINT ( 'NONE',  ( 37.17435860658612512, 3.604726614523243278, 163.2368371151495694 ) ) ;
#29970 = CARTESIAN_POINT ( 'NONE',  ( -57.12127896937850124, 218.5309553116392465, 2.162041339862725842 ) ) ;
#29971 = CARTESIAN_POINT ( 'NONE',  ( 26.75643035624999655, 246.4093750006144887, -3.323476615752271268 ) ) ;
#29972 = CYLINDRICAL_SURFACE ( 'NONE', #21272, 6.000000000000001776 ) ;
#29973 = CARTESIAN_POINT ( 'NONE',  ( -45.04836230271183695, 206.0451222850691977, -2.149950860017851184 ) ) ;
#29974 = CARTESIAN_POINT ( 'NONE',  ( 2.311890736173175753, 129.7226862821014777, 12.53471296425194836 ) ) ;
#29975 = CARTESIAN_POINT ( 'NONE',  ( 28.05545009495152087, 5.407089921784856479, 166.4626274657055660 ) ) ;
#29976 = ORIENTED_EDGE ( 'NONE', *, *, #1831, .F. ) ;
#29977 = VECTOR ( 'NONE', #12884, 1000.000000000000000 ) ;
#29978 = CARTESIAN_POINT ( 'NONE',  ( -28.29648172771258885, 205.1140383288905298, 6.355902910654599225 ) ) ;
#29979 = CARTESIAN_POINT ( 'NONE',  ( -13.04141134922759804, 133.1726862821014663, -8.927990412390657937 ) ) ;
#29980 = CARTESIAN_POINT ( 'NONE',  ( -46.24330436395489841, 210.1155267958016850, -8.500000000000003553 ) ) ;
#29981 = CARTESIAN_POINT ( 'NONE',  ( -2.064181346179269738, 130.2976862821014379, 9.465287035748067623 ) ) ;
#29982 = LINE ( 'NONE', #27140, #17637 ) ;
#29983 = CARTESIAN_POINT ( 'NONE',  ( -12.46528703574805697, 31.39768628210144641, -2.660918448318280838 ) ) ;
#29984 = EDGE_CURVE ( 'NONE', #8243, #28841, #31105, .T. ) ;
#29985 = CARTESIAN_POINT ( 'NONE',  ( 22.56230152254412502, -3.464101615137755275, -6.562500000000047073 ) ) ;
#29986 = SHAPE_REPRESENTATION ( 'extension pipe', ( #17215 ), #34722 ) ;
#29987 = ORIENTED_EDGE ( 'NONE', *, *, #22220, .F. ) ;
#29988 = CARTESIAN_POINT ( 'NONE',  ( -36.34747103062156981, 213.3500491399821328, -5.571401726697985168 ) ) ;
#29989 = CARTESIAN_POINT ( 'NONE',  ( 0.1745138560725837118, 116.2101862821014748, -15.50000000000000533 ) ) ;
#29990 = DIRECTION ( 'NONE',  ( 0.5887012860850814322, -0.8083506638592999893, 0.000000000000000000 ) ) ;
#29991 = CARTESIAN_POINT ( 'NONE',  ( -5.529263428287297444, 136.7273137178985110, -7.954856959092311719 ) ) ;
#29992 = CARTESIAN_POINT ( 'NONE',  ( -27.24356964374999990, 199.3156250006145171, -15.72908226750537786 ) ) ;
#29993 = FACE_OUTER_BOUND ( 'NONE', #26381, .T. ) ;
#29994 = CARTESIAN_POINT ( 'NONE',  ( 27.00000000000001066, 195.2375000000000114, 15.58845726811988897 ) ) ;
#29995 = CARTESIAN_POINT ( 'NONE',  ( 15.00000000000000000, 0.000000000000000000, -0.9000000000000119016 ) ) ;
#29996 = CARTESIAN_POINT ( 'NONE',  ( 16.07423293023537525, 3.170634016558939727, -7.999999999999998224 ) ) ;
#29997 = CARTESIAN_POINT ( 'NONE',  ( 36.71355410024671784, 3.464101615138219348, 160.7644657540884054 ) ) ;
#29998 = CARTESIAN_POINT ( 'NONE',  ( 0.1745138560723095977, 77.78981371789853938, 9.500000000000005329 ) ) ;
#29999 = CARTESIAN_POINT ( 'NONE',  ( 10.49999999999999645, 244.5000000000000000, -5.000000000000000000 ) ) ;
#30000 = EDGE_LOOP ( 'NONE', ( #13841, #36338, #11901, #33272 ) ) ;
#30001 = AXIS2_PLACEMENT_3D ( 'NONE', #31949, #2766, #14338 ) ;
#30002 = CARTESIAN_POINT ( 'NONE',  ( 26.99999999999999645, 244.0187500012290513, -3.464101615137755275 ) ) ;
#30003 = CARTESIAN_POINT ( 'NONE',  ( 12.50000000000000355, 84.68981371789854506, -0.1745138560722771515 ) ) ;
#30004 = CARTESIAN_POINT ( 'NONE',  ( 22.80587116629412847, 3.604726614523243278, -3.984374999385507987 ) ) ;
#30005 = CARTESIAN_POINT ( 'NONE',  ( 15.24356964375000167, -3.323476615752272600, -4.265624999385501326 ) ) ;
#30006 = CARTESIAN_POINT ( 'NONE',  ( 6.932735513424201024, 46.45231371789855501, -10.69584247140429412 ) ) ;
#30007 = CIRCLE ( 'NONE', #34256, 2.649999999999992806 ) ;
#30008 = ORIENTED_EDGE ( 'NONE', *, *, #27045, .T. ) ;
#30009 = CARTESIAN_POINT ( 'NONE',  ( 18.12178482187500350, -4.985214923628407568, -7.265624999385461358 ) ) ;
#30010 = CARTESIAN_POINT ( 'NONE',  ( 18.12178482187499640, 244.7218750006145171, -4.985214923628404904 ) ) ;
#30011 = EDGE_CURVE ( 'NONE', #34698, #17773, #15576, .T. ) ;
#30012 = CARTESIAN_POINT ( 'NONE',  ( -12.53471296425194836, 30.82268628210144001, 2.311890736173176641 ) ) ;
#30013 = CARTESIAN_POINT ( 'NONE',  ( -36.73586230271183695, 206.8500491399821328, 5.686928522499748340 ) ) ;
#30014 = CARTESIAN_POINT ( 'NONE',  ( -49.40252896937850124, 206.6499508600178387, -5.571401726697954970 ) ) ;
#30015 = SHAPE_REPRESENTATION_RELATIONSHIP ( 'NONE' , 'NONE' ,  #4527, #14238 ) ;
#30016 = CARTESIAN_POINT ( 'NONE',  ( 33.56808966913361303, -5.196152422706629359, 159.2327825269904622 ) ) ;
#30017 = CARTESIAN_POINT ( 'NONE',  ( -12.53471296425189152, 89.57731371789856212, -2.311890736173453753 ) ) ;
#30018 = CARTESIAN_POINT ( 'NONE',  ( -46.83705436395489130, 206.7903428501026042, -3.378800118222489157 ) ) ;
#30019 = CARTESIAN_POINT ( 'NONE',  ( -67.22247103062156270, 206.6499508600178672, 5.571401726697986057 ) ) ;
#30020 = CARTESIAN_POINT ( 'NONE',  ( 15.24356964375000167, -3.323476615752272600, -6.065624999385484273 ) ) ;
#30021 = DIRECTION ( 'NONE',  ( 1.000000000000000000, 0.000000000000000000, 0.000000000000000000 ) ) ;
#30022 = CARTESIAN_POINT ( 'NONE',  ( -14.25334919248795096, 51.91481371789856070, 6.092822981423662299 ) ) ;
#30023 = CARTESIAN_POINT ( 'NONE',  ( -47.02752896937850835, 214.3500491399821897, 7.303452534266821949 ) ) ;
#30024 = DIRECTION ( 'NONE',  ( 0.9961946980917462113, 0.000000000000000000, -0.08715574274765118534 ) ) ;
#30025 = CARTESIAN_POINT ( 'NONE',  ( 2.311890736173175753, 83.72268628210143504, 12.53471296425194836 ) ) ;
#30026 = CARTESIAN_POINT ( 'NONE',  ( -2.908627838312119351, 23.92268628210143788, -15.53471296425195369 ) ) ;
#30027 = CARTESIAN_POINT ( 'NONE',  ( -47.00000000000000711, 252.0000000000000000, 5.000000000000000000 ) ) ;
#30028 = CARTESIAN_POINT ( 'NONE',  ( 30.66693367924855096, -7.209453229046482114, 160.4935575611445415 ) ) ;
#30029 = ORIENTED_EDGE ( 'NONE', *, *, #8012, .F. ) ;
#30030 = CARTESIAN_POINT ( 'NONE',  ( 8.927990412390657937, 52.67268628210144499, -13.04141134922759804 ) ) ;
#30031 = CARTESIAN_POINT ( 'NONE',  ( -27.24356964374999279, 198.4906250006145569, 15.72908226750539384 ) ) ;
#30032 = CARTESIAN_POINT ( 'NONE',  ( 27.24356964375000345, 199.6343750006145399, -3.336375036156643733E-15 ) ) ;
#30033 = CARTESIAN_POINT ( 'NONE',  ( 20.99999999999999645, 185.0294372515228645, 0.000000000000000000 ) ) ;
#30034 = CARTESIAN_POINT ( 'NONE',  ( -41.49330436395490551, 210.1155267958017134, -6.500000000000000888 ) ) ;
#30035 = CARTESIAN_POINT ( 'NONE',  ( 10.56230152254470056, 3.464101615138089674, -7.574999998771039245 ) ) ;
#30036 = CARTESIAN_POINT ( 'NONE',  ( 4.622313124798573369, 19.03518628210144925, 11.61527771782819940 ) ) ;
#30037 = CARTESIAN_POINT ( 'NONE',  ( 23.87821517812499650, 249.7093750006145285, -4.985214923628404904 ) ) ;
#30038 = CARTESIAN_POINT ( 'NONE',  ( -2.064181346179062349, 137.3023137178985564, -9.465287035748106703 ) ) ;
#30039 = CARTESIAN_POINT ( 'NONE',  ( 26.75643035624999655, 245.1718750006145058, -3.323476615752271268 ) ) ;
#30040 = ORIENTED_EDGE ( 'NONE', *, *, #7960, .T. ) ;
#30041 = CARTESIAN_POINT ( 'NONE',  ( 15.00000000000000178, -3.464101615137757051, -7.612499999999993605 ) ) ;
#30042 = CARTESIAN_POINT ( 'NONE',  ( 19.39230484541324628, 245.0138461906613543, -5.999999999999989342 ) ) ;
#30043 = VECTOR ( 'NONE', #16519, 1000.000000000000000 ) ;
#30044 = CARTESIAN_POINT ( 'NONE',  ( 7.228626920338837358, 132.1273137178985451, 10.49813415416005036 ) ) ;
#30045 = CARTESIAN_POINT ( 'NONE',  ( 10.31873187879411446, 3.604726614523236616, -6.928124999385510741 ) ) ;
#30046 = CARTESIAN_POINT ( 'NONE',  ( 34.19028422204287665, 5.407089921784857367, 164.9471746853683669 ) ) ;
#30047 = DIRECTION ( 'NONE',  ( 2.168404344971009176E-17, 0.000000000000000000, 1.000000000000000000 ) ) ;
#30048 = CARTESIAN_POINT ( 'NONE',  ( -26.99999999999998934, 199.5874999999999773, 15.58845726811991561 ) ) ;
#30049 = EDGE_LOOP ( 'NONE', ( #14248, #35646, #35059, #26407 ) ) ;
#30050 = CARTESIAN_POINT ( 'NONE',  ( -4.622313124798576922, 51.23518628210143788, -11.61527771782819762 ) ) ;
#30051 = ORIENTED_EDGE ( 'NONE', *, *, #29509, .F. ) ;
#30052 = ORIENTED_EDGE ( 'NONE', *, *, #17924, .T. ) ;
#30053 = CARTESIAN_POINT ( 'NONE',  ( 6.500000000000000888, 244.5000000000000000, -11.00000000000000000 ) ) ;
#30054 = CARTESIAN_POINT ( 'NONE',  ( 20.99999999999999645, 6.646953231504538984, -1.153124999385464200 ) ) ;
#30055 = CARTESIAN_POINT ( 'NONE',  ( 26.99999999999999645, 7.347880794884117764E-16, -1.124999999999987121 ) ) ;
#30056 = CARTESIAN_POINT ( 'NONE',  ( 22.60769515458671108, 242.9325961894323029, 6.000000000000010658 ) ) ;
#30057 = CARTESIAN_POINT ( 'NONE',  ( 15.24356964374999990, 3.323476615752268604, -7.828124999385470240 ) ) ;
#30058 = CARTESIAN_POINT ( 'NONE',  ( 4.622313124798573369, 74.23518628210145209, 11.61527771782819940 ) ) ;
#30059 = CARTESIAN_POINT ( 'NONE',  ( -15.46528703574811736, 15.40231371789854720, 3.257655550456946436 ) ) ;
#30060 = CARTESIAN_POINT ( 'NONE',  ( 22.56230152254410370, 7.347880794884117764E-16, -3.712499998771018106 ) ) ;
#30061 = CARTESIAN_POINT ( 'NONE',  ( 24.86053627419733658, 3.464101615137476831, 162.9684110048161756 ) ) ;
#30062 = CARTESIAN_POINT ( 'NONE',  ( -36.74330436395489130, 210.1155267958017703, -4.499999999999996447 ) ) ;
#30063 = CARTESIAN_POINT ( 'NONE',  ( 21.00000000000000355, 0.000000000000000000, 50.00000000000001421 ) ) ;
#30064 = CARTESIAN_POINT ( 'NONE',  ( 37.22995187613445012, 7.347880794884117764E-16, 166.6669193415062580 ) ) ;
#30065 = CARTESIAN_POINT ( 'NONE',  ( -12.53471296425189152, 135.5773137178985621, -2.311890736173453753 ) ) ;
#30066 = CARTESIAN_POINT ( 'NONE',  ( -49.01413769728823411, 213.1499508600178672, 5.686928522499718142 ) ) ;
#30067 = CARTESIAN_POINT ( 'NONE',  ( -64.64955436395490551, 216.3070033484980002, -6.137860380172975638 ) ) ;
#30068 = APPLICATION_PROTOCOL_DEFINITION ( 'draft international standard', 'automotive_design', 1998, #1567 ) ;
#30069 = CARTESIAN_POINT ( 'NONE',  ( 29.51984097383938987, 5.908847061326898853, 159.3365289693693398 ) ) ;
#30070 = CARTESIAN_POINT ( 'NONE',  ( 27.24356964375000345, 197.7781250006145228, -3.336375036156643733E-15 ) ) ;
#30071 = CARTESIAN_POINT ( 'NONE',  ( 10.83675517735179206, 120.3398137178985507, -11.08355503943118769 ) ) ;
#30072 = CARTESIAN_POINT ( 'NONE',  ( -39.30877896937850124, 211.6261429550004607, -6.530955311639245586 ) ) ;
#30073 = AXIS2_PLACEMENT_3D ( 'NONE', #28255, #13861, #31287 ) ;
#30074 = VERTEX_POINT ( 'NONE', #35697 ) ;
#30075 = CARTESIAN_POINT ( 'NONE',  ( 6.932735513423970097, 27.94768628210143646, 10.69584247140445044 ) ) ;
#30076 = LINE ( 'NONE', #15683, #29228 ) ;
#30077 = CARTESIAN_POINT ( 'NONE',  ( 22.56230152254411792, 7.347880794884125653E-16, -6.975000000000036948 ) ) ;
#30078 = CARTESIAN_POINT ( 'NONE',  ( 34.26382187998621731, 5.407089921784862696, 165.7877139618832985 ) ) ;
#30079 = CARTESIAN_POINT ( 'NONE',  ( 0.1745138560725837118, 107.0101862821014578, -15.50000000000000533 ) ) ;
#30080 = CARTESIAN_POINT ( 'NONE',  ( -54.15997103062156981, 215.5714017266979852, 3.350049139982118618 ) ) ;
#30081 = EDGE_CURVE ( 'NONE', #14162, #24412, #21697, .T. ) ;
#30082 = CARTESIAN_POINT ( 'NONE',  ( 22.80587116629410716, 7.646167579472015790E-16, -3.515624999385541294 ) ) ;
#30083 =( BOUNDED_CURVE ( )  B_SPLINE_CURVE ( 2, ( #30764, #19777, #5520, #27909, #25256, #36619, #2127, #8385, #1939, #25807, #28094, #17104, #13890, #25438, #22791, #33790, #16920, #37178, #36991, #5342, #28644, #16733, #28461, #11034, #14071, #2497, #13704, #25620, #22608, #34154, #11219, #28279, #34339, #19955, #8200, #2681, #31313, #25065, #10661, #14256, #4968, #19404, #37354, #36806, #11407, #16550, #22977, #30950, #34526, #8566, #10848, #4787, #13509, #22240, #16360, #7828, #22421, #33970, #8010, #19585, #2318, #31135, #5152, #14998, #20324, #6279, #28830, #32239, #26738, #26176, #29202, #32051, #23164, #14438, #26360, #9128, #6081, #2865, #29011, #3055, #12147, #17855, #26551, #771, #20887, #9317, #20133, #20694, #32428, #17288, #14625, #25992, #213, #35262, #22, #15190, #17478, #6473, #3244, #14817, #23723, #578, #29395, #8752, #11588, #3430, #18042, #17666, #29585, #396, #3623, #12340, #11778, #23914, #11963, #23532, #35455, #35078, #31679, #5709, #34705, #5898, #31864, #23344, #34896, #8936, #20513, #35645, #10060, #6844, #33187, #21268, #36020, #13282, #7047, #12535, #24099, #30541, #13096, #7230, #18615, #1149, #18983, #24651, #21455, #29772, #1712, #1339, #26930, #4558, #16133, #15568, #27124, #12909, #24837, #24474, #21822, #21635, #36202, #18803, #9873, #10246, #15948, #3804, #32995, #32806, #3994, #18422, #18232, #9690, #32618, #30157, #29966, #27685, #960, #30345, #4370, #33374, #27502, #15381, #4186, #12719, #1523, #7412, #9505, #21081, #6656, #24288, #15758, #35833, #27309, #22564, #7599, #4746, #5116, #33930, #33562, #14030, #2457, #1899, #13663, #27866, #22381, #25397, #13469, #28243, #19174, #16695, #25581, #7786, #25215, #2089, #16318, #30723, #7971, #31094, #28054, #25021, #10619, #22198, #34111, #19737, #2272, #8163, #37134, #31275, #36766, #28417, #5301, #13850, #16881, #36578, #36947, #10993, #11179, #30904, #33746, #36389, #10435, #10809, #19364, #4925, #22008, #16507, #19545, #7348, #33489, #4493, #1649, #24218, #4673, #29899, #16070, #13221, #18736, #36140, #35763, #10181, #27057, #6978, #30277, #18921, #1460 ),
 .UNSPECIFIED., .F., .F. ) 
 B_SPLINE_CURVE_WITH_KNOTS ( ( 3, 2, 2, 2, 2, 2, 2, 2, 2, 2, 2, 2, 2, 2, 2, 2, 2, 2, 2, 2, 2, 2, 2, 2, 2, 2, 2, 2, 2, 2, 2, 2, 2, 2, 2, 2, 2, 2, 2, 2, 2, 2, 2, 2, 2, 2, 2, 2, 2, 2, 2, 2, 2, 2, 2, 2, 2, 2, 2, 2, 2, 2, 2, 2, 2, 2, 2, 2, 2, 2, 2, 2, 2, 2, 2, 2, 2, 2, 2, 2, 2, 2, 2, 2, 2, 2, 2, 2, 2, 2, 2, 2, 2, 2, 2, 2, 2, 2, 2, 2, 2, 2, 2, 2, 2, 2, 2, 2, 2, 2, 2, 2, 2, 2, 2, 2, 2, 2, 2, 2, 2, 2, 2, 2, 2, 2, 2, 2, 2, 2, 2, 3 ),
 ( 0.000000000000000000, 0.007246376811594202987, 0.01449275362318840597, 0.02173913043478260809, 0.02898550724637681195, 0.03623188405797101580, 0.04347826086956521618, 0.05072463768115942351, 0.05797101449275362389, 0.06521739130434782428, 0.07246376811594203160, 0.07971014492753622505, 0.08695652173913043237, 0.09420289855072463969, 0.1014492753623188470, 0.1086956521739130405, 0.1159420289855072478, 0.1231884057971014551, 0.1304347826086956486, 0.1376811594202898559, 0.1449275362318840632, 0.1521739130434782705, 0.1594202898550724501, 0.1666666666666666574, 0.1739130434782608647, 0.1811594202898550721, 0.1884057971014492794, 0.1956521739130434867, 0.2028985507246376940, 0.2101449275362318736, 0.2173913043478260809, 0.2246376811594202882, 0.2318840579710144956, 0.2391304347826087029, 0.2463768115942029102, 0.2536231884057971175, 0.2608695652173912971, 0.2681159420289855322, 0.2753623188405797118, 0.2826086956521738358, 0.2898550724637681264, 0.2971014492753623060, 0.3043478260869565410, 0.3115942028985507206, 0.3188405797101449002, 0.3260869565217391353, 0.3333333333333333148, 0.3405797101449275499, 0.3478260869565217295, 0.3550724637681159646, 0.3623188405797101441, 0.3695652173913043237, 0.3768115942028985588, 0.3840579710144927383, 0.3913043478260869734, 0.3985507246376811530, 0.4057971014492753881, 0.4130434782608695676, 0.4202898550724637472, 0.4275362318840579268, 0.4347826086956521618, 0.4420289855072463969, 0.4492753623188405765, 0.4565217391304347561, 0.4637681159420289911, 0.4710144927536231707, 0.4782608695652174058, 0.4855072463768115854, 0.4927536231884058204, 0.5000000000000000000, 0.5072463768115942351, 0.5144927536231883591, 0.5217391304347825942, 0.5289855072463768293, 0.5362318840579710644, 0.5434782608695651884, 0.5507246376811594235, 0.5579710144927536586, 0.5652173913043476716, 0.5724637681159420177, 0.5797101449275362528, 0.5869565217391304879, 0.5942028985507246119, 0.6014492753623188470, 0.6086956521739130821, 0.6159420289855072062, 0.6231884057971014412, 0.6304347826086956763, 0.6376811594202898004, 0.6449275362318841465, 0.6521739130434782705, 0.6594202898550725056, 0.6666666666666666297, 0.6739130434782608647, 0.6811594202898550998, 0.6884057971014492239, 0.6956521739130434590, 0.7028985507246376940, 0.7101449275362319291, 0.7173913043478260532, 0.7246376811594202882, 0.7318840579710145233, 0.7391304347826086474, 0.7463768115942028825, 0.7536231884057971175, 0.7608695652173913526, 0.7681159420289854767, 0.7753623188405797118, 0.7826086956521739468, 0.7898550724637680709, 0.7971014492753623060, 0.8043478260869565410, 0.8115942028985507761, 0.8188405797101449002, 0.8260869565217391353, 0.8333333333333333703, 0.8405797101449274944, 0.8478260869565217295, 0.8550724637681158535, 0.8623188405797101996, 0.8695652173913043237, 0.8768115942028985588, 0.8840579710144927938, 0.8913043478260869179, 0.8985507246376811530, 0.9057971014492753881, 0.9130434782608695121, 0.9202898550724637472, 0.9275362318840579823, 0.9347826086956523284, 0.9420289855072463414, 0.9470763321615516261 ),
 .UNSPECIFIED. ) 
 CURVE ( )  GEOMETRIC_REPRESENTATION_ITEM ( )  RATIONAL_B_SPLINE_CURVE ( ( 1.000000000000000000, 0.8660254037844387076, 1.000000000000000000, 0.8660254037844387076, 1.000000000000000000, 0.8660254037844387076, 1.000000000000000000, 0.8660254037844387076, 1.000000000000000000, 0.8660254037844387076, 1.000000000000000000, 0.8660254037844387076, 1.000000000000000000, 0.8660254037844387076, 1.000000000000000000, 0.8660254037844387076, 1.000000000000000000, 0.8660254037844387076, 1.000000000000000000, 0.8660254037844387076, 1.000000000000000000, 0.8660254037844387076, 1.000000000000000000, 0.8660254037844387076, 1.000000000000000000, 0.8660254037844387076, 1.000000000000000000, 0.8660254037844387076, 1.000000000000000000, 0.8660254037844387076, 1.000000000000000000, 0.8660254037844387076, 1.000000000000000000, 0.8660254037844387076, 1.000000000000000000, 0.8660254037844387076, 1.000000000000000000, 0.8660254037844387076, 1.000000000000000000, 0.8660254037844387076, 1.000000000000000000, 0.8660254037844387076, 1.000000000000000000, 0.8660254037844387076, 1.000000000000000000, 0.8660254037844387076, 1.000000000000000000, 0.8660254037844387076, 1.000000000000000000, 0.8660254037844387076, 1.000000000000000000, 0.8660254037844387076, 1.000000000000000000, 0.8660254037844387076, 1.000000000000000000, 0.8660254037844387076, 1.000000000000000000, 0.8660254037844387076, 1.000000000000000000, 0.8660254037844387076, 1.000000000000000000, 0.8660254037844387076, 1.000000000000000000, 0.8660254037844387076, 1.000000000000000000, 0.8660254037844387076, 1.000000000000000000, 0.8660254037844387076, 1.000000000000000000, 0.8660254037844387076, 1.000000000000000000, 0.8660254037844387076, 1.000000000000000000, 0.8660254037844387076, 1.000000000000000000, 0.8660254037844387076, 1.000000000000000000, 0.8660254037844387076, 1.000000000000000000, 0.8660254037844387076, 1.000000000000000000, 0.8660254037844387076, 1.000000000000000000, 0.8660254037844387076, 1.000000000000000000, 0.8660254037844387076, 1.000000000000000000, 0.8660254037844387076, 1.000000000000000000, 0.8660254037844387076, 1.000000000000000000, 0.8660254037844387076, 1.000000000000000000, 0.8660254037844387076, 1.000000000000000000, 0.8660254037844387076, 1.000000000000000000, 0.8660254037844387076, 1.000000000000000000, 0.8660254037844387076, 1.000000000000000000, 0.8660254037844387076, 1.000000000000000000, 0.8660254037844387076, 1.000000000000000000, 0.8660254037844387076, 1.000000000000000000, 0.8660254037844387076, 1.000000000000000000, 0.8660254037844387076, 1.000000000000000000, 0.8660254037844387076, 1.000000000000000000, 0.8660254037844387076, 1.000000000000000000, 0.8660254037844387076, 1.000000000000000000, 0.8660254037844387076, 1.000000000000000000, 0.8660254037844387076, 1.000000000000000000, 0.8660254037844387076, 1.000000000000000000, 0.8660254037844387076, 1.000000000000000000, 0.8660254037844387076, 1.000000000000000000, 0.8660254037844387076, 1.000000000000000000, 0.8660254037844387076, 1.000000000000000000, 0.8660254037844387076, 1.000000000000000000, 0.8660254037844387076, 1.000000000000000000, 0.8660254037844387076, 1.000000000000000000, 0.8660254037844387076, 1.000000000000000000, 0.8660254037844387076, 1.000000000000000000, 0.8660254037844387076, 1.000000000000000000, 0.8660254037844387076, 1.000000000000000000, 0.8660254037844387076, 1.000000000000000000, 0.8660254037844387076, 1.000000000000000000, 0.8660254037844387076, 1.000000000000000000, 0.8660254037844387076, 1.000000000000000000, 0.8660254037844387076, 1.000000000000000000, 0.8660254037844387076, 1.000000000000000000, 0.8660254037844387076, 1.000000000000000000, 0.8660254037844387076, 1.000000000000000000, 0.8660254037844387076, 1.000000000000000000, 0.8660254037844387076, 1.000000000000000000, 0.8660254037844387076, 1.000000000000000000, 0.8660254037844387076, 1.000000000000000000, 0.8660254037844387076, 1.000000000000000000, 0.8660254037844387076, 1.000000000000000000, 0.8660254037844387076, 1.000000000000000000, 0.8660254037844387076, 1.000000000000000000, 0.8660254037844387076, 1.000000000000000000, 0.8660254037844387076, 1.000000000000000000, 0.8660254037844387076, 1.000000000000000000, 0.8660254037844387076, 1.000000000000000000, 0.8660254037844387076, 1.000000000000000000, 0.8660254037844387076, 1.000000000000000000, 0.8660254037844387076, 1.000000000000000000, 0.8660254037844387076, 1.000000000000000000, 0.8660254037844387076, 1.000000000000000000, 0.8660254037844387076, 1.000000000000000000, 0.8660254037844387076, 1.000000000000000000, 0.8660254037844387076, 1.000000000000000000, 0.8660254037844387076, 1.000000000000000000, 0.8660254037844387076, 1.000000000000000000, 0.8660254037844387076, 1.000000000000000000, 0.8660254037844387076, 1.000000000000000000, 0.8660254037844387076, 1.000000000000000000, 0.8660254037844387076, 1.000000000000000000, 0.8660254037844387076, 1.000000000000000000, 0.8660254037844387076, 1.000000000000000000, 0.8660254037844387076, 1.000000000000000000, 0.8660254037844387076, 1.000000000000000000, 0.8660254037844387076, 1.000000000000000000, 0.8660254037844387076, 1.000000000000000000, 0.8660254037844387076, 1.000000000000000000, 0.8660254037844387076, 1.000000000000000000, 0.8660254037844387076, 1.000000000000000000, 0.8660254037844387076, 1.000000000000000000, 0.8660254037844387076, 1.000000000000000000, 0.8660254037844387076, 1.000000000000000000, 0.8660254037844387076, 1.000000000000000000, 0.8660254037844387076, 1.000000000000000000, 0.8660254037844387076, 1.000000000000000000, 0.8660254037844387076, 1.000000000000000000, 0.8660254037844387076, 1.000000000000000000, 0.8660254037844387076, 1.000000000000000000, 0.8660254037844387076, 1.000000000000000000, 0.8660254037844387076, 1.000000000000000000, 0.8660254037844387076, 1.000000000000000000, 0.8660254037844387076, 1.000000000000000000, 0.8660254037844387076, 1.000000000000000000, 0.8660254037844387076, 1.000000000000000000, 0.9066821602640693367, 0.9433623867133065222 ) ) 
 REPRESENTATION_ITEM ( '' )  );
#30084 = CARTESIAN_POINT ( 'NONE',  ( -9.534712964251941258, 40.02268628210144641, 1.715153634034234154 ) ) ;
#30085 = CARTESIAN_POINT ( 'NONE',  ( -77.00000000000002842, 210.0000000000000000, 2.500000000000001332 ) ) ;
#30086 = CARTESIAN_POINT ( 'NONE',  ( -69.59747103062156270, 213.3500491399821328, -5.571401726697985168 ) ) ;
#30087 = ADVANCED_FACE ( 'NONE', ( #12588 ), #4051, .F. ) ;
#30088 = DIRECTION ( 'NONE',  ( 0.000000000000000000, 0.000000000000000000, -1.000000000000000000 ) ) ;
#30089 = CARTESIAN_POINT ( 'NONE',  ( 6.932735513423970097, 73.94768628210145778, 10.69584247140445044 ) ) ;
#30090 = DIRECTION ( 'NONE',  ( 0.000000000000000000, 1.000000000000000000, 0.000000000000000000 ) ) ;
#30091 = CARTESIAN_POINT ( 'NONE',  ( 26.99999999999999645, 247.5812500012290513, -7.347880794884117764E-16 ) ) ;
#30093 = ORIENTED_EDGE ( 'NONE', *, *, #29738, .T. ) ;
#30092 = CARTESIAN_POINT ( 'NONE',  ( 5.529263428287477744, 52.67268628210144499, -7.954856959092191815 ) ) ;
#30094 = CARTESIAN_POINT ( 'NONE',  ( 24.44222019244867283, 0.000000000000000000, 160.9816845590745800 ) ) ;
#30095 = EDGE_LOOP ( 'NONE', ( #36837, #17559, #1613, #25734 ) ) ;
#30096 = CARTESIAN_POINT ( 'NONE',  ( 18.00000000000000000, 5.196152422706630247, -0.07499999999999173994 ) ) ;
#30097 = VECTOR ( 'NONE', #10309, 1000.000000000000000 ) ;
#30098 = CARTESIAN_POINT ( 'NONE',  ( 31.21356360324042356, 6.928203230275514990, 166.7415661826265421 ) ) ;
#30099 = CARTESIAN_POINT ( 'NONE',  ( 37.16782192588006239, -3.604726614523238837, 163.1621225127927062 ) ) ;
#30100 = CARTESIAN_POINT ( 'NONE',  ( 36.78545758801433152, -3.464101615137755275, 161.5863263800139862 ) ) ;
#30101 = CARTESIAN_POINT ( 'NONE',  ( 26.99999999999999645, 246.6250000000000000, -7.347880794884117764E-16 ) ) ;
#30102 = CARTESIAN_POINT ( 'NONE',  ( -27.24356964375000345, 195.2656250006145342, -15.72908226750537786 ) ) ;
#30103 = ADVANCED_FACE ( 'NONE', ( #3489 ), #23971, .F. ) ;
#30104 = CARTESIAN_POINT ( 'NONE',  ( 2.660918448318002838, 105.1023137178985536, 12.46528703574811558 ) ) ;
#30105 = CARTESIAN_POINT ( 'NONE',  ( 2.660918448318279950, 107.2976862821014521, -12.46528703574805874 ) ) ;
#30106 = ORIENTED_EDGE ( 'NONE', *, *, #12616, .F. ) ;
#30107 = ORIENTED_EDGE ( 'NONE', *, *, #9772, .T. ) ;
#30108 = CARTESIAN_POINT ( 'NONE',  ( -13.62178482187500528, 196.1281250006145171, -23.59362340125807123 ) ) ;
#30109 = CARTESIAN_POINT ( 'NONE',  ( 22.56230152254257604, -3.464101615138639900, -9.149999998771018994 ) ) ;
#30110 = AXIS2_PLACEMENT_3D ( 'NONE', #35885, #20948, #9185 ) ;
#30111 = CARTESIAN_POINT ( 'NONE',  ( 13.04141134922778988, 83.82731371789856212, -8.927990412390371944 ) ) ;
#30112 = CARTESIAN_POINT ( 'NONE',  ( 18.12178482187499640, 4.985214923628404904, -6.628124999385476279 ) ) ;
#30113 = CARTESIAN_POINT ( 'NONE',  ( 18.12178482187500350, 244.9843750006145342, 4.985214923628407568 ) ) ;
#30114 =( BOUNDED_CURVE ( )  B_SPLINE_CURVE ( 2, ( #35461, #9322, #778, #5902, #35083, #32058, #9135, #14822, #401 ),
 .UNSPECIFIED., .F., .F. ) 
 B_SPLINE_CURVE_WITH_KNOTS ( ( 3, 2, 2, 2, 3 ),
 ( 0.3804347826086956763, 0.3840579710144927383, 0.3913043478260869734, 0.3985507246376811530, 0.4021739130434782705 ),
 .UNSPECIFIED. ) 
 CURVE ( )  GEOMETRIC_REPRESENTATION_ITEM ( )  RATIONAL_B_SPLINE_CURVE ( ( 0.9330127018922194093, 0.9330127018922198534, 1.000000000000000000, 0.8660254037844387076, 1.000000000000000000, 0.8660254037844387076, 1.000000000000000000, 0.9330127018922194093, 0.9330127018922194093 ) ) 
 REPRESENTATION_ITEM ( '' )  );
#30115 = CARTESIAN_POINT ( 'NONE',  ( -6.594114490232312775, 96.66018628210144925, -6.840914352312096547 ) ) ;
#30116 = DIRECTION ( 'NONE',  ( -0.000000000000000000, 1.000000000000000000, 0.000000000000000000 ) ) ;
#30117 = CARTESIAN_POINT ( 'NONE',  ( -9.534712964251895073, 52.77731371789855785, -1.715153634034446428 ) ) ;
#30118 = CARTESIAN_POINT ( 'NONE',  ( 16.56230152254411436, -7.209453229046475009, -7.228124999385518556 ) ) ;
#30119 = CARTESIAN_POINT ( 'NONE',  ( 9.500000000000005329, 112.2898137178985678, -0.1745138560723090149 ) ) ;
#30120 = CARTESIAN_POINT ( 'NONE',  ( 20.99999999999999645, 240.4093750006145171, 6.646953231504538984 ) ) ;
#30121 = CARTESIAN_POINT ( 'NONE',  ( 10.49813415416005213, 37.82731371789854791, -7.228626920338837358 ) ) ;
#30122 = CARTESIAN_POINT ( 'NONE',  ( 10.49813415415989581, 82.57268628210145778, 7.228626920339068285 ) ) ;
#30123 = CARTESIAN_POINT ( 'NONE',  ( 19.56230152254411792, -5.196152422706629359, -6.937499998771023968 ) ) ;
#30124 = CARTESIAN_POINT ( 'NONE',  ( -3.253724281355068545E-15, 196.2874999999999659, -27.00000000000000000 ) ) ;
#30125 = CARTESIAN_POINT ( 'NONE',  ( 37.17599277676264080, 7.646167579472015790E-16, 163.2555157657388065 ) ) ;
#30126 = CARTESIAN_POINT ( 'NONE',  ( 22.80587116629412137, 7.646167579472024665E-16, -3.121874999385543248 ) ) ;
#30127 = CARTESIAN_POINT ( 'NONE',  ( -54.50000000000000711, 237.0000000000000000, -2.500000000000000000 ) ) ;
#30128 = CARTESIAN_POINT ( 'NONE',  ( -77.00000000000002842, 210.0000000000000000, 5.000000000000000000 ) ) ;
#30129 = CARTESIAN_POINT ( 'NONE',  ( 15.00000000000000000, 244.1500000000000057, 0.000000000000000000 ) ) ;
#30130 = CARTESIAN_POINT ( 'NONE',  ( 5.233372021372432847, 92.34768628210142083, 8.152565276336710909 ) ) ;
#30131 = CARTESIAN_POINT ( 'NONE',  ( 23.99999999999999645, 5.196152422706631135, -2.343749998770960907 ) ) ;
#30132 = CARTESIAN_POINT ( 'NONE',  ( -4.944772684328673229, 139.7851862821014493, 11.48171059495397728 ) ) ;
#30133 =( REPRESENTATION_RELATIONSHIP ('NONE','NONE', #4304, #16167 ) REPRESENTATION_RELATIONSHIP_WITH_TRANSFORMATION ( #15485 )SHAPE_REPRESENTATION_RELATIONSHIP( ) );
#30134 = LINE ( 'NONE', #4165, #19724 ) ;
#30135 = CARTESIAN_POINT ( 'NONE',  ( 15.24356964374999990, 248.9593750006145285, 0.000000000000000000 ) ) ;
#30136 = ORIENTED_EDGE ( 'NONE', *, *, #17571, .T. ) ;
#30137 = CARTESIAN_POINT ( 'NONE',  ( 24.95534962787547073, -3.604726614523240613, 166.8467808440897500 ) ) ;
#30138 = AXIS2_PLACEMENT_3D ( 'NONE', #45, #17131, #28667 ) ;
#30139 = CARTESIAN_POINT ( 'NONE',  ( 26.75643035624999655, 7.049594010296217766E-16, -3.515624999385458249 ) ) ;
#30140 = CARTESIAN_POINT ( 'NONE',  ( -13.62178482187500528, 199.3343750006145569, -23.59362340125807123 ) ) ;
#30141 = CARTESIAN_POINT ( 'NONE',  ( 23.30664739095454507, -5.481896322917826581, -8.000000000000001776 ) ) ;
#30142 = CARTESIAN_POINT ( 'NONE',  ( 31.29200377171330771, 6.928203230275514990, 167.6381414109090997 ) ) ;
#30143 = CARTESIAN_POINT ( 'NONE',  ( 26.99999999999952038, -3.464101615138027057, -7.406249998770969789 ) ) ;
#30144 = CARTESIAN_POINT ( 'NONE',  ( 23.87821517812499650, 242.0593750006145228, -4.985214923628404904 ) ) ;
#30145 = CARTESIAN_POINT ( 'NONE',  ( 25.01087993033039325, 0.000000000000000000, 164.6868468578000488 ) ) ;
#30146 = CARTESIAN_POINT ( 'NONE',  ( -1.715153634034442431, 13.67731371789853867, 9.534712964251900402 ) ) ;
#30147 = CARTESIAN_POINT ( 'NONE',  ( 13.62178482187499640, 197.4593750006145285, -23.59362340125807123 ) ) ;
#30149 = ORIENTED_EDGE ( 'NONE', *, *, #5304, .T. ) ;
#30148 = VERTEX_POINT ( 'NONE', #7101 ) ;
#30150 =( BOUNDED_CURVE ( )  B_SPLINE_CURVE ( 2, ( #945, #14610, #6265, #12520, #6642, #383, #26347 ),
 .UNSPECIFIED., .F., .F. ) 
 B_SPLINE_CURVE_WITH_KNOTS ( ( 3, 2, 2, 3 ),
 ( 0.7391304347826079812, 0.7463768115942022163, 0.7536231884057965624, 0.7608695652173907975 ),
 .UNSPECIFIED. ) 
 CURVE ( )  GEOMETRIC_REPRESENTATION_ITEM ( )  RATIONAL_B_SPLINE_CURVE ( ( 1.000000000000012212, 0.8660254037844263841, 1.000000000000000000, 0.8660254037844387076, 1.000000000000000000, 0.8660254037844489217, 0.9999999999999897859 ) ) 
 REPRESENTATION_ITEM ( '' )  );
#30151 = CARTESIAN_POINT ( 'NONE',  ( 26.75643035624999655, 246.3718750006145228, -7.049594010296217766E-16 ) ) ;
#30152 = CARTESIAN_POINT ( 'NONE',  ( 12.53471296425189330, 20.57731371789854435, 2.311890736173451533 ) ) ;
#30153 = CARTESIAN_POINT ( 'NONE',  ( 26.75643035624999655, -3.323476615752267715, -1.303124999385484095 ) ) ;
#30154 = CARTESIAN_POINT ( 'NONE',  ( -6.092822981423666739, 127.8148137178985735, -14.25334919248795096 ) ) ;
#30155 = CARTESIAN_POINT ( 'NONE',  ( 21.00000000000000000, 6.646953231504538984, -0.3656249993854637226 ) ) ;
#30156 = ORIENTED_EDGE ( 'NONE', *, *, #20025, .F. ) ;
#30157 = CARTESIAN_POINT ( 'NONE',  ( 16.56230152254411436, 7.209453229046482114, -6.609374999385521754 ) ) ;
#30158 = VERTEX_POINT ( 'NONE', #15060 ) ;
#30159 = CARTESIAN_POINT ( 'NONE',  ( -27.24356964375000345, 195.3031250006145285, 0.000000000000000000 ) ) ;
#30160 = CARTESIAN_POINT ( 'NONE',  ( 4.622313124798573369, 138.6351862821014720, 11.61527771782819940 ) ) ;
#30161 = CARTESIAN_POINT ( 'NONE',  ( 34.06772145880400160, 5.407089921784862696, 163.5462758911768617 ) ) ;
#30162 = CARTESIAN_POINT ( 'NONE',  ( -57.91294563604517265, 216.1378603801729241, -6.307003348498026796 ) ) ;
#30163 = CARTESIAN_POINT ( 'NONE',  ( 20.99999999999999645, 246.9343750006145228, -6.646953231504538984 ) ) ;
#30164 = SURFACE_SIDE_STYLE ('',( #18622 ) ) ;
#30165 = CARTESIAN_POINT ( 'NONE',  ( 0.000000000000000000, 200.0000000000000000, -27.00000000000000355 ) ) ;
#30166 = CARTESIAN_POINT ( 'NONE',  ( -49.00669563604517265, 209.8844732041982297, -4.499999999999996447 ) ) ;
#30167 = CARTESIAN_POINT ( 'NONE',  ( 8.962234695871762469, 135.7601862821014720, -8.715434833791931624 ) ) ;
#30168 = CARTESIAN_POINT ( 'NONE',  ( 34.26872439051576436, 5.407089921784857367, 165.8437499136509814 ) ) ;
#30169 = ORIENTED_EDGE ( 'NONE', *, *, #22645, .T. ) ;
#30170 = CARTESIAN_POINT ( 'NONE',  ( -7.234628195640263826, 195.0700961906613600, -27.00000000000003553 ) ) ;
#30171 = CARTESIAN_POINT ( 'NONE',  ( 0.1745138560725837118, 134.6101862821014947, -15.50000000000000533 ) ) ;
#30172 = CARTESIAN_POINT ( 'NONE',  ( -50.00372103062156981, 218.5309553116391896, -2.162041339862839084 ) ) ;
#30173 = CARTESIAN_POINT ( 'NONE',  ( 8.710071997420127943, 119.0851862821014606, 3.796722387233375073 ) ) ;
#30174 = CARTESIAN_POINT ( 'NONE',  ( 19.39230484541326405, 249.0638461906613657, -5.999999999999998224 ) ) ;
#30175 = CARTESIAN_POINT ( 'NONE',  ( -7.228626920339069173, 29.67268628210144499, 10.49813415415989581 ) ) ;
#30176 = CARTESIAN_POINT ( 'NONE',  ( 10.56230152254410548, 3.464101615137757051, -7.687500000000020428 ) ) ;
#30177 = UNCERTAINTY_MEASURE_WITH_UNIT (LENGTH_MEASURE( 1.000000000000000082E-05 ), #6522, 'distance_accuracy_value', 'NONE');
#30178 = VECTOR ( 'NONE', #18401, 1000.000000000000227 ) ;
#30179 = ORIENTED_EDGE ( 'NONE', *, *, #34414, .T. ) ;
#30180 = CARTESIAN_POINT ( 'NONE',  ( -1.045839947578415010E-13, 196.1750000012290229, 27.00000000000000355 ) ) ;
#30181 = CARTESIAN_POINT ( 'NONE',  ( -15.46528703574804986, 114.1976862821014578, -3.257655550457287497 ) ) ;
#30182 = DIRECTION ( 'NONE',  ( 0.9961946980917462113, 0.000000000000000000, -0.08715574274765178209 ) ) ;
#30183 = CARTESIAN_POINT ( 'NONE',  ( -7.954856959092191815, 4.372686282101438948, -5.529263428287477744 ) ) ;
#30184 = CARTESIAN_POINT ( 'NONE',  ( 13.62178482187499640, 198.7531250006145456, -23.59362340125807123 ) ) ;
#30185 = CARTESIAN_POINT ( 'NONE',  ( 21.00000000000000355, 0.000000000000000000, 50.00000000000001421 ) ) ;
#30186 = CARTESIAN_POINT ( 'NONE',  ( -13.50000000000000533, 195.4250000000000114, -23.38268590217984411 ) ) ;
#30187 = CARTESIAN_POINT ( 'NONE',  ( 22.56230152254411792, 7.347880794884125653E-16, -5.625000000000018652 ) ) ;
#30188 = CARTESIAN_POINT ( 'NONE',  ( 36.82794601260381029, 7.347880794884125653E-16, 162.0719712953337250 ) ) ;
#30189 = CARTESIAN_POINT ( 'NONE',  ( 9.465287035748106703, 75.20231371789854791, -2.064181346179063237 ) ) ;
#30190 = VERTEX_POINT ( 'NONE', #24344 ) ;
#30191 = CARTESIAN_POINT ( 'NONE',  ( 15.00000000000000178, 243.3437500012290400, 3.464101615137757051 ) ) ;
#30192 = CARTESIAN_POINT ( 'NONE',  ( -11.61527771782809282, 89.86481371789855643, -4.622313124798832717 ) ) ;
#30193 = CARTESIAN_POINT ( 'NONE',  ( 10.31873187879410558, -3.604726614523244610, -4.209374999385490312 ) ) ;
#30194 = CARTESIAN_POINT ( 'NONE',  ( -10.52346919520418922, 142.9999999999999432, 8.647714196784560770 ) ) ;
#30195 = CARTESIAN_POINT ( 'NONE',  ( 15.24356964374999990, 0.000000000000000000, -5.203124999385494220 ) ) ;
#30196 = CARTESIAN_POINT ( 'NONE',  ( -6.932735513424201912, 51.05231371789854933, 10.69584247140429412 ) ) ;
#30197 = ORIENTED_EDGE ( 'NONE', *, *, #9657, .T. ) ;
#30198 = CARTESIAN_POINT ( 'NONE',  ( 20.99999999999999645, 185.0294372515228645, 5.999999999999999112 ) ) ;
#30199 = CARTESIAN_POINT ( 'NONE',  ( 15.24356964374999990, 243.8968750006145285, 0.000000000000000000 ) ) ;
#30200 = CARTESIAN_POINT ( 'NONE',  ( -6.932735513423968321, 23.34768628210144570, -10.69584247140445221 ) ) ;
#30201 = EDGE_CURVE ( 'NONE', #21112, #3622, #35968, .T. ) ;
#30202 = CARTESIAN_POINT ( 'NONE',  ( -41.28794563604515844, 205.3262412349648116, 4.842901733360249317 ) ) ;
#30203 = CARTESIAN_POINT ( 'NONE',  ( -50.59002896937850124, 204.4285982733020433, 3.350049139982171020 ) ) ;
#30204 =( NAMED_UNIT ( * ) SI_UNIT ( $, .STERADIAN. ) SOLID_ANGLE_UNIT ( ) );
#30205 = CYLINDRICAL_SURFACE ( 'NONE', #3647, 5.999999999999999112 ) ;
#30206 = CARTESIAN_POINT ( 'NONE',  ( -4.622313124798826500, 78.36481371789855643, 11.61527771782809637 ) ) ;
#30207 = CARTESIAN_POINT ( 'NONE',  ( -41.69122103062156270, 208.9097554298617752, -4.530955311639240257 ) ) ;
#30208 = CARTESIAN_POINT ( 'NONE',  ( -51.98288769728821990, 203.5309553116391612, -1.857196546604028775 ) ) ;
#30209 = ADVANCED_FACE ( 'NONE', ( #12774 ), #21510, .T. ) ;
#30210 =( BOUNDED_CURVE ( )  B_SPLINE_CURVE ( 3, ( #3419, #21439, #14987, #7033 ),
 .UNSPECIFIED., .F., .F. ) 
 B_SPLINE_CURVE_WITH_KNOTS ( ( 4, 4 ),
 ( 4.712388980384690562, 6.283185307179586232 ),
 .UNSPECIFIED. ) 
 CURVE ( )  GEOMETRIC_REPRESENTATION_ITEM ( )  RATIONAL_B_SPLINE_CURVE ( ( 1.000000000000000000, 0.8047378541243652705, 0.8047378541243652705, 1.000000000000000000 ) ) 
 REPRESENTATION_ITEM ( '' )  );
#30211 = CARTESIAN_POINT ( 'NONE',  ( 15.24356964374999990, 0.000000000000000000, -6.103124999385478588 ) ) ;
#30212 = DIRECTION ( 'NONE',  ( 0.08715574274765150453, 0.000000000000000000, 0.9961946980917461003 ) ) ;
#30213 = CARTESIAN_POINT ( 'NONE',  ( -11.08355503943118592, 62.83981371789855785, -10.83675517735179383 ) ) ;
#30214 = CARTESIAN_POINT ( 'NONE',  ( -45.64211230271183695, 201.5309553116392181, 2.393094931466368980 ) ) ;
#30215 = FACE_OUTER_BOUND ( 'NONE', #26880, .T. ) ;
#30216 = CARTESIAN_POINT ( 'NONE',  ( -4.622313124798576922, 78.83518628210146062, -11.61527771782819762 ) ) ;
#30217 = CARTESIAN_POINT ( 'NONE',  ( 2.908627838312118019, 19.32268628210144001, 15.53471296425195369 ) ) ;
#30218 = EDGE_CURVE ( 'NONE', #20931, #25619, #19504, .T. ) ;
#30219 = DIRECTION ( 'NONE',  ( 1.000000000000000000, 0.000000000000000000, 0.000000000000000000 ) ) ;
#30220 = CARTESIAN_POINT ( 'NONE',  ( -27.93311285808765732, 208.1767028850233885, -7.793846208402254838 ) ) ;
#30221 = ORIENTED_EDGE ( 'NONE', *, *, #14345, .F. ) ;
#30222 = CARTESIAN_POINT ( 'NONE',  ( 10.83675517735155225, 55.26018628210144357, 11.08355503943142573 ) ) ;
#30223 = CARTESIAN_POINT ( 'NONE',  ( 27.24356964375000345, 198.2281250006145399, -3.336375036156643733E-15 ) ) ;
#30224 = ADVANCED_FACE ( 'NONE', ( #30773 ), #4979, .F. ) ;
#30225 = CARTESIAN_POINT ( 'NONE',  ( 13.62178482187501416, 199.5593750006145513, 23.59362340125806767 ) ) ;
#30226 = CARTESIAN_POINT ( 'NONE',  ( -40.89955436395488420, 214.8429017333601792, -4.673758765035196383 ) ) ;
#30227 = CARTESIAN_POINT ( 'NONE',  ( 24.99999999999999289, 0.000000000000000000, 49.65004534589634488 ) ) ;
#30228 = ADVANCED_FACE ( 'NONE', ( #19597 ), #7653, .F. ) ;
#30229 = CARTESIAN_POINT ( 'NONE',  ( 8.962234695871762469, 25.36018628210144499, -8.715434833791931624 ) ) ;
#30230 = CARTESIAN_POINT ( 'NONE',  ( 9.000000000000003553, 242.0000000000000000, -5.999999999999998224 ) ) ;
#30231 = CARTESIAN_POINT ( 'NONE',  ( -8.152565276336593669, 136.1523137178985507, -5.233372021372610483 ) ) ;
#30232 = CARTESIAN_POINT ( 'NONE',  ( 23.87821517812499650, 243.4093750006145171, -4.985214923628404904 ) ) ;
#30233 = VERTEX_POINT ( 'NONE', #19230 ) ;
#30234 = CARTESIAN_POINT ( 'NONE',  ( 15.00000000000000178, 245.1437500012290798, 3.464101615137757051 ) ) ;
#30235 = CARTESIAN_POINT ( 'NONE',  ( -2.660918448318005058, 128.1023137178985678, -12.46528703574811558 ) ) ;
#30236 = CARTESIAN_POINT ( 'NONE',  ( 22.80587116629411071, -3.604726614523235284, -7.153124999385556571 ) ) ;
#30237 = CARTESIAN_POINT ( 'NONE',  ( 27.85934967376930516, 5.407089921784856479, 164.2211893949991293 ) ) ;
#30238 = CARTESIAN_POINT ( 'NONE',  ( 25.44230085693126497, 0.000000000000000000, 169.6180106133541869 ) ) ;
#30239 = CARTESIAN_POINT ( 'NONE',  ( -26.99999999999998934, 197.7875000000000227, 15.58845726811991561 ) ) ;
#30240 = VERTEX_POINT ( 'NONE', #16374 ) ;
#30241 = CARTESIAN_POINT ( 'NONE',  ( -4.622313124798576922, 32.83518628210143930, -11.61527771782819762 ) ) ;
#30242 = ORIENTED_EDGE ( 'NONE', *, *, #11135, .T. ) ;
#30243 = ORIENTED_EDGE ( 'NONE', *, *, #24913, .T. ) ;
#30244 = LINE ( 'NONE', #15278, #22484 ) ;
#30245 = DIRECTION ( 'NONE',  ( 0.000000000000000000, -0.000000000000000000, 1.000000000000000000 ) ) ;
#30246 = CARTESIAN_POINT ( 'NONE',  ( 26.99999999999999645, 249.3812500012290343, -7.347880794884117764E-16 ) ) ;
#30247 = DIRECTION ( 'NONE',  ( -0.000000000000000000, 1.000000000000000000, -0.000000000000000000 ) ) ;
#30248 = CARTESIAN_POINT ( 'NONE',  ( 18.12178482187500350, -4.985214923628407568, -9.515624999385464022 ) ) ;
#30249 = CARTESIAN_POINT ( 'NONE',  ( -7.228626920339069173, 84.87268628210146915, 10.49813415415989581 ) ) ;
#30250 = CARTESIAN_POINT ( 'NONE',  ( 8.927990412390657937, 135.4726862821014777, -13.04141134922759804 ) ) ;
#30251 = CARTESIAN_POINT ( 'NONE',  ( 22.60769515458672885, 243.6236538117967143, -5.999999999999998224 ) ) ;
#30252 = CARTESIAN_POINT ( 'NONE',  ( 18.34109276192021909, 217.0904193015437613, 5.392997762649728521 ) ) ;
#30253 = CARTESIAN_POINT ( 'NONE',  ( -60.48586230271183695, 207.8500491399821613, 3.954877714930852495 ) ) ;
#30254 = CYLINDRICAL_SURFACE ( 'NONE', #12518, 6.000000000000001776 ) ;
#30255 = CARTESIAN_POINT ( 'NONE',  ( 34.13024420985595953, 5.196152422706631135, 165.6582383296822343 ) ) ;
#30256 = CARTESIAN_POINT ( 'NONE',  ( -2.311890736173448424, 133.2773137178985507, 12.53471296425189330 ) ) ;
#30257 = EDGE_CURVE ( 'NONE', #30542, #30763, #29879, .T. ) ;
#30258 = CARTESIAN_POINT ( 'NONE',  ( -52.18080436395490551, 203.5000000000000000, -0.1155267958017335561 ) ) ;
#30259 = CARTESIAN_POINT ( 'NONE',  ( -63.26413769728823411, 214.1499508600179240, 7.418979330068584233 ) ) ;
#30260 = EDGE_CURVE ( 'NONE', #36155, #5728, #7026, .T. ) ;
#30261 = PRODUCT_CONTEXT ( 'NONE', #3005, 'mechanical' ) ;
#30262 = CARTESIAN_POINT ( 'NONE',  ( 18.12178482187499640, 4.985214923628404904, -0.7781249993854821856 ) ) ;
#30263 = CARTESIAN_POINT ( 'NONE',  ( -1.926257025242585782E-15, 199.2406250006145285, -31.45816453501075927 ) ) ;
#30264 = CARTESIAN_POINT ( 'NONE',  ( 15.53471296425188797, 121.7773137178985650, 2.908627838312457747 ) ) ;
#30265 = CARTESIAN_POINT ( 'NONE',  ( -43.66294563604516554, 214.6737587650350747, -4.842901733360249317 ) ) ;
#30266 = EDGE_CURVE ( 'NONE', #35280, #18752, #25557, .T. ) ;
#30267 = EDGE_LOOP ( 'NONE', ( #14482, #9425, #32659, #3575 ) ) ;
#30268 = CARTESIAN_POINT ( 'NONE',  ( 27.87526709119022783, 5.196152422706636465, 163.0058021847763712 ) ) ;
#30269 = CARTESIAN_POINT ( 'NONE',  ( -27.00000000000000355, 197.7500000000000000, 0.000000000000000000 ) ) ;
#30270 = CARTESIAN_POINT ( 'NONE',  ( 24.82951852428355011, 0.000000000000000000, 165.4085247487197989 ) ) ;
#30271 = CARTESIAN_POINT ( 'NONE',  ( 8.927990412390657937, 98.67268628210146630, -13.04141134922759804 ) ) ;
#30272 = CARTESIAN_POINT ( 'NONE',  ( -60.49330436395489841, 210.1155267958017134, -6.500000000000000888 ) ) ;
#30273 = ADVANCED_FACE ( 'NONE', ( #2330 ), #22063, .F. ) ;
#30274 = CARTESIAN_POINT ( 'NONE',  ( 10.31873187879410914, 0.000000000000000000, -3.290624999385538541 ) ) ;
#30275 = CARTESIAN_POINT ( 'NONE',  ( 0.1745138560725194299, 33.41018628210144925, -9.500000000000005329 ) ) ;
#30276 = CARTESIAN_POINT ( 'NONE',  ( -38.92038769728823411, 207.6069050685337913, 8.469044688360781947 ) ) ;
#30277 = CARTESIAN_POINT ( 'NONE',  ( 19.68408634441911431, -5.407089921784861808, -9.946874999385540761 ) ) ;
#30278 = CARTESIAN_POINT ( 'NONE',  ( -10.49813415415989581, 77.97268628210144925, -7.228626920339068285 ) ) ;
#30279 = CARTESIAN_POINT ( 'NONE',  ( -1.909035429704832693E-15, 199.4375000000000284, -31.17691453623979214 ) ) ;
#30280 = FACE_OUTER_BOUND ( 'NONE', #26004, .T. ) ;
#30282 = ORIENTED_EDGE ( 'NONE', *, *, #13782, .T. ) ;
#30281 = CARTESIAN_POINT ( 'NONE',  ( -9.465287035748065847, 40.59768628210144215, -2.064181346179273735 ) ) ;
#30283 = FACE_OUTER_BOUND ( 'NONE', #27514, .T. ) ;
#30284 = EDGE_LOOP ( 'NONE', ( #37239, #30927, #36591, #24473, #14939, #27207 ) ) ;
#30285 = CARTESIAN_POINT ( 'NONE',  ( 23.99999999999999645, 5.196152422706631135, -1.950000000000007283 ) ) ;
#30286 = VECTOR ( 'NONE', #17654, 1000.000000000000000 ) ;
#30287 = CARTESIAN_POINT ( 'NONE',  ( -65.04538769728824832, 211.8571965466039444, -6.469044688360768625 ) ) ;
#30288 = CARTESIAN_POINT ( 'NONE',  ( 30.86303410043077022, -7.209453229046482114, 162.7349956318509783 ) ) ;
#30289 = CARTESIAN_POINT ( 'NONE',  ( 30.70370250816666058, 6.928203230275514990, 160.9138271987898463 ) ) ;
#30290 = CARTESIAN_POINT ( 'NONE',  ( 23.99999999999999645, 246.6999999999999886, -5.196152422706631135 ) ) ;
#30291 = PLANE ( 'NONE',  #916 ) ;
#30292 = CARTESIAN_POINT ( 'NONE',  ( -12.46528703574811558, 89.00231371789855928, 2.660918448318003726 ) ) ;
#30293 = CARTESIAN_POINT ( 'NONE',  ( 6.932735513423970097, 110.7476862821014691, 10.69584247140445044 ) ) ;
#30294 = EDGE_LOOP ( 'NONE', ( #24734, #23406, #13748, #36287 ) ) ;
#30295 = ORIENTED_EDGE ( 'NONE', *, *, #35212, .T. ) ;
#30296 = CARTESIAN_POINT ( 'NONE',  ( -27.00000000000000355, 199.2125000012290457, 0.000000000000000000 ) ) ;
#30297 = CARTESIAN_POINT ( 'NONE',  ( 1.120210788295102201E-13, 196.7375000000000398, -27.00000000000000711 ) ) ;
#30298 = CARTESIAN_POINT ( 'NONE',  ( 13.04141134922778988, 65.42731371789857064, -8.927990412390371944 ) ) ;
#30299 = CARTESIAN_POINT ( 'NONE',  ( 21.00000000000000000, -6.646953231504538984, -6.890624999385480898 ) ) ;
#30300 = CARTESIAN_POINT ( 'NONE',  ( 23.87821517812499650, 245.2093750006145569, -4.985214923628404904 ) ) ;
#30301 = AXIS2_PLACEMENT_3D ( 'NONE', #33771, #24864, #5137 ) ;
#30302 = CARTESIAN_POINT ( 'NONE',  ( -61.48288769728824121, 205.5309553116392465, -1.321298161741839117 ) ) ;
#30303 = CARTESIAN_POINT ( 'NONE',  ( -26.99999999999998934, 195.2000000012290286, 15.58845726811991561 ) ) ;
#30304 = EDGE_CURVE ( 'NONE', #36194, #16873, #33726, .T. ) ;
#30305 = CARTESIAN_POINT ( 'NONE',  ( -2.064181346179062349, 63.70231371789854791, -9.465287035748106703 ) ) ;
#30306 = CARTESIAN_POINT ( 'NONE',  ( 19.68408634441910721, -5.407089921784855591, -8.540624999385542537 ) ) ;
#30307 = CARTESIAN_POINT ( 'NONE',  ( -0.1745138560723084320, 109.9898137178985706, -9.500000000000005329 ) ) ;
#30308 = DIRECTION ( 'NONE',  ( 0.000000000000000000, -0.000000000000000000, 1.000000000000000000 ) ) ;
#30309 = CARTESIAN_POINT ( 'NONE',  ( 7.228626920338837358, 30.92731371789854222, 10.49813415416005036 ) ) ;
#30310 =( BOUNDED_SURFACE ( )  B_SPLINE_SURFACE ( 1, 2, ( 
 ( #35898, #15258, #9941, #21335, #6921, #18492, #30032, #21521, #30225, #19055, #8036, #31335, #4623, #27933, #36830, #7851, #13730, #5363, #22074, #2341, #19424, #4991, #25278, #33814, #33626, #5179, #25463, #10872, #31158, #19799, #28303, #37015, #13534, #13348, #14093, #13912, #11058, #22445, #30974, #16941, #33992, #24904, #30785, #16573, #25645, #4808, #19611, #16388, #7666, #25089, #16755, #22633, #34181, #1963, #8225, #36645, #10683, #36455, #28483, #28118, #19244, #2526, #37199, #11243, #2149, #27751, #22815, #22262, #34363, #30606, #10495, #16202, #1781, #34918, #26386, #8962, #11986, #29226, #8586, #5732, #5919, #31704, #17877, #25830, #23368, #20534, #9151, #14840, #28665, #20348, #17311, #2888, #20155, #17129, #28854, #31518, #6105, #34731, #32077, #14460, #2702, #26016, #17499, #37377, #44, #11610, #11429, #22997, #23184, #17688, #34546, #6306, #8775, #604, #3268, #420, #23558, #31890, #35103, #29034, #3078, #14278, #20718, #14647, #26197, #29422, #32262, #3456, #235, #11799, #15025, #26575, #12173, #23747, #8408 ),
 ( #19976, #5543, #1174, #1552, #27151, #10091, #35858, #24501, #7074, #35670, #32452, #21483, #24127, #29992, #26955, #6685, #18642, #9899, #12748, #15977, #24315, #35481, #4023, #33023, #23938, #1367, #18070, #26766, #30184, #4210, #6496, #27527, #30374, #15788, #9720, #13124, #29612, #27337, #15217, #12938, #21294, #6875, #32830, #36047, #35285, #9343, #21661, #33214, #3648, #7254, #29800, #18450, #20913, #15595, #21105, #18828, #798, #4395, #12368, #9530, #32643, #18256, #3833, #15411, #985, #12561, #27893, #19011, #34139, #27711, #19201, #25423, #4586, #13491, #1740, #28266, #24678, #19568, #36788, #13307, #21848, #10831, #13874, #10643, #22406, #13689, #8186, #33953, #31298, #11019, #7996, #16162, #36976, #22221, #31120, #5138, #4949, #16719, #30932, #30569, #24866, #36414, #10273, #2298, #25049, #22593, #30748, #7439, #33586, #33773, #10457, #7626, #22035, #4771, #16344, #1923, #19761, #36602, #5327, #7813, #16903, #28444, #19389, #33400, #2482, #36232, #16531, #28078, #2111, #25237, #8370, #20308, #3039, #25975, #34324 ) ),
 .UNSPECIFIED., .F., .F., .F. ) 
 B_SPLINE_SURFACE_WITH_KNOTS ( ( 2, 2 ),
 ( 3, 2, 2, 2, 2, 2, 2, 2, 2, 2, 2, 2, 2, 2, 2, 2, 2, 2, 2, 2, 2, 2, 2, 2, 2, 2, 2, 2, 2, 2, 2, 2, 2, 2, 2, 2, 2, 2, 2, 2, 2, 2, 2, 2, 2, 2, 2, 2, 2, 2, 2, 2, 2, 2, 2, 2, 2, 2, 2, 2, 2, 2, 2, 2, 2, 2, 2, 3 ),
 ( 0.000000000000000000, 1.000000000000000000 ),
 ( 0.000000000000000000, 0.01388888888888888812, 0.02777777777777777624, 0.04166666666666666435, 0.05555555555555555247, 0.06944444444444444753, 0.08333333333333332871, 0.09722222222222222376, 0.1111111111111111049, 0.1250000000000000000, 0.1388888888888888951, 0.1527777777777777901, 0.1666666666666666574, 0.1805555555555555525, 0.1944444444444444475, 0.2083333333333333426, 0.2222222222222222099, 0.2361111111111111049, 0.2500000000000000000, 0.2638888888888888951, 0.2777777777777777901, 0.2916666666666666852, 0.3055555555555555802, 0.3194444444444444198, 0.3333333333333333148, 0.3472222222222222099, 0.3611111111111111049, 0.3750000000000000000, 0.3888888888888888951, 0.4027777777777777901, 0.4166666666666666852, 0.4305555555555555802, 0.4444444444444444198, 0.4583333333333333148, 0.4722222222222222099, 0.4861111111111111049, 0.5000000000000000000, 0.5138888888888888395, 0.5277777777777777901, 0.5416666666666666297, 0.5555555555555555802, 0.5694444444444444198, 0.5833333333333333703, 0.5972222222222222099, 0.6111111111111111605, 0.6250000000000000000, 0.6388888888888888395, 0.6527777777777777901, 0.6666666666666666297, 0.6805555555555555802, 0.6944444444444444198, 0.7083333333333333703, 0.7222222222222222099, 0.7361111111111111605, 0.7500000000000000000, 0.7638888888888888395, 0.7777777777777777901, 0.7916666666666666297, 0.8055555555555555802, 0.8194444444444444198, 0.8333333333333333703, 0.8472222222222222099, 0.8611111111111111605, 0.8750000000000000000, 0.8888888888888888395, 0.9027777777777777901, 0.9166666666666666297, 0.9258785558287927486 ),
 .UNSPECIFIED. ) 
 GEOMETRIC_REPRESENTATION_ITEM ( )  RATIONAL_B_SPLINE_SURFACE ( (
 ( 1.000000000000000000, 0.8660254037844387076, 1.000000000000000000, 0.8660254037844387076, 1.000000000000000000, 0.8660254037844387076, 1.000000000000000000, 0.8660254037844387076, 1.000000000000000000, 0.8660254037844387076, 1.000000000000000000, 0.8660254037844387076, 1.000000000000000000, 0.8660254037844387076, 1.000000000000000000, 0.8660254037844387076, 1.000000000000000000, 0.8660254037844387076, 1.000000000000000000, 0.8660254037844387076, 1.000000000000000000, 0.8660254037844387076, 1.000000000000000000, 0.8660254037844387076, 1.000000000000000000, 0.8660254037844387076, 1.000000000000000000, 0.8660254037844387076, 1.000000000000000000, 0.8660254037844387076, 1.000000000000000000, 0.8660254037844387076, 1.000000000000000000, 0.8660254037844387076, 1.000000000000000000, 0.8660254037844387076, 1.000000000000000000, 0.8660254037844387076, 1.000000000000000000, 0.8660254037844387076, 1.000000000000000000, 0.8660254037844387076, 1.000000000000000000, 0.8660254037844387076, 1.000000000000000000, 0.8660254037844387076, 1.000000000000000000, 0.8660254037844387076, 1.000000000000000000, 0.8660254037844387076, 1.000000000000000000, 0.8660254037844387076, 1.000000000000000000, 0.8660254037844387076, 1.000000000000000000, 0.8660254037844387076, 1.000000000000000000, 0.8660254037844387076, 1.000000000000000000, 0.8660254037844387076, 1.000000000000000000, 0.8660254037844387076, 1.000000000000000000, 0.8660254037844387076, 1.000000000000000000, 0.8660254037844387076, 1.000000000000000000, 0.8660254037844387076, 1.000000000000000000, 0.8660254037844387076, 1.000000000000000000, 0.8660254037844387076, 1.000000000000000000, 0.8660254037844387076, 1.000000000000000000, 0.8660254037844387076, 1.000000000000000000, 0.8660254037844387076, 1.000000000000000000, 0.8660254037844387076, 1.000000000000000000, 0.8660254037844387076, 1.000000000000000000, 0.8660254037844387076, 1.000000000000000000, 0.8660254037844387076, 1.000000000000000000, 0.8660254037844387076, 1.000000000000000000, 0.8660254037844387076, 1.000000000000000000, 0.8660254037844387076, 1.000000000000000000, 0.8660254037844387076, 1.000000000000000000, 0.8660254037844387076, 1.000000000000000000, 0.8660254037844387076, 1.000000000000000000, 0.8660254037844387076, 1.000000000000000000, 0.8660254037844387076, 1.000000000000000000, 0.8660254037844387076, 1.000000000000000000, 0.8660254037844387076, 1.000000000000000000, 0.8660254037844387076, 1.000000000000000000, 0.8660254037844387076, 1.000000000000000000, 0.8660254037844387076, 1.000000000000000000, 0.8660254037844387076, 1.000000000000000000, 0.8660254037844387076, 1.000000000000000000, 0.8660254037844387076, 1.000000000000000000, 0.8660254037844387076, 1.000000000000000000, 0.8660254037844387076, 1.000000000000000000, 0.8660254037844387076, 1.000000000000000000, 0.8660254037844387076, 1.000000000000000000, 0.8660254037844387076, 1.000000000000000000, 0.8660254037844387076, 1.000000000000000000, 0.8660254037844387076, 1.000000000000000000, 0.9111405425767590271, 0.9401542252352144136),
 ( 1.000000000000000000, 0.8660254037844387076, 1.000000000000000000, 0.8660254037844387076, 1.000000000000000000, 0.8660254037844387076, 1.000000000000000000, 0.8660254037844387076, 1.000000000000000000, 0.8660254037844387076, 1.000000000000000000, 0.8660254037844387076, 1.000000000000000000, 0.8660254037844387076, 1.000000000000000000, 0.8660254037844387076, 1.000000000000000000, 0.8660254037844387076, 1.000000000000000000, 0.8660254037844387076, 1.000000000000000000, 0.8660254037844387076, 1.000000000000000000, 0.8660254037844387076, 1.000000000000000000, 0.8660254037844387076, 1.000000000000000000, 0.8660254037844387076, 1.000000000000000000, 0.8660254037844387076, 1.000000000000000000, 0.8660254037844387076, 1.000000000000000000, 0.8660254037844387076, 1.000000000000000000, 0.8660254037844387076, 1.000000000000000000, 0.8660254037844387076, 1.000000000000000000, 0.8660254037844387076, 1.000000000000000000, 0.8660254037844387076, 1.000000000000000000, 0.8660254037844387076, 1.000000000000000000, 0.8660254037844387076, 1.000000000000000000, 0.8660254037844387076, 1.000000000000000000, 0.8660254037844387076, 1.000000000000000000, 0.8660254037844387076, 1.000000000000000000, 0.8660254037844387076, 1.000000000000000000, 0.8660254037844387076, 1.000000000000000000, 0.8660254037844387076, 1.000000000000000000, 0.8660254037844387076, 1.000000000000000000, 0.8660254037844387076, 1.000000000000000000, 0.8660254037844387076, 1.000000000000000000, 0.8660254037844387076, 1.000000000000000000, 0.8660254037844387076, 1.000000000000000000, 0.8660254037844387076, 1.000000000000000000, 0.8660254037844387076, 1.000000000000000000, 0.8660254037844387076, 1.000000000000000000, 0.8660254037844387076, 1.000000000000000000, 0.8660254037844387076, 1.000000000000000000, 0.8660254037844387076, 1.000000000000000000, 0.8660254037844387076, 1.000000000000000000, 0.8660254037844387076, 1.000000000000000000, 0.8660254037844387076, 1.000000000000000000, 0.8660254037844387076, 1.000000000000000000, 0.8660254037844387076, 1.000000000000000000, 0.8660254037844387076, 1.000000000000000000, 0.8660254037844387076, 1.000000000000000000, 0.8660254037844387076, 1.000000000000000000, 0.8660254037844387076, 1.000000000000000000, 0.8660254037844387076, 1.000000000000000000, 0.8660254037844387076, 1.000000000000000000, 0.8660254037844387076, 1.000000000000000000, 0.8660254037844387076, 1.000000000000000000, 0.8660254037844387076, 1.000000000000000000, 0.8660254037844387076, 1.000000000000000000, 0.8660254037844387076, 1.000000000000000000, 0.8660254037844387076, 1.000000000000000000, 0.8660254037844387076, 1.000000000000000000, 0.8660254037844387076, 1.000000000000000000, 0.8660254037844387076, 1.000000000000000000, 0.8660254037844387076, 1.000000000000000000, 0.8660254037844387076, 1.000000000000000000, 0.8660254037844387076, 1.000000000000000000, 0.8660254037844387076, 1.000000000000000000, 0.8660254037844387076, 1.000000000000000000, 0.8660254037844387076, 1.000000000000000000, 0.9111405425767590271, 0.9401542252352144136) ) ) 
 REPRESENTATION_ITEM ( '' )  SURFACE ( )  );
#30311 = CARTESIAN_POINT ( 'NONE',  ( 7.228626920339068285, 89.47268628210144925, -10.49813415415989581 ) ) ;
#30312 = CARTESIAN_POINT ( 'NONE',  ( 16.56230152254411436, -6.928203230275506996, -7.424999998770979381 ) ) ;
#30313 = DIRECTION ( 'NONE',  ( 1.000000000000000000, 0.000000000000000000, 0.000000000000000000 ) ) ;
#30314 = CARTESIAN_POINT ( 'NONE',  ( 30.94637677943320497, -7.209453229046475009, 163.6876068119012189 ) ) ;
#30315 = CARTESIAN_POINT ( 'NONE',  ( 16.56230152254411436, -7.209453229046482114, -3.234374999385536853 ) ) ;
#30316 = CARTESIAN_POINT ( 'NONE',  ( -27.00000000000000355, 197.7500000000000000, 0.000000000000000000 ) ) ;
#30317 = CARTESIAN_POINT ( 'NONE',  ( 26.99999999999999645, 7.347880794884117764E-16, -3.768749998770942966 ) ) ;
#30318 = DIRECTION ( 'NONE',  ( 0.08715574274765150453, 0.000000000000000000, 0.9961946980917461003 ) ) ;
#30319 = CARTESIAN_POINT ( 'NONE',  ( 7.954856959092191815, 100.9726862821014635, 5.529263428287477744 ) ) ;
#30320 = CARTESIAN_POINT ( 'NONE',  ( 15.00000000000008171, -3.464101615137802348, -4.406249998770950249 ) ) ;
#30321 = CARTESIAN_POINT ( 'NONE',  ( -8.962234695871760692, 140.3601862821014379, 8.715434833791933400 ) ) ;
#30322 = CARTESIAN_POINT ( 'NONE',  ( 20.99999999999999289, 249.4937500012290457, -5.999999999999998224 ) ) ;
#30323 = CARTESIAN_POINT ( 'NONE',  ( 15.24356964374999990, 249.3718750006145228, -3.323476615752268604 ) ) ;
#30325 = ORIENTED_EDGE ( 'NONE', *, *, #35174, .F. ) ;
#30324 = VECTOR ( 'NONE', #35462, 1000.000000000000000 ) ;
#30326 = CARTESIAN_POINT ( 'NONE',  ( 37.25443294523552851, 7.646167579472015790E-16, 164.1520909940213642 ) ) ;
#30327 = CARTESIAN_POINT ( 'NONE',  ( 26.75643035624999655, 7.049594010296217766E-16, -3.965624999385464200 ) ) ;
#30328 = CARTESIAN_POINT ( 'NONE',  ( -27.24356964375000345, 198.0593750006145513, 0.000000000000000000 ) ) ;
#30329 = CARTESIAN_POINT ( 'NONE',  ( 37.33780710767756972, 7.347880794884125653E-16, 167.8997102791704492 ) ) ;
#30330 = CARTESIAN_POINT ( 'NONE',  ( 15.24356964374999990, 0.000000000000000000, -0.1406249993854691294 ) ) ;
#30331 = CARTESIAN_POINT ( 'NONE',  ( 15.24356964375000167, 244.0468750006145342, 3.323476615752272600 ) ) ;
#30332 = CARTESIAN_POINT ( 'NONE',  ( 10.31873187879411091, 0.000000000000000000, -2.840624999385532590 ) ) ;
#30333 =( BOUNDED_CURVE ( )  B_SPLINE_CURVE ( 2, ( #12132, #1134, #15176, #23899, #20875, #756, #12326 ),
 .UNSPECIFIED., .F., .F. ) 
 B_SPLINE_CURVE_WITH_KNOTS ( ( 3, 2, 2, 3 ),
 ( 0.5217391304347842595, 0.5289855072463786057, 0.5362318840579728407, 0.5434782608695670758 ),
 .UNSPECIFIED. ) 
 CURVE ( )  GEOMETRIC_REPRESENTATION_ITEM ( )  RATIONAL_B_SPLINE_CURVE ( ( 0.9999999999999692468, 0.8660254037844694608, 1.000000000000000000, 0.8660254037844387076, 1.000000000000000000, 0.8660254037844038466, 1.000000000000034861 ) ) 
 REPRESENTATION_ITEM ( '' )  );
#30334 = CARTESIAN_POINT ( 'NONE',  ( -12.50000000000000355, 135.2898137178985678, 0.1745138560722786503 ) ) ;
#30335 = CARTESIAN_POINT ( 'NONE',  ( 5.778771075727756162E-15, 197.7218750006145456, 31.45816453501076637 ) ) ;
#30337 = ORIENTED_EDGE ( 'NONE', *, *, #14770, .F. ) ;
#30336 = ORIENTED_EDGE ( 'NONE', *, *, #7768, .T. ) ;
#30338 = CARTESIAN_POINT ( 'NONE',  ( 15.24356964374999990, 247.0093750006145115, -3.323476615752268604 ) ) ;
#30339 = CARTESIAN_POINT ( 'NONE',  ( -12.50000000000000355, 34.08981371789854364, 0.1745138560722786503 ) ) ;
#30340 = CARTESIAN_POINT ( 'NONE',  ( 26.75643035624999655, 3.323476615752271712, -3.478124999385468819 ) ) ;
#30341 = CARTESIAN_POINT ( 'NONE',  ( -5.770363421894122880, 124.3648137178985849, 14.38691631536194393 ) ) ;
#30342 = EDGE_CURVE ( 'NONE', #27706, #15426, #27225, .T. ) ;
#30343 = CARTESIAN_POINT ( 'NONE',  ( 26.99999999999999645, 3.464101615137755275, -9.131249998770954335 ) ) ;
#30344 = ORIENTED_EDGE ( 'NONE', *, *, #35976, .T. ) ;
#30345 = CARTESIAN_POINT ( 'NONE',  ( 22.80587116629411781, -3.604726614523238837, -6.759374999385540761 ) ) ;
#30346 = EDGE_CURVE ( 'NONE', #27758, #8211, #33802, .T. ) ;
#30347 = VERTEX_POINT ( 'NONE', #27553 ) ;
#30348 = CARTESIAN_POINT ( 'NONE',  ( 27.24356964375000700, 197.2906250006145399, 15.72908226750537075 ) ) ;
#30349 = CARTESIAN_POINT ( 'NONE',  ( -12.53471296425194836, 141.2226862821014493, 2.311890736173176641 ) ) ;
#30350 = CARTESIAN_POINT ( 'NONE',  ( 36.97498984505087805, 7.646167579472024665E-16, 160.9580417432647153 ) ) ;
#30351 = EDGE_CURVE ( 'NONE', #10416, #952, #24572, .T. ) ;
#30352 = AXIS2_PLACEMENT_3D ( 'NONE', #5495, #31655, #17450 ) ;
#30353 = CARTESIAN_POINT ( 'NONE',  ( -56.92336230271183695, 217.4189793300686233, 4.149950860017807663 ) ) ;
#30354 = CARTESIAN_POINT ( 'NONE',  ( 26.75643035624999655, 247.2343750006145058, 3.323476615752267271 ) ) ;
#30355 = DIRECTION ( 'NONE',  ( -0.000000000000000000, -1.000000000000000000, -0.000000000000000000 ) ) ;
#30356 = CARTESIAN_POINT ( 'NONE',  ( -42.47544563604517265, 213.3788001182224718, 3.209657149897419348 ) ) ;
#30357 = CARTESIAN_POINT ( 'NONE',  ( -8.962234695871760692, 140.3601862821014379, 8.715434833791933400 ) ) ;
#30358 = CARTESIAN_POINT ( 'NONE',  ( 15.47812160658635428, 6.148716598298411107, -10.19635144101486368 ) ) ;
#30359 = ORIENTED_EDGE ( 'NONE', *, *, #12928, .F. ) ;
#30360 = CARTESIAN_POINT ( 'NONE',  ( 18.00000000000000355, -5.196152422706632912, -5.324999999999996625 ) ) ;
#30361 = CARTESIAN_POINT ( 'NONE',  ( -15.46528703574804986, 114.1976862821014578, -3.257655550457287497 ) ) ;
#30362 = CARTESIAN_POINT ( 'NONE',  ( -46.04538769728823411, 212.3930949314662371, -8.469044688360781947 ) ) ;
#30363 = CARTESIAN_POINT ( 'NONE',  ( -7.954856959092191815, 114.7726862821014322, -5.529263428287477744 ) ) ;
#30364 = DIRECTION ( 'NONE',  ( 0.000000000000000000, -0.000000000000000000, 1.000000000000000000 ) ) ;
#30365 = CARTESIAN_POINT ( 'NONE',  ( 11.48171059495397728, 17.88518628210143646, 4.944772684328674117 ) ) ;
#30366 = CARTESIAN_POINT ( 'NONE',  ( 10.56230152254410548, 0.000000000000000000, -9.450000000000041922 ) ) ;
#30367 = VERTEX_POINT ( 'NONE', #22621 ) ;
#30368 = CARTESIAN_POINT ( 'NONE',  ( 20.99999999999999645, 0.000000000000000000, -8.000000000000000000 ) ) ;
#30369 = CARTESIAN_POINT ( 'NONE',  ( -8.152565276336710909, 85.44768628210142936, 5.233372021372435512 ) ) ;
#30370 =( BOUNDED_CURVE ( )  B_SPLINE_CURVE ( 2, ( #25458, #6057, #37010, #8913, #34176, #17834, #11054, #556, #34872 ),
 .UNSPECIFIED., .F., .F. ) 
 B_SPLINE_CURVE_WITH_KNOTS ( ( 3, 2, 2, 2, 3 ),
 ( 0.1630434782608695676, 0.1666666666666666574, 0.1739130434782608647, 0.1811594202898550721, 0.1847826086956521618 ),
 .UNSPECIFIED. ) 
 CURVE ( )  GEOMETRIC_REPRESENTATION_ITEM ( )  RATIONAL_B_SPLINE_CURVE ( ( 0.9330127018922194093, 0.9330127018922196314, 1.000000000000000000, 0.8660254037844387076, 1.000000000000000000, 0.8660254037844387076, 1.000000000000000000, 0.9330127018922196314, 0.9330127018922194093 ) ) 
 REPRESENTATION_ITEM ( '' )  );
#30371 = CYLINDRICAL_SURFACE ( 'NONE', #4855, 4.000000000000000888 ) ;
#30372 = CARTESIAN_POINT ( 'NONE',  ( 8.152565276336593669, 131.5523137178985564, 5.233372021372610483 ) ) ;
#30373 = AXIS2_PLACEMENT_3D ( 'NONE', #13733, #4994, #25092 ) ;
#30374 = CARTESIAN_POINT ( 'NONE',  ( 13.62178482187501416, 198.6031250006145399, 23.59362340125806767 ) ) ;
#30375 = DIRECTION ( 'NONE',  ( 1.000000000000000000, 0.000000000000000000, 0.000000000000000000 ) ) ;
#30376 = CARTESIAN_POINT ( 'NONE',  ( 27.24356964374999635, 197.8718750006145513, -15.72908226750539029 ) ) ;
#30377 = CARTESIAN_POINT ( 'NONE',  ( 17.00000000000000000, 4.898587196589406912E-16, 50.17464377163448574 ) ) ;
#30378 = CARTESIAN_POINT ( 'NONE',  ( 21.00000000000000355, 0.000000000000000000, 50.00000000000001421 ) ) ;
#30379 = CARTESIAN_POINT ( 'NONE',  ( 9.534712964251900402, 75.77731371789855075, 1.715153634034445540 ) ) ;
#30380 = ORIENTED_EDGE ( 'NONE', *, *, #15016, .T. ) ;
#30381 = VECTOR ( 'NONE', #23654, 1000.000000000000114 ) ;
#30382 = CARTESIAN_POINT ( 'NONE',  ( 15.00000000000000178, 244.2437500012290457, 3.464101615137757051 ) ) ;
#30383 = CARTESIAN_POINT ( 'NONE',  ( -2.311890736173447980, 87.27731371789856496, 12.53471296425189330 ) ) ;
#30384 = CARTESIAN_POINT ( 'NONE',  ( 10.31873187879411091, -3.604726614523244610, -5.109374999385544847 ) ) ;
#30385 = DIRECTION ( 'NONE',  ( -0.9933043639548644332, 0.1155267958017622554, 0.000000000000000000 ) ) ;
#30386 = CARTESIAN_POINT ( 'NONE',  ( 26.75643035624999655, 7.049594010296217766E-16, -4.528124999385485516 ) ) ;
#30387 = CARTESIAN_POINT ( 'NONE',  ( -10.49813415416004858, 51.62731371789855217, 7.228626920338839135 ) ) ;
#30388 = ORIENTED_EDGE ( 'NONE', *, *, #36803, .F. ) ;
#30389 = CARTESIAN_POINT ( 'NONE',  ( 20.99999999999999645, -6.646953231504538984, -7.228124999385454608 ) ) ;
#30390 = CARTESIAN_POINT ( 'NONE',  ( 15.24356964374999990, 244.7593750006145115, -3.323476615752268604 ) ) ;
#30391 = CARTESIAN_POINT ( 'NONE',  ( -4.622313124798576922, 14.43518628210144250, -11.61527771782819762 ) ) ;
#30392 = CARTESIAN_POINT ( 'NONE',  ( -34.75669563604516554, 209.8844732041982013, -6.500000000000000888 ) ) ;
#30393 = CARTESIAN_POINT ( 'NONE',  ( -54.54836230271182984, 204.3130714775002446, -3.149950860017828091 ) ) ;
#30394 =( LENGTH_UNIT ( ) NAMED_UNIT ( * ) SI_UNIT ( .MILLI., .METRE. ) );
#30395 = VECTOR ( 'NONE', #16295, 1000.000000000000000 ) ;
#30396 = CARTESIAN_POINT ( 'NONE',  ( 24.59253236524878616, -3.464101615137757051, 159.9051123081840160 ) ) ;
#30397 = CARTESIAN_POINT ( 'NONE',  ( -10.69584247140429412, 71.75231371789855928, -6.932735513424201024 ) ) ;
#30398 = CARTESIAN_POINT ( 'NONE',  ( -47.43080436395489841, 205.4999999999999716, -0.1155267958017894420 ) ) ;
#30399 = CARTESIAN_POINT ( 'NONE',  ( -60.29538769728823411, 211.8571965466039444, -6.469044688360768625 ) ) ;
#30400 = EDGE_CURVE ( 'NONE', #21723, #8971, #9074, .T. ) ;
#30401 = DIRECTION ( 'NONE',  ( 0.000000000000000000, 0.000000000000000000, 1.000000000000000000 ) ) ;
#30402 = CARTESIAN_POINT ( 'NONE',  ( 36.79526260918112257, -3.464101615137414214, 161.6983982847735888 ) ) ;
#30403 = CARTESIAN_POINT ( 'NONE',  ( -15.53471296425188442, 61.97731371789853938, -2.908627838312459080 ) ) ;
#30404 = CARTESIAN_POINT ( 'NONE',  ( -43.06919563604516554, 218.5000000000000000, -0.1155267958018185298 ) ) ;
#30405 = DIRECTION ( 'NONE',  ( -0.000000000000000000, 1.000000000000000000, -0.000000000000000000 ) ) ;
#30406 = CARTESIAN_POINT ( 'NONE',  ( -6.932735513423968321, 60.14768628210144641, -10.69584247140445221 ) ) ;
#30407 = CARTESIAN_POINT ( 'NONE',  ( -14.25334919248782306, 31.68518628210144428, -6.092822981423979378 ) ) ;
#30408 = FACE_BOUND ( 'NONE', #16339, .T. ) ;
#30409 = CARTESIAN_POINT ( 'NONE',  ( -28.40689544173954673, 204.5242310104925707, -5.838094896048071192 ) ) ;
#30410 = ORIENTED_EDGE ( 'NONE', *, *, #25721, .T. ) ;
#30411 = CARTESIAN_POINT ( 'NONE',  ( 3.257655550457285720, 33.69768628210143646, -15.46528703574804986 ) ) ;
#30412 = CARTESIAN_POINT ( 'NONE',  ( 27.24356964374999279, 196.9156250006145399, -15.72908226750539207 ) ) ;
#30413 = FACE_OUTER_BOUND ( 'NONE', #16872, .T. ) ;
#30414 =( BOUNDED_CURVE ( )  B_SPLINE_CURVE ( 2, ( #14053, #3036, #16900, #3224, #8731, #19938, #19757 ),
 .UNSPECIFIED., .F., .F. ) 
 B_SPLINE_CURVE_WITH_KNOTS ( ( 3, 2, 2, 3 ),
 ( 0.4130434782608723432, 0.4202898550724666338, 0.4275362318840610354, 0.4347826086956553260 ),
 .UNSPECIFIED. ) 
 CURVE ( )  GEOMETRIC_REPRESENTATION_ITEM ( )  RATIONAL_B_SPLINE_CURVE ( ( 0.9999999999999487077, 0.8660254037844899999, 1.000000000000000000, 0.8660254037844387076, 1.000000000000000000, 0.8660254037843801989, 1.000000000000058620 ) ) 
 REPRESENTATION_ITEM ( '' )  );
#30415 = DIRECTION ( 'NONE',  ( 0.000000000000000000, 1.000000000000000000, 0.000000000000000000 ) ) ;
#30416 = CARTESIAN_POINT ( 'NONE',  ( -33.57663769728823411, 204.3130714775002730, 3.149950860017883603 ) ) ;
#30417 = EDGE_CURVE ( 'NONE', #30424, #7705, #1314, .T. ) ;
#30418 = CARTESIAN_POINT ( 'NONE',  ( -7.946041369334237991, 195.0000000000000000, 26.05901981062767092 ) ) ;
#30419 = CARTESIAN_POINT ( 'NONE',  ( 12.50000000000000355, 17.31018628210144428, 0.1745138560725507937 ) ) ;
#30420 = LINE ( 'NONE', #33258, #3241 ) ;
#30421 = CARTESIAN_POINT ( 'NONE',  ( -9.534712964251895073, 126.3773137178985309, -1.715153634034446428 ) ) ;
#30422 = CARTESIAN_POINT ( 'NONE',  ( 26.75643035624999655, 244.7218750006145456, -3.323476615752271268 ) ) ;
#30423 = EDGE_CURVE ( 'NONE', #24827, #28622, #3751, .T. ) ;
#30424 = VERTEX_POINT ( 'NONE', #37368 ) ;
#30425 = CARTESIAN_POINT ( 'NONE',  ( 24.77555942491173369, 0.000000000000000000, 161.9971211729523475 ) ) ;
#30426 = DIRECTION ( 'NONE',  ( -0.000000000000000000, 1.000000000000000000, -0.000000000000000000 ) ) ;
#30427 = CARTESIAN_POINT ( 'NONE',  ( -10.69584247140429412, 136.1523137178985792, -6.932735513424201024 ) ) ;
#30428 = CARTESIAN_POINT ( 'NONE',  ( 22.80587116629410716, 7.646167579472015790E-16, -6.215624999385549465 ) ) ;
#30429 = CARTESIAN_POINT ( 'NONE',  ( 37.21194452064604974, -3.604726614523235284, 163.6664460787016253 ) ) ;
#30430 = CARTESIAN_POINT ( 'NONE',  ( 20.99999999999999645, 6.928203230275506996, -1.912500000000006306 ) ) ;
#30431 = CARTESIAN_POINT ( 'NONE',  ( -27.00000000000000355, 197.7125000000000057, -15.58845726811989429 ) ) ;
#30432 = CIRCLE ( 'NONE', #5010, 5.500000000000005329 ) ;
#30433 = EDGE_LOOP ( 'NONE', ( #1503, #15521, #16938 ) ) ;
#30434 = CARTESIAN_POINT ( 'NONE',  ( -11.48171059495397373, 31.68518628210144428, -4.944772684328680334 ) ) ;
#30435 = ORIENTED_EDGE ( 'NONE', *, *, #31453, .F. ) ;
#30436 = EDGE_LOOP ( 'NONE', ( #10280, #6280, #23242, #17964 ) ) ;
#30437 = DIRECTION ( 'NONE',  ( 0.000000000000000000, -1.000000000000000000, 0.000000000000000000 ) ) ;
#30438 = CARTESIAN_POINT ( 'NONE',  ( 25.25600545691528254, 0.000000000000000000, 167.4886444474074381 ) ) ;
#30439 = CARTESIAN_POINT ( 'NONE',  ( 23.99999999999999645, 249.4562500012290229, -5.196152422706631135 ) ) ;
#30440 = LINE ( 'NONE', #16224, #29926 ) ;
#30441 = CARTESIAN_POINT ( 'NONE',  ( 26.75643035624999655, 7.049594010296217766E-16, -9.365624999385479654 ) ) ;
#30442 = CARTESIAN_POINT ( 'NONE',  ( 0.1745138560725515708, 79.41018628210144925, -12.50000000000000355 ) ) ;
#30443 = CARTESIAN_POINT ( 'NONE',  ( -13.23911966647218463, 131.4476862821014436, 8.632099005475506459 ) ) ;
#30444 = EDGE_CURVE ( 'NONE', #30939, #17372, #6415, .T. ) ;
#30445 = CARTESIAN_POINT ( 'NONE',  ( 7.136082524518490011, 215.1989690533051487, 3.001545256184956934 ) ) ;
#30446 =( BOUNDED_CURVE ( )  B_SPLINE_CURVE ( 2, ( #9259, #7487, #18174, #3748, #21713, #6411, #32373 ),
 .UNSPECIFIED., .F., .F. ) 
 B_SPLINE_CURVE_WITH_KNOTS ( ( 3, 2, 2, 3 ),
 ( 0.3478260869565213409, 0.3550724637681154094, 0.3623188405797093670, 0.3695652173913033800 ),
 .UNSPECIFIED. ) 
 CURVE ( )  GEOMETRIC_REPRESENTATION_ITEM ( )  RATIONAL_B_SPLINE_CURVE ( ( 1.000000000000007105, 0.8660254037844313801, 1.000000000000000000, 0.8660254037844387076, 1.000000000000000000, 0.8660254037844561381, 0.9999999999999825695 ) ) 
 REPRESENTATION_ITEM ( '' )  );
#30447 = B_SPLINE_CURVE_WITH_KNOTS ( 'NONE', 3,
 ( #7587, #22185, #1887, #13458 ),
 .UNSPECIFIED., .F., .F.,
 ( 4, 4 ),
 ( 0.000000000000000000, 1.000000000000000000 ),
 .UNSPECIFIED. ) ;
#30448 = CARTESIAN_POINT ( 'NONE',  ( -58.70461230271184405, 208.6787018382582346, -4.469044688360757966 ) ) ;
#30449 =( NAMED_UNIT ( * ) PLANE_ANGLE_UNIT ( ) SI_UNIT ( $, .RADIAN. ) );
#30450 = CARTESIAN_POINT ( 'NONE',  ( 3.306546357697854128E-15, 200.0000000000000000, 27.00000000000000355 ) ) ;
#30451 = CARTESIAN_POINT ( 'NONE',  ( 37.19400013225104118, 3.464101615137755275, 166.2559890285434108 ) ) ;
#30452 = CARTESIAN_POINT ( 'NONE',  ( -7.228626920338836470, 127.5273137178985792, -10.49813415416005213 ) ) ;
#30453 = CARTESIAN_POINT ( 'NONE',  ( -51.98288769728821990, 203.5309553116391612, -1.857196546604028775 ) ) ;
#30454 = CARTESIAN_POINT ( 'NONE',  ( -56.93080436395490551, 201.5000000000000000, -0.1155267958017054536 ) ) ;
#30455 = EDGE_CURVE ( 'NONE', #11570, #9957, #11284, .T. ) ;
#30456 = APPLICATION_PROTOCOL_DEFINITION ( 'draft international standard', 'automotive_design', 1998, #346 ) ;
#30457 = CARTESIAN_POINT ( 'NONE',  ( 18.12178482187500350, -4.985214923628407568, -1.978124999385488803 ) ) ;
#30458 = CARTESIAN_POINT ( 'NONE',  ( 27.24356964375000700, 196.8406250006145513, 15.72908226750537075 ) ) ;
#30459 = CARTESIAN_POINT ( 'NONE',  ( 3.257655550456945548, 114.3023137178985422, 15.46528703574811736 ) ) ;
#30460 = CARTESIAN_POINT ( 'NONE',  ( -44.05877896937847993, 211.6261429550004607, -6.530955311639245586 ) ) ;
#30461 = EDGE_LOOP ( 'NONE', ( #9775, #31134, #10436, #36203, #1130, #7414, #35374, #19768, #9875, #29054, #25806, #14255, #12262, #34516, #19994, #37221, #34525, #22969, #20674, #1960, #31577, #34875, #25948, #24393, #13703, #8959, #15044, #14180, #15737, #34847, #10932, #2359, #14152, #22837, #19062, #1713, #5360 ) ) ;
#30462 = DIRECTION ( 'NONE',  ( -0.000000000000000000, -0.000000000000000000, 1.000000000000000000 ) ) ;
#30463 = CARTESIAN_POINT ( 'NONE',  ( 31.45868912971819142, 0.000000000000000000, 169.5433637710095809 ) ) ;
#30464 = CARTESIAN_POINT ( 'NONE',  ( -81.72704584564829133, 216.6260876520869658, -7.500000000000000000 ) ) ;
#30465 = CARTESIAN_POINT ( 'NONE',  ( 37.28875051894242887, 7.646167579472024665E-16, 164.5443426563950027 ) ) ;
#30466 = CARTESIAN_POINT ( 'NONE',  ( -13.23911966647218463, 85.44768628210142936, 8.632099005475506459 ) ) ;
#30467 = CARTESIAN_POINT ( 'NONE',  ( -55.54538769728823411, 211.8571965466040012, -6.469044688360769513 ) ) ;
#30468 = CARTESIAN_POINT ( 'NONE',  ( 16.56230152254411436, 7.209453229046475009, -3.853124999385534988 ) ) ;
#30469 = CARTESIAN_POINT ( 'NONE',  ( -6.594114490232312775, 32.26018628210145067, -6.840914352312096547 ) ) ;
#30470 = CARTESIAN_POINT ( 'NONE',  ( 18.00000000000000000, 5.196152422706630247, -2.718749998770947585 ) ) ;
#30471 = CARTESIAN_POINT ( 'NONE',  ( -40.10788769728823411, 218.4690446883607535, 2.393094931466250408 ) ) ;
#30472 = DIRECTION ( 'NONE',  ( 0.000000000000000000, 1.000000000000000000, 0.000000000000000000 ) ) ;
#30473 = CARTESIAN_POINT ( 'NONE',  ( -8.962234695871760692, 85.16018628210144925, 8.715434833791933400 ) ) ;
#30474 = CARTESIAN_POINT ( 'NONE',  ( 20.99999999999999645, -6.928203230275506996, -7.931249998770954157 ) ) ;
#30475 = CARTESIAN_POINT ( 'NONE',  ( -4.500000000000002665, 244.5000000000000000, 2.500000000000000000 ) ) ;
#30477 = CARTESIAN_POINT ( 'NONE',  ( 10.31873187879410736, 0.000000000000000000, -1.096874999385516469 ) ) ;
#30476 = CARTESIAN_POINT ( 'NONE',  ( 1.715153634034233487, 37.72268628210143504, 9.534712964251941258 ) ) ;
#30478 = CARTESIAN_POINT ( 'NONE',  ( 27.00000000000036593, -3.464101615137536783, -6.056249998770942611 ) ) ;
#30479 = VERTEX_POINT ( 'NONE', #29023 ) ;
#30480 = CARTESIAN_POINT ( 'NONE',  ( 24.00000000000000000, -5.196152422706629359, -3.000000000000002665 ) ) ;
#30481 = STYLED_ITEM ( 'NONE', ( #3108 ), #14238 ) ;
#30482 = CARTESIAN_POINT ( 'NONE',  ( 30.82381401619432992, -7.209453229046482114, 162.2867080177096852 ) ) ;
#30483 = CARTESIAN_POINT ( 'NONE',  ( 33.72823834632531259, 5.196152422706637353, 161.0632902835097013 ) ) ;
#30484 = CARTESIAN_POINT ( 'NONE',  ( 26.99999999999999645, 245.2750000000000057, -7.347880794884117764E-16 ) ) ;
#30485 = CARTESIAN_POINT ( 'NONE',  ( 5.649999999999987921, 244.5000000000000000, -2.499999999999999556 ) ) ;
#30486 = CARTESIAN_POINT ( 'NONE',  ( 11.61527771782809637, 76.06481371789855928, 4.622313124798827388 ) ) ;
#30487 = CARTESIAN_POINT ( 'NONE',  ( -10.69584247140444866, 85.44768628210144357, 6.932735513423972762 ) ) ;
#30488 = EDGE_LOOP ( 'NONE', ( #15425, #34000, #22462, #13829 ) ) ;
#30489 = VERTEX_POINT ( 'NONE', #25633 ) ;
#30490 = CARTESIAN_POINT ( 'NONE',  ( -26.99999999999998934, 198.3500000012290627, 15.58845726811991561 ) ) ;
#30491 = CARTESIAN_POINT ( 'NONE',  ( -27.00000000000000355, 196.8125000000000000, -15.58845726811989429 ) ) ;
#30492 = CARTESIAN_POINT ( 'NONE',  ( 10.83675517735179206, 65.13981371789854791, -11.08355503943118769 ) ) ;
#30493 = CARTESIAN_POINT ( 'NONE',  ( 15.24356964374999990, 3.323476615752268604, -7.490624999385497418 ) ) ;
#30494 = CARTESIAN_POINT ( 'NONE',  ( 15.24356964374999990, 244.4593750006145569, 0.000000000000000000 ) ) ;
#30495 = AXIS2_PLACEMENT_3D ( 'NONE', #36456, #36270, #25090 ) ;
#30496 = CARTESIAN_POINT ( 'NONE',  ( -52.97247103062156270, 207.6499508600178387, 3.839350919129076445 ) ) ;
#30497 = ADVANCED_FACE ( 'NONE', ( #26187 ), #37189, .T. ) ;
#30498 = CARTESIAN_POINT ( 'NONE',  ( 25.48152094116770883, 0.000000000000000000, 170.0662982274954800 ) ) ;
#30499 = CARTESIAN_POINT ( 'NONE',  ( -2.064181346179062349, 54.50231371789855928, -9.465287035748106703 ) ) ;
#30500 = CARTESIAN_POINT ( 'NONE',  ( 22.80587116629411071, -3.604726614523235284, -8.503124999385544669 ) ) ;
#30501 = CARTESIAN_POINT ( 'NONE',  ( -3.796722387233185003, 91.01481371789856212, -8.710071997420207879 ) ) ;
#30502 = CARTESIAN_POINT ( 'NONE',  ( 15.24356964374999990, 239.8468750006145171, 0.000000000000000000 ) ) ;
#30503 = CARTESIAN_POINT ( 'NONE',  ( -0.1745138560722763466, 27.18981371789855217, -12.50000000000000355 ) ) ;
#30504 = PRESENTATION_LAYER_ASSIGNMENT (  '', '', ( #825 ) ) ;
#30505 = CARTESIAN_POINT ( 'NONE',  ( -12.46528703574805697, 77.39768628210144641, -2.660918448318280838 ) ) ;
#30506 = CARTESIAN_POINT ( 'NONE',  ( 10.56230152254411436, 3.464101615137752166, -7.574999998771032139 ) ) ;
#30507 = VECTOR ( 'NONE', #26485, 1000.000000000000000 ) ;
#30508 = CARTESIAN_POINT ( 'NONE',  ( -47.00000000000000711, 244.5000000000000000, 5.000000000000000000 ) ) ;
#30509 = CARTESIAN_POINT ( 'NONE',  ( 36.98316069593346356, 3.604726614523238837, 161.0514349962108156 ) ) ;
#30510 = CARTESIAN_POINT ( 'NONE',  ( 10.31873187879411091, -3.604726614523244610, -6.009374999385537208 ) ) ;
#30511 = SURFACE_STYLE_FILL_AREA ( #12876 ) ;
#30512 = CARTESIAN_POINT ( 'NONE',  ( 1.120210788295102201E-13, 196.8500000012290343, -27.00000000000000711 ) ) ;
#30513 = CARTESIAN_POINT ( 'NONE',  ( 2.064181346179272847, 88.89768628210146062, -9.465287035748065847 ) ) ;
#30514 = CARTESIAN_POINT ( 'NONE',  ( 9.184850993605147944E-16, 141.0000000000000000, -7.500000000000000000 ) ) ;
#30515 = CARTESIAN_POINT ( 'NONE',  ( 2.660918448318279950, 134.8976862821014890, -12.46528703574805697 ) ) ;
#30516 = CARTESIAN_POINT ( 'NONE',  ( -6.406268989994019059, 143.0000000000000853, 10.69826447808074299 ) ) ;
#30517 = CARTESIAN_POINT ( 'NONE',  ( 21.00000000000000000, 249.5218750006145285, 6.646953231504538984 ) ) ;
#30518 = ORIENTED_EDGE ( 'NONE', *, *, #26598, .F. ) ;
#30519 = CARTESIAN_POINT ( 'NONE',  ( 27.85934967376930516, 5.407089921784856479, 164.2211893949991293 ) ) ;
#30520 = CARTESIAN_POINT ( 'NONE',  ( 18.12178482187499640, 4.985214923628404904, -4.265624999385458693 ) ) ;
#30521 = EDGE_CURVE ( 'NONE', #34832, #18566, #18047, .T. ) ;
#30522 = CARTESIAN_POINT ( 'NONE',  ( -1.926257025242585782E-15, 198.3968750006145285, -31.45816453501076637 ) ) ;
#30523 = CARTESIAN_POINT ( 'NONE',  ( 31.44888410865908313, 6.928203230275514990, 169.4312918674742434 ) ) ;
#30524 = CARTESIAN_POINT ( 'NONE',  ( -47.00000000000000711, 244.5000000000000000, 5.000000000000000000 ) ) ;
#30525 = CARTESIAN_POINT ( 'NONE',  ( 15.24356964375000167, 243.1468750006145285, 3.323476615752272600 ) ) ;
#30526 = CARTESIAN_POINT ( 'NONE',  ( -6.932735513424201912, 133.8523137178985678, 10.69584247140429412 ) ) ;
#30527 = CARTESIAN_POINT ( 'NONE',  ( 2.311890736173175753, 138.9226862821014663, 12.53471296425194659 ) ) ;
#30529 = ORIENTED_EDGE ( 'NONE', *, *, #4696, .T. ) ;
#30528 = ORIENTED_EDGE ( 'NONE', *, *, #22083, .F. ) ;
#30530 = VECTOR ( 'NONE', #24364, 1000.000000000000000 ) ;
#30531 = CARTESIAN_POINT ( 'NONE',  ( -56.70466238434234185, 244.2363183625454894, -2.499999999999996447 ) ) ;
#30532 = CARTESIAN_POINT ( 'NONE',  ( 15.24356964375000167, 243.9343750006145228, 3.323476615752272600 ) ) ;
#30533 = FACE_BOUND ( 'NONE', #28003, .T. ) ;
#30534 = CIRCLE ( 'NONE', #15318, 25.00000000000000000 ) ;
#30535 = CARTESIAN_POINT ( 'NONE',  ( 26.75643035624999655, 3.323476615752271712, -3.928124999385464999 ) ) ;
#30536 = CARTESIAN_POINT ( 'NONE',  ( 8.927990412390371944, 104.5273137178985650, 13.04141134922778811 ) ) ;
#30538 = LINE ( 'NONE', #4923, #7110 ) ;
#30537 = MECHANICAL_DESIGN_GEOMETRIC_PRESENTATION_REPRESENTATION (  '', ( #1459 ), #14183 ) ;
#30539 = CARTESIAN_POINT ( 'NONE',  ( 26.99999999999999645, -3.464101615137751278, -8.756249998770950782 ) ) ;
#30540 = ORIENTED_EDGE ( 'NONE', *, *, #10065, .T. ) ;
#30541 = CARTESIAN_POINT ( 'NONE',  ( 22.80587116629411781, 3.604726614523243278, -5.334374999385495641 ) ) ;
#30542 = VERTEX_POINT ( 'NONE', #16504 ) ;
#30543 = CARTESIAN_POINT ( 'NONE',  ( -27.24356964374999990, 196.1656250006145399, -15.72908226750537786 ) ) ;
#30544 = CARTESIAN_POINT ( 'NONE',  ( 0.1745138560725515708, 134.6101862821014663, -12.50000000000000355 ) ) ;
#30545 = CARTESIAN_POINT ( 'NONE',  ( -31.00000000000003553, 209.9999999999999716, -6.500000000000000888 ) ) ;
#30546 = CARTESIAN_POINT ( 'NONE',  ( 36.89654967657799745, 7.646167579472024665E-16, 160.0614665149821576 ) ) ;
#30547 = CARTESIAN_POINT ( 'NONE',  ( -54.94419563604517265, 201.5000000000000000, 0.1155267958018195706 ) ) ;
#30548 = CARTESIAN_POINT ( 'NONE',  ( 15.24356964374999990, 247.4968750006145228, 0.000000000000000000 ) ) ;
#30549 = DIRECTION ( 'NONE',  ( 0.000000000000000000, 0.000000000000000000, 1.000000000000000000 ) ) ;
#30550 = DIRECTION ( 'NONE',  ( 0.000000000000000000, 0.000000000000000000, -1.000000000000000000 ) ) ;
#30551 = CARTESIAN_POINT ( 'NONE',  ( -32.97544563604516554, 213.3788001182224718, 3.209657149897419348 ) ) ;
#30552 = CARTESIAN_POINT ( 'NONE',  ( -6.932735513423968321, 133.7476862821014549, -10.69584247140445221 ) ) ;
#30553 = CARTESIAN_POINT ( 'NONE',  ( 22.56230152254410370, 7.347880794884117764E-16, -1.912499998771022280 ) ) ;
#30554 = ORIENTED_EDGE ( 'NONE', *, *, #7478, .F. ) ;
#30555 = CARTESIAN_POINT ( 'NONE',  ( -27.00000000000000355, 195.1625000012290343, 0.000000000000000000 ) ) ;
#30556 = CARTESIAN_POINT ( 'NONE',  ( 10.56230152254410548, 0.000000000000000000, -9.000000000000035527 ) ) ;
#30557 = CARTESIAN_POINT ( 'NONE',  ( -10.83675517735155047, 124.2601862821014578, -11.08355503943142750 ) ) ;
#30558 = CARTESIAN_POINT ( 'NONE',  ( -9.534712964251941258, 113.6226862821014549, 1.715153634034234154 ) ) ;
#30559 = EDGE_CURVE ( 'NONE', #19776, #20032, #30538, .T. ) ;
#30560 = CARTESIAN_POINT ( 'NONE',  ( 2.999999999999997335, 237.0000000000000000, -2.500000000000000000 ) ) ;
#30561 = CARTESIAN_POINT ( 'NONE',  ( -10.69584247140444866, 11.84768628210144925, 6.932735513423972762 ) ) ;
#30562 = CARTESIAN_POINT ( 'NONE',  ( 13.56230152254411792, -5.196152422706638241, -8.925000000000071765 ) ) ;
#30563 = VERTEX_POINT ( 'NONE', #5114 ) ;
#30564 = DIRECTION ( 'NONE',  ( -0.000000000000000000, -1.000000000000000000, -0.000000000000000000 ) ) ;
#30565 = CARTESIAN_POINT ( 'NONE',  ( 9.534712964251941258, 81.42268628210145209, -1.715153634034235708 ) ) ;
#30566 = CARTESIAN_POINT ( 'NONE',  ( 22.60769515458672885, 244.0736538117967029, -5.999999999999998224 ) ) ;
#30567 = CARTESIAN_POINT ( 'NONE',  ( -7.954856959092309943, 125.2273137178985394, 5.529263428287300108 ) ) ;
#30568 = EDGE_CURVE ( 'NONE', #33602, #30621, #13948, .T. ) ;
#30569 = CARTESIAN_POINT ( 'NONE',  ( -1.926257025242585782E-15, 196.0906250006145228, -31.45816453501075927 ) ) ;
#30570 = CARTESIAN_POINT ( 'NONE',  ( 20.99999999999995026, 242.7437500012290741, -5.999999999999998224 ) ) ;
#30571 = CARTESIAN_POINT ( 'NONE',  ( 27.24356964375000700, 199.1468750006145285, 15.72908226750537075 ) ) ;
#30572 = CARTESIAN_POINT ( 'NONE',  ( 25.05010001456683710, 0.000000000000000000, 165.1351344719413419 ) ) ;
#30573 = EDGE_CURVE ( 'NONE', #35447, #18087, #22241, .T. ) ;
#30574 = DIRECTION ( 'NONE',  ( 0.000000000000000000, 0.000000000000000000, 1.000000000000000000 ) ) ;
#30575 = CARTESIAN_POINT ( 'NONE',  ( 5.529263428287300108, 58.52731371789855785, 7.954856959092309943 ) ) ;
#30576 = ORIENTED_EDGE ( 'NONE', *, *, #33218, .T. ) ;
#30577 = CARTESIAN_POINT ( 'NONE',  ( 18.00000000000000355, 240.6812500012290457, 5.196152422706632912 ) ) ;
#30578 = CARTESIAN_POINT ( 'NONE',  ( -2.311890736173447980, 78.07731371789856212, 12.53471296425189330 ) ) ;
#30579 = CARTESIAN_POINT ( 'NONE',  ( 13.44051670066910731, 5.407089921784862696, -5.221874999385534011 ) ) ;
#30580 = CARTESIAN_POINT ( 'NONE',  ( 13.62178482187499640, 199.6531250006145228, -23.59362340125807123 ) ) ;
#30581 = CARTESIAN_POINT ( 'NONE',  ( 26.75643035624999655, -3.323476615752267715, -6.365624999385492089 ) ) ;
#30582 = CARTESIAN_POINT ( 'NONE',  ( 12.53471296425189330, 20.57731371789854435, 2.311890736173451977 ) ) ;
#30583 = ORIENTED_EDGE ( 'NONE', *, *, #26822, .T. ) ;
#30584 = CARTESIAN_POINT ( 'NONE',  ( 15.24356964374999990, 0.000000000000000000, -7.790624999385459049 ) ) ;
#30585 = CARTESIAN_POINT ( 'NONE',  ( -4.622313124798576922, 23.63518628210144357, -11.61527771782819762 ) ) ;
#30586 = CARTESIAN_POINT ( 'NONE',  ( 25.18249928241153413, 0.000000000000000000, 169.4431132759913794 ) ) ;
#30587 = AXIS2_PLACEMENT_3D ( 'NONE', #33907, #37477, #19894 ) ;
#30588 = CARTESIAN_POINT ( 'NONE',  ( -60.28794563604516554, 205.3262412349647832, 4.842901733360250205 ) ) ;
#30589 = DIRECTION ( 'NONE',  ( 0.08715574274765143514, 0.000000000000000000, -0.9961946980917461003 ) ) ;
#30590 = CARTESIAN_POINT ( 'NONE',  ( -6.932735513424201912, 60.25231371789855217, 10.69584247140429412 ) ) ;
#30591 = CARTESIAN_POINT ( 'NONE',  ( -48.22247103062156981, 207.6499508600178387, 3.839350919129076445 ) ) ;
#30592 = CARTESIAN_POINT ( 'NONE',  ( -63.65997103062156981, 215.5714017266979852, 3.350049139982118618 ) ) ;
#30593 = CARTESIAN_POINT ( 'NONE',  ( 18.91026388320226914, 5.440443521936087379, -7.988398020327252880 ) ) ;
#30594 = CARTESIAN_POINT ( 'NONE',  ( -8.871229729697644117, 219.1703717126474089, -3.236093818008944467 ) ) ;
#30595 = CARTESIAN_POINT ( 'NONE',  ( -13.23911966647199812, 34.95231371789854080, -8.632099005475788900 ) ) ;
#30596 = CARTESIAN_POINT ( 'NONE',  ( -44.25669563604517265, 209.8844732041981729, -8.500000000000003553 ) ) ;
#30597 =( BOUNDED_CURVE ( )  B_SPLINE_CURVE ( 2, ( #11935, #23138, #20485, #25081, #28804, #34680, #8725 ),
 .UNSPECIFIED., .F., .F. ) 
 B_SPLINE_CURVE_WITH_KNOTS ( ( 3, 2, 2, 3 ),
 ( 0.7826086956521710603, 0.7898550724637652953, 0.7971014492753596414, 0.8043478260869539875 ),
 .UNSPECIFIED. ) 
 CURVE ( )  GEOMETRIC_REPRESENTATION_ITEM ( )  RATIONAL_B_SPLINE_CURVE ( ( 1.000000000000053291, 0.8660254037843853059, 1.000000000000000000, 0.8660254037844387076, 1.000000000000000000, 0.8660254037844858921, 0.9999999999999528155 ) ) 
 REPRESENTATION_ITEM ( '' )  );
#30598 = CARTESIAN_POINT ( 'NONE',  ( 27.00000000000001421, 199.7375000000000114, 15.58845726811988897 ) ) ;
#30599 = CARTESIAN_POINT ( 'NONE',  ( 12.50000000000000355, 72.51018628210145778, 0.1745138560725507937 ) ) ;
#30600 = CARTESIAN_POINT ( 'NONE',  ( 2.908627838312118019, 10.12268628210144428, 15.53471296425195369 ) ) ;
#30601 = CARTESIAN_POINT ( 'NONE',  ( 22.56230152254412857, -3.464101615137755275, -2.062499999999993339 ) ) ;
#30602 = CARTESIAN_POINT ( 'NONE',  ( 19.39230484541324273, 244.2986538117967257, 5.999999999999987566 ) ) ;
#30603 = ORIENTED_EDGE ( 'NONE', *, *, #11723, .F. ) ;
#30604 = CARTESIAN_POINT ( 'NONE',  ( -2.908627838312119351, 23.92268628210143788, -15.53471296425195369 ) ) ;
#30605 = CARTESIAN_POINT ( 'NONE',  ( 27.24356964375000345, 196.8781250006145171, -3.336375036156643733E-15 ) ) ;
#30606 = CARTESIAN_POINT ( 'NONE',  ( 5.778771075727756162E-15, 197.2718750006145569, 31.45816453501075927 ) ) ;
#30607 = CARTESIAN_POINT ( 'NONE',  ( 27.84912036836594140, -5.196152422706638241, 162.7069437753488046 ) ) ;
#30608 = CARTESIAN_POINT ( 'NONE',  ( 22.56230152254410015, 7.347880794884117764E-16, -7.762499998770988618 ) ) ;
#30609 = CARTESIAN_POINT ( 'NONE',  ( 21.00000000000000000, 240.2687500012290513, 5.999999999999998224 ) ) ;
#30610 = AXIS2_PLACEMENT_3D ( 'NONE', #9031, #5992, #12242 ) ;
#30611 = CARTESIAN_POINT ( 'NONE',  ( 15.24356964375000167, 247.1968750006145115, 3.323476615752272600 ) ) ;
#30612 = CARTESIAN_POINT ( 'NONE',  ( -6.594114490232462877, 106.5398137178985536, 6.840914352311949109 ) ) ;
#30613 = CARTESIAN_POINT ( 'NONE',  ( 20.99999999999999645, 243.4468750006145399, -6.646953231504538984 ) ) ;
#30614 = ORIENTED_EDGE ( 'NONE', *, *, #24095, .T. ) ;
#30615 =( NAMED_UNIT ( * ) SI_UNIT ( $, .STERADIAN. ) SOLID_ANGLE_UNIT ( ) );
#30616 = CYLINDRICAL_SURFACE ( 'NONE', #24715, 5.999999999999999112 ) ;
#30617 = CARTESIAN_POINT ( 'NONE',  ( 13.44051670066911619, -5.407089921784859143, -9.065624999385569538 ) ) ;
#30618 = CARTESIAN_POINT ( 'NONE',  ( 27.87242303518145548, -5.407089921784859143, 164.3706185997128841 ) ) ;
#30619 = CARTESIAN_POINT ( 'NONE',  ( 36.90638618107669799, 7.347880794884125653E-16, 162.9685465236163111 ) ) ;
#30620 = CARTESIAN_POINT ( 'NONE',  ( -13.49999999999998401, 198.7250000000000227, 23.38268590217985476 ) ) ;
#30621 = VERTEX_POINT ( 'NONE', #2087 ) ;
#30622 = CARTESIAN_POINT ( 'NONE',  ( 12.53471296425194659, 35.42268628210144499, -2.311890736173178418 ) ) ;
#30623 = EDGE_LOOP ( 'NONE', ( #28726, #32973, #14951, #1938, #17141, #783 ) ) ;
#30624 = ORIENTED_EDGE ( 'NONE', *, *, #36935, .F. ) ;
#30625 = CARTESIAN_POINT ( 'NONE',  ( 23.99999999999999645, 5.196152422706631135, -5.043749998770941545 ) ) ;
#30626 = CARTESIAN_POINT ( 'NONE',  ( 22.56230152254410370, 0.000000000000000000, -10.00000000000000000 ) ) ;
#30627 = CARTESIAN_POINT ( 'NONE',  ( 24.89321967762106169, 0.000000000000000000, 163.3419840153761982 ) ) ;
#30628 = CARTESIAN_POINT ( 'NONE',  ( -1.045839947578415010E-13, 195.1625000000000512, 27.00000000000000355 ) ) ;
#30629 = CARTESIAN_POINT ( 'NONE',  ( 18.12178482187500350, -4.985214923628407568, -9.965624999385468641 ) ) ;
#30630 = CARTESIAN_POINT ( 'NONE',  ( -2.311890736173176641, 69.92268628210146630, -12.53471296425194836 ) ) ;
#30631 = CARTESIAN_POINT ( 'NONE',  ( -11.08355503943142573, 140.3601862821014663, 10.83675517735155402 ) ) ;
#30632 = CARTESIAN_POINT ( 'NONE',  ( -62.46502896937850124, 215.5714017266979567, -3.350049139982168800 ) ) ;
#30633 = CARTESIAN_POINT ( 'NONE',  ( 15.81961138684334678, 215.1803886131542640, 3.965927053047088258 ) ) ;
#30634 = CARTESIAN_POINT ( 'NONE',  ( -59.10044563604517265, 206.6211998817775566, -3.209657149897419348 ) ) ;
#30635 = CARTESIAN_POINT ( 'NONE',  ( 37.15478004801459377, 3.464101615137755275, 165.8077014144021462 ) ) ;
#30636 = CARTESIAN_POINT ( 'NONE',  ( -4.944772684328424539, 118.6148137178985564, -11.48171059495408031 ) ) ;
#30637 = CARTESIAN_POINT ( 'NONE',  ( -47.03497103062156981, 204.4285982733020148, -3.350049139982115509 ) ) ;
#30638 = CARTESIAN_POINT ( 'NONE',  ( -53.17038769728823411, 207.6069050685337913, 8.469044688360781947 ) ) ;
#30639 = VECTOR ( 'NONE', #2988, 1000.000000000000114 ) ;
#30640 = CARTESIAN_POINT ( 'NONE',  ( 26.75643035624999655, 3.323476615752271268, -2.690624999385500704 ) ) ;
#30641 = CARTESIAN_POINT ( 'NONE',  ( -27.24356964374999990, 195.2656250006145342, -15.72908226750537786 ) ) ;
#30642 = CARTESIAN_POINT ( 'NONE',  ( -6.092822981423666739, 100.2148137178985650, -14.25334919248795096 ) ) ;
#30643 = CARTESIAN_POINT ( 'NONE',  ( -40.89211230271181563, 203.5309553116391612, 1.857196546604092280 ) ) ;
#30644 = ORIENTED_EDGE ( 'NONE', *, *, #18712, .F. ) ;
#30645 =( BOUNDED_CURVE ( )  B_SPLINE_CURVE ( 2, ( #6304, #17875, #23183, #29420, #20154, #28664, #2701, #3454, #5731 ),
 .UNSPECIFIED., .F., .F. ) 
 B_SPLINE_CURVE_WITH_KNOTS ( ( 3, 2, 2, 2, 3 ),
 ( 0.1458333333333333426, 0.1527777777777777901, 0.1666666666666666574, 0.1805555555555555525, 0.1875000000000000000 ),
 .UNSPECIFIED. ) 
 CURVE ( )  GEOMETRIC_REPRESENTATION_ITEM ( )  RATIONAL_B_SPLINE_CURVE ( ( 0.9330127018922194093, 0.9330127018922194093, 1.000000000000000000, 0.8660254037844387076, 1.000000000000000000, 0.8660254037844387076, 1.000000000000000000, 0.9330127018922194093, 0.9330127018922194093 ) ) 
 REPRESENTATION_ITEM ( '' )  );
#30646 = CYLINDRICAL_SURFACE ( 'NONE', #29525, 5.999999999999999112 ) ;
#30647 = CARTESIAN_POINT ( 'NONE',  ( 8.715434833791931624, 119.6601862821014493, 8.962234695871760692 ) ) ;
#30648 = CARTESIAN_POINT ( 'NONE',  ( -11.08355503943142573, 75.96018628210144641, 10.83675517735155402 ) ) ;
#30649 = CARTESIAN_POINT ( 'NONE',  ( 28.12039261777511356, 5.196152422706630247, 165.8075997743837604 ) ) ;
#30650 = CARTESIAN_POINT ( 'NONE',  ( 27.89366724747619131, 5.407089921784862696, 164.6134410573727678 ) ) ;
#30651 = CARTESIAN_POINT ( 'NONE',  ( -14.38691631536207183, 76.53518628210146346, 5.770363421893814682 ) ) ;
#30652 = CIRCLE ( 'NONE', #19168, 5.000000000000000000 ) ;
#30653 = CARTESIAN_POINT ( 'NONE',  ( -55.14955436395489130, 214.8429017333601792, -4.673758765035197271 ) ) ;
#30654 = CARTESIAN_POINT ( 'NONE',  ( 22.80587116629411781, 3.604726614523238837, -4.378124999385524241 ) ) ;
#30655 = CARTESIAN_POINT ( 'NONE',  ( -5.233372021372430183, 32.54768628210143788, -8.152565276336710909 ) ) ;
#30656 = CARTESIAN_POINT ( 'NONE',  ( 19.39230484541324628, 246.3075961894322745, -5.999999999999989342 ) ) ;
#30657 = CARTESIAN_POINT ( 'NONE',  ( -69.99330436395490551, 210.1155267958017134, -6.500000000000000888 ) ) ;
#30658 = DIRECTION ( 'NONE',  ( 0.000000000000000000, 1.000000000000000000, 0.000000000000000000 ) ) ;
#30659 = CARTESIAN_POINT ( 'NONE',  ( -12.50000000000000355, 49.51018628210145067, -0.1745138560725492671 ) ) ;
#30660 = DIRECTION ( 'NONE',  ( -0.000000000000000000, -0.000000000000000000, 1.000000000000000000 ) ) ;
#30662 = CARTESIAN_POINT ( 'NONE',  ( 10.31873187879410736, 3.604726614523240613, -1.584374999385509630 ) ) ;
#30661 = CARTESIAN_POINT ( 'NONE',  ( -6.594114490232312775, 41.46018628210145351, -6.840914352312096547 ) ) ;
#30663 = DIRECTION ( 'NONE',  ( 0.000000000000000000, 0.000000000000000000, 1.000000000000000000 ) ) ;
#30664 = EDGE_LOOP ( 'NONE', ( #34644, #10310, #3118 ) ) ;
#30665 = CARTESIAN_POINT ( 'NONE',  ( 15.00000000000000000, 0.000000000000000000, -1.349999999999990097 ) ) ;
#30666 = CARTESIAN_POINT ( 'NONE',  ( 37.05343001352376575, 7.646167579472024665E-16, 161.8546169715473013 ) ) ;
#30667 = CARTESIAN_POINT ( 'NONE',  ( 24.77229108455869522, 3.464101615137757051, 161.9597638717739017 ) ) ;
#30668 = CARTESIAN_POINT ( 'NONE',  ( 24.00000000000000000, 245.6500000000000057, 5.196152422706629359 ) ) ;
#30669 = CYLINDRICAL_SURFACE ( 'NONE', #30670, 6.000000000000001776 ) ;
#30670 = AXIS2_PLACEMENT_3D ( 'NONE', #27818, #7730, #13235 ) ;
#30671 =( BOUNDED_CURVE ( )  B_SPLINE_CURVE ( 2, ( #5018, #33838, #16410, #13004, #10339, #21727, #21544 ),
 .UNSPECIFIED., .F., .F. ) 
 B_SPLINE_CURVE_WITH_KNOTS ( ( 3, 2, 2, 3 ),
 ( 0.6956521739130424598, 0.7028985507246365838, 0.7101449275362308189, 0.7173913043478248319 ),
 .UNSPECIFIED. ) 
 CURVE ( )  GEOMETRIC_REPRESENTATION_ITEM ( )  RATIONAL_B_SPLINE_CURVE ( ( 1.000000000000018430, 0.8660254037844202779, 1.000000000000000000, 0.8660254037844387076, 1.000000000000000000, 0.8660254037844612451, 0.9999999999999774625 ) ) 
 REPRESENTATION_ITEM ( '' )  );
#30672 = CARTESIAN_POINT ( 'NONE',  ( 2.311890736173452865, 91.87731371789855928, -12.53471296425189152 ) ) ;
#30673 = CARTESIAN_POINT ( 'NONE',  ( 11.61527771782819940, 90.33518628210144641, -4.622313124798573369 ) ) ;
#30674 = ORIENTED_EDGE ( 'NONE', *, *, #24687, .T. ) ;
#30675 = VERTEX_POINT ( 'NONE', #13661 ) ;
#30676 = CARTESIAN_POINT ( 'NONE',  ( -13.49999999999998401, 198.3875000012290286, 23.38268590217985476 ) ) ;
#30677 = CARTESIAN_POINT ( 'NONE',  ( -13.04141134922778456, 60.82731371789854080, 8.927990412390377273 ) ) ;
#30678 = CARTESIAN_POINT ( 'NONE',  ( 23.87821517812500005, -4.985214923628404016, -6.853124999385479477 ) ) ;
#30679 = CARTESIAN_POINT ( 'NONE',  ( 26.75643035624999655, 244.1968750006145399, 3.323476615752267715 ) ) ;
#30680 = CARTESIAN_POINT ( 'NONE',  ( -58.90997103062156981, 213.8393509191290889, 2.350049139982164359 ) ) ;
#30681 = AXIS2_PLACEMENT_3D ( 'NONE', #30463, #35234, #11930 ) ;
#30682 = CARTESIAN_POINT ( 'NONE',  ( 20.99999999999999645, 185.0294372515228645, -5.999999999999999112 ) ) ;
#30683 = CARTESIAN_POINT ( 'NONE',  ( 0.1745138560723095977, 40.98981371789854933, 9.500000000000005329 ) ) ;
#30684 = CARTESIAN_POINT ( 'NONE',  ( 22.80587116629410360, 3.604726614523238837, -8.428124999385516958 ) ) ;
#30685 = ADVANCED_FACE ( 'NONE', ( #36387 ), #7783, .T. ) ;
#30686 = CARTESIAN_POINT ( 'NONE',  ( -9.465287035748106703, 98.20231371789854791, 2.064181346179061460 ) ) ;
#30687 = CARTESIAN_POINT ( 'NONE',  ( 13.62178482187499640, 198.8093750006145513, -23.59362340125807123 ) ) ;
#30688 = CARTESIAN_POINT ( 'NONE',  ( -2.311890736173448424, 22.87731371789854151, 12.53471296425189330 ) ) ;
#30689 = CARTESIAN_POINT ( 'NONE',  ( 2.311890736173175753, 74.52268628210146062, 12.53471296425194836 ) ) ;
#30690 = CARTESIAN_POINT ( 'NONE',  ( 19.56230152254410370, 5.196152422706631135, -8.587499998771008336 ) ) ;
#30691 = ADVANCED_FACE ( 'NONE', ( #24834 ), #25213, .T. ) ;
#30692 = LINE ( 'NONE', #4709, #1385 ) ;
#30693 = CARTESIAN_POINT ( 'NONE',  ( 24.63505227327785363, 3.604726614523236616, 163.1857653286025709 ) ) ;
#30694 = CARTESIAN_POINT ( 'NONE',  ( 26.99999999999999645, 3.464101615137755275, -0.5812499987709716098 ) ) ;
#30695 = CARTESIAN_POINT ( 'NONE',  ( 19.68408634441912142, -5.407089921784861808, -7.246874999385532590 ) ) ;
#30696 = CARTESIAN_POINT ( 'NONE',  ( -77.00000000000002842, 210.0000000000000000, 3.000000000000000000 ) ) ;
#30697 = CARTESIAN_POINT ( 'NONE',  ( 9.465287035748067623, 100.3976862821014606, 2.064181346179272847 ) ) ;
#30698 = DIRECTION ( 'NONE',  ( -0.000000000000000000, -1.000000000000000000, -0.000000000000000000 ) ) ;
#30699 = CARTESIAN_POINT ( 'NONE',  ( -7.228626920339069173, 130.8726862821014834, 10.49813415415989581 ) ) ;
#30700 = CARTESIAN_POINT ( 'NONE',  ( -6.962373209266437435, 142.9999999999999716, 9.648466868844547406 ) ) ;
#30701 = CARTESIAN_POINT ( 'NONE',  ( 21.00000000000000000, 240.8593750006145342, 6.646953231504538984 ) ) ;
#30702 = VERTEX_POINT ( 'NONE', #36764 ) ;
#30703 = CARTESIAN_POINT ( 'NONE',  ( 24.83768937516613917, -3.604726614523240613, 165.5019180016658993 ) ) ;
#30704 = CARTESIAN_POINT ( 'NONE',  ( 21.00000000000000000, 6.646953231504538984, -6.103124999385481253 ) ) ;
#30705 = AXIS2_PLACEMENT_3D ( 'NONE', #5166, #21690, #2138 ) ;
#30706 = EDGE_CURVE ( 'NONE', #11580, #28711, #29426, .T. ) ;
#30707 = CARTESIAN_POINT ( 'NONE',  ( -27.24356964374999279, 198.9968750006145513, 15.72908226750539384 ) ) ;
#30708 = CARTESIAN_POINT ( 'NONE',  ( 16.83508850220853148, 4.102936442506299741, -8.000000000000000000 ) ) ;
#30709 = CARTESIAN_POINT ( 'NONE',  ( 31.40966402442264283, 6.928203230275514990, 168.9830042533329504 ) ) ;
#30710 = CARTESIAN_POINT ( 'NONE',  ( 20.99999999999999645, 243.8125000000000284, 5.999999999999998224 ) ) ;
#30711 = CARTESIAN_POINT ( 'NONE',  ( 15.24356964375000167, 242.2468750006145228, 3.323476615752272600 ) ) ;
#30712 = LINE ( 'NONE', #1698, #5748 ) ;
#30713 = CARTESIAN_POINT ( 'NONE',  ( -5.529263428287297444, 7.927313717898536005, -7.954856959092311719 ) ) ;
#30714 = CARTESIAN_POINT ( 'NONE',  ( 27.24356964375000345, 195.5843750006145285, -3.336375036156643733E-15 ) ) ;
#30716 = ORIENTED_EDGE ( 'NONE', *, *, #19236, .T. ) ;
#30715 = ORIENTED_EDGE ( 'NONE', *, *, #33294, .F. ) ;
#30717 = CARTESIAN_POINT ( 'NONE',  ( 18.12178482187500350, 244.8718750006145228, 4.985214923628407568 ) ) ;
#30718 = CARTESIAN_POINT ( 'NONE',  ( 4.622313124798831829, 9.364813717898545775, -11.61527771782809282 ) ) ;
#30719 = CARTESIAN_POINT ( 'NONE',  ( 23.87821517812499650, 4.985214923628404904, -3.440624999385466509 ) ) ;
#30720 = CARTESIAN_POINT ( 'NONE',  ( 13.23911966647199812, 103.9523137178985763, 8.632099005475788900 ) ) ;
#30721 = CARTESIAN_POINT ( 'NONE',  ( 19.56230152254412147, -5.196152422706635576, -0.3000000000000779821 ) ) ;
#30722 = CARTESIAN_POINT ( 'NONE',  ( 15.00000000000000178, -3.464101615137757051, -9.806249998770931953 ) ) ;
#30723 = CARTESIAN_POINT ( 'NONE',  ( 16.56230152254411081, -7.209453229046482114, -8.184374999385489957 ) ) ;
#30724 = EDGE_LOOP ( 'NONE', ( #35090, #6179 ) ) ;
#30725 = CARTESIAN_POINT ( 'NONE',  ( 13.49999999999999645, 199.5125000012290286, -23.38268590217984766 ) ) ;
#30726 = CARTESIAN_POINT ( 'NONE',  ( 10.49813415415989581, 110.1726862821014521, 7.228626920339068285 ) ) ;
#30727 = CARTESIAN_POINT ( 'NONE',  ( 16.56230152254411436, 7.209453229046475009, -1.603124999385524108 ) ) ;
#30728 = CARTESIAN_POINT ( 'NONE',  ( -59.10044563604517265, 203.6929966515019430, -6.137860380172892150 ) ) ;
#30729 = CARTESIAN_POINT ( 'NONE',  ( 23.87821517812499650, 244.6468750006145285, -4.985214923628404904 ) ) ;
#30730 = VECTOR ( 'NONE', #2618, 1000.000000000000000 ) ;
#30731 = PLANE ( 'NONE',  #18842 ) ;
#30732 = EDGE_CURVE ( 'NONE', #28398, #21699, #18297, .T. ) ;
#30733 = CARTESIAN_POINT ( 'NONE',  ( -65.43377896937850835, 208.3738570449995109, 6.530955311639247363 ) ) ;
#30734 = CARTESIAN_POINT ( 'NONE',  ( 18.00000000000000355, 246.0250000000000057, 5.196152422706632912 ) ) ;
#30735 = CARTESIAN_POINT ( 'NONE',  ( 16.56230152254411081, -6.928203230275506996, -0.6749999987709800475 ) ) ;
#30736 = ORIENTED_EDGE ( 'NONE', *, *, #33797, .F. ) ;
#30737 = CARTESIAN_POINT ( 'NONE',  ( 15.00000000000000000, 0.000000000000000000, -5.399999999999987921 ) ) ;
#30738 = CARTESIAN_POINT ( 'NONE',  ( 10.56230152254491195, -3.464101615138220236, -8.962500000000034106 ) ) ;
#30739 = CARTESIAN_POINT ( 'NONE',  ( 14.38691631536207538, 127.1351862821014720, -5.770363421893813793 ) ) ;
#30740 = EDGE_CURVE ( 'NONE', #23956, #10660, #16879, .T. ) ;
#30741 = DIRECTION ( 'NONE',  ( 0.000000000000000000, 0.000000000000000000, -1.000000000000000000 ) ) ;
#30742 = CARTESIAN_POINT ( 'NONE',  ( 0.1745138560725515708, 5.810186282101447830, -12.50000000000000355 ) ) ;
#30743 = CARTESIAN_POINT ( 'NONE',  ( 10.56230152254410903, -3.464101615137761048, -9.862500000000036238 ) ) ;
#30744 = EDGE_LOOP ( 'NONE', ( #16539, #3191, #13554, #27392 ) ) ;
#30745 = FACE_OUTER_BOUND ( 'NONE', #31343, .T. ) ;
#30746 = CARTESIAN_POINT ( 'NONE',  ( 8.710071997420127943, 82.28518628210146346, 3.796722387233375073 ) ) ;
#30747 = CARTESIAN_POINT ( 'NONE',  ( 6.840914352311949109, 122.6398137178985479, 6.594114490232462877 ) ) ;
#30748 = CARTESIAN_POINT ( 'NONE',  ( -13.62178482187498396, 195.8281250006145342, 23.59362340125808188 ) ) ;
#30749 = CARTESIAN_POINT ( 'NONE',  ( 15.00000000000021316, -3.464101615137879620, -5.812500000000008882 ) ) ;
#30750 = CARTESIAN_POINT ( 'NONE',  ( 13.62178482187499640, 197.4593750006145285, -23.59362340125807123 ) ) ;
#30751 = CARTESIAN_POINT ( 'NONE',  ( 15.00000000000045297, -3.464101615138017287, -1.706249998770939191 ) ) ;
#30752 = DIRECTION ( 'NONE',  ( 0.000000000000000000, 1.000000000000000000, 0.000000000000000000 ) ) ;
#30753 = CARTESIAN_POINT ( 'NONE',  ( 8.152565276336593669, 57.95231371789854791, 5.233372021372610483 ) ) ;
#30754 = CARTESIAN_POINT ( 'NONE',  ( 18.00000000000000000, 5.196152422706630247, -9.975000000000012079 ) ) ;
#30755 = ORIENTED_EDGE ( 'NONE', *, *, #2683, .F. ) ;
#30756 = CARTESIAN_POINT ( 'NONE',  ( 21.00000000000000000, 241.8437500012290400, -6.928203230275506996 ) ) ;
#30757 = VECTOR ( 'NONE', #36130, 999.9999999999998863 ) ;
#30758 = CARTESIAN_POINT ( 'NONE',  ( 8.715434833792128799, 65.13981371789854791, -8.962234695871567070 ) ) ;
#30759 = CARTESIAN_POINT ( 'NONE',  ( 13.44051670066910731, 5.407089921784862696, -7.471874999385508254 ) ) ;
#30760 = CARTESIAN_POINT ( 'NONE',  ( -27.24356964375000345, 198.4531250006145342, 0.000000000000000000 ) ) ;
#30761 = CARTESIAN_POINT ( 'NONE',  ( 15.24356964374999990, 0.000000000000000000, -7.003124999385490490 ) ) ;
#30762 = CARTESIAN_POINT ( 'NONE',  ( -12.46528703574811558, 33.80231371789854933, 2.660918448318003726 ) ) ;
#30763 = VERTEX_POINT ( 'NONE', #5299 ) ;
#30764 = CARTESIAN_POINT ( 'NONE',  ( 10.31873187879410914, 0.000000000000000000, -0.1968749993855323233 ) ) ;
#30765 = CARTESIAN_POINT ( 'NONE',  ( -4.622313124798576922, 5.235186282101428112, -11.61527771782819762 ) ) ;
#30766 = CARTESIAN_POINT ( 'NONE',  ( 22.56230152254410726, 7.347880794884117764E-16, -9.562499998771039955 ) ) ;
#30767 = CARTESIAN_POINT ( 'NONE',  ( -59.89211230271182984, 203.5309553116391612, 1.857196546604092280 ) ) ;
#30768 = FACE_OUTER_BOUND ( 'NONE', #24738, .T. ) ;
#30769 = CARTESIAN_POINT ( 'NONE',  ( 8.962234695871567070, 67.43981371789855928, 8.715434833792127023 ) ) ;
#30770 = EDGE_CURVE ( 'NONE', #32942, #20931, #12952, .T. ) ;
#30771 = CARTESIAN_POINT ( 'NONE',  ( -67.21502896937850835, 213.8393509191290889, -2.350049139982142155 ) ) ;
#30772 = CARTESIAN_POINT ( 'NONE',  ( -54.75372103062154849, 216.5309553116391612, -1.626142955000564383 ) ) ;
#30773 = FACE_OUTER_BOUND ( 'NONE', #23513, .T. ) ;
#30774 = CARTESIAN_POINT ( 'NONE',  ( -14.25334919248795096, 42.71481371789855075, 6.092822981423662299 ) ) ;
#30775 = CARTESIAN_POINT ( 'NONE',  ( -35.54836230271182984, 202.5810206699313767, -4.149950860017804111 ) ) ;
#30776 = CARTESIAN_POINT ( 'NONE',  ( -10.69584247140444866, 30.24768628210144783, 6.932735513423972762 ) ) ;
#30777 = CARTESIAN_POINT ( 'NONE',  ( 26.99999999999999289, 0.000000000000000000, -8.000000000000000000 ) ) ;
#30778 = CARTESIAN_POINT ( 'NONE',  ( -7.228626920339069173, 66.47268628210144925, 10.49813415415989581 ) ) ;
#30779 = CARTESIAN_POINT ( 'NONE',  ( 15.46528703574804986, 8.397686282101439303, 3.257655550457285720 ) ) ;
#30780 = CARTESIAN_POINT ( 'NONE',  ( 22.56230152254411436, 3.464101615137759271, -2.437500000000027534 ) ) ;
#30781 = CARTESIAN_POINT ( 'NONE',  ( -28.98576012241837319, 202.0511556252696721, -1.045925494027194702 ) ) ;
#30782 = EDGE_LOOP ( 'NONE', ( #11427, #11885, #36804, #24136 ) ) ;
#30783 = CARTESIAN_POINT ( 'NONE',  ( 11.08355503943142750, 34.56018628210144783, -10.83675517735155225 ) ) ;
#30784 = CARTESIAN_POINT ( 'NONE',  ( -27.24356964375000345, 195.7156250006145513, -15.72908226750537786 ) ) ;
#30785 = CARTESIAN_POINT ( 'NONE',  ( 27.24356964375000345, 198.2843750006145456, -3.336375036156643733E-15 ) ) ;
#30786 = CARTESIAN_POINT ( 'NONE',  ( 2.999999999999997335, 244.5000000000000000, 1.000000000000000000 ) ) ;
#30787 = CARTESIAN_POINT ( 'NONE',  ( 13.49999999999999645, 195.4625000012290172, -23.38268590217984766 ) ) ;
#30788 = CARTESIAN_POINT ( 'NONE',  ( -7.234628195640354420, 195.1424038105676573, 26.99999999999996803 ) ) ;
#30789 = CARTESIAN_POINT ( 'NONE',  ( 12.53471296425194836, 7.822686282101448896, -2.311890736173178418 ) ) ;
#30790 = CARTESIAN_POINT ( 'NONE',  ( 21.00000000000000000, 248.8468750006145456, -6.646953231504538984 ) ) ;
#30791 = CARTESIAN_POINT ( 'NONE',  ( -7.954856959092309943, 106.8273137178985479, 5.529263428287300108 ) ) ;
#30792 = CARTESIAN_POINT ( 'NONE',  ( 15.24356964375000167, 244.0468750006145342, 3.323476615752272600 ) ) ;
#30793 = ORIENTED_EDGE ( 'NONE', *, *, #20591, .F. ) ;
#30794 = CARTESIAN_POINT ( 'NONE',  ( 21.00000000000000000, 249.0437500012290570, -6.928203230275506996 ) ) ;
#30795 = CARTESIAN_POINT ( 'NONE',  ( -10.69584247140429412, 108.5523137178985564, -6.932735513424201024 ) ) ;
#30796 = CARTESIAN_POINT ( 'NONE',  ( 16.56230152254411436, -7.209453229046475009, -9.928124999385525840 ) ) ;
#30797 = CARTESIAN_POINT ( 'NONE',  ( 24.55988044515800439, 0.000000000000000000, 162.3265474014984591 ) ) ;
#30798 = FACE_OUTER_BOUND ( 'NONE', #22177, .T. ) ;
#30799 = CARTESIAN_POINT ( 'NONE',  ( 26.99999999999999645, 197.1125000000000398, -15.58845726811990495 ) ) ;
#30800 = EDGE_LOOP ( 'NONE', ( #3707, #12576, #6342, #4736, #36094, #20785, #1788, #30156 ) ) ;
#30801 = CARTESIAN_POINT ( 'NONE',  ( 0.1745138560725515708, 33.41018628210144925, -12.50000000000000355 ) ) ;
#30802 = VERTEX_POINT ( 'NONE', #10596 ) ;
#30803 = AXIS2_PLACEMENT_3D ( 'NONE', #20064, #17032, #10960 ) ;
#30804 = VERTEX_POINT ( 'NONE', #22359 ) ;
#30805 = CARTESIAN_POINT ( 'NONE',  ( 21.00000000000000000, 6.928203230275506996, -3.656249998770947585 ) ) ;
#30806 = CARTESIAN_POINT ( 'NONE',  ( 23.87821517812499650, 4.985214923628404904, -0.7406249993854585600 ) ) ;
#30807 = CARTESIAN_POINT ( 'NONE',  ( 26.99999999999999645, 249.3437500012290400, 3.464101615137751278 ) ) ;
#30808 = CARTESIAN_POINT ( 'NONE',  ( 23.99999999999999645, 5.196152422706631135, -4.649999999999987921 ) ) ;
#30809 = CARTESIAN_POINT ( 'NONE',  ( 26.75643035624999655, 249.0343750006145456, 3.323476615752267715 ) ) ;
#30810 = CARTESIAN_POINT ( 'NONE',  ( -12.50000000000000355, 67.91018628210144925, -0.1745138560725492671 ) ) ;
#30811 = CARTESIAN_POINT ( 'NONE',  ( 5.770363421894130873, 9.364813717898543999, -14.38691631536193860 ) ) ;
#30812 = EDGE_CURVE ( 'NONE', #25531, #23197, #34092, .T. ) ;
#30813 = CARTESIAN_POINT ( 'NONE',  ( -58.90252896937850124, 206.6499508600178387, -5.571401726697954970 ) ) ;
#30814 = CARTESIAN_POINT ( 'NONE',  ( 5.128366027876307243, 215.9518627395465558, -0.7835069059934931524 ) ) ;
#30815 = CARTESIAN_POINT ( 'NONE',  ( -53.16294563604516554, 213.2096571498974527, -3.378800118222469617 ) ) ;
#30816 = CARTESIAN_POINT ( 'NONE',  ( 34.01258395714663152, 5.196152422706631135, 164.3133754872583836 ) ) ;
#30817 = CARTESIAN_POINT ( 'NONE',  ( -12.46528703574811558, 125.8023137178985706, 2.660918448318003726 ) ) ;
#30818 = CARTESIAN_POINT ( 'NONE',  ( -68.01413769728823411, 212.1499508600178387, 3.954877714930865817 ) ) ;
#30820 = ADVANCED_FACE ( 'NONE', ( #36924 ), #31618, .F. ) ;
#30819 = CARTESIAN_POINT ( 'NONE',  ( -63.46205436395489841, 216.1378603801730094, 6.307003348497944195 ) ) ;
#30821 = CONTEXT_DEPENDENT_SHAPE_REPRESENTATION ( #7179, #5302 ) ;
#30822 = CARTESIAN_POINT ( 'NONE',  ( 15.24356964374999990, 3.323476615752268604, -1.640624999385488891 ) ) ;
#30823 = CARTESIAN_POINT ( 'NONE',  ( -27.24356964374999990, 196.6156250006145285, -15.72908226750537786 ) ) ;
#30824 = CARTESIAN_POINT ( 'NONE',  ( -8.632099005475794229, 97.05231371789855643, 13.23911966647199812 ) ) ;
#30825 = CARTESIAN_POINT ( 'NONE',  ( -46.82961230271183695, 211.8571965466040297, 6.469044688360755302 ) ) ;
#30826 = ORIENTED_EDGE ( 'NONE', *, *, #23118, .T. ) ;
#30827 = CARTESIAN_POINT ( 'NONE',  ( 25.25600545691528254, 0.000000000000000000, 167.4886444474074381 ) ) ;
#30828 = CARTESIAN_POINT ( 'NONE',  ( -11.48171059495397373, 123.6851862821014549, -4.944772684328680334 ) ) ;
#30829 = CARTESIAN_POINT ( 'NONE',  ( -14.25334919248782306, 59.28518628210144925, -6.092822981423979378 ) ) ;
#30830 = PLANE ( 'NONE',  #4745 ) ;
#30831 = CARTESIAN_POINT ( 'NONE',  ( 24.79356678040014117, -3.604726614523244610, 164.9975944357569517 ) ) ;
#30832 = CARTESIAN_POINT ( 'NONE',  ( -3.257655550457281723, 93.49768628210142651, 15.46528703574804986 ) ) ;
#30833 = CARTESIAN_POINT ( 'NONE',  ( -54.55580436395489841, 216.5000000000000000, 0.1155267958017343610 ) ) ;
#30834 = CARTESIAN_POINT ( 'NONE',  ( 19.68408634441910365, -5.407089921784855591, -5.840624999385535254 ) ) ;
#30835 = CARTESIAN_POINT ( 'NONE',  ( -9.534712964251941258, 30.82268628210143291, 1.715153634034234154 ) ) ;
#30836 = CARTESIAN_POINT ( 'NONE',  ( 27.00000000000023448, 3.464101615137617163, -2.831249998770953180 ) ) ;
#30837 = CARTESIAN_POINT ( 'NONE',  ( -58.90997103062156270, 215.5714017266979852, 3.350049139982118618 ) ) ;
#30838 = CARTESIAN_POINT ( 'NONE',  ( 20.99999999999999289, 243.1937500012290343, -5.999999999999997335 ) ) ;
#30839 = CARTESIAN_POINT ( 'NONE',  ( 7.228626920339068285, 52.67268628210144499, -10.49813415415989581 ) ) ;
#30840 = CARTESIAN_POINT ( 'NONE',  ( -13.49999999999998401, 197.8249999999999886, 23.38268590217985476 ) ) ;
#30841 = CARTESIAN_POINT ( 'NONE',  ( 5.438367727407757144E-14, 197.7500000012290400, -27.00000000000000000 ) ) ;
#30843 = CARTESIAN_POINT ( 'NONE',  ( 13.44051670066911264, -5.407089921784865361, -1.471874999385502925 ) ) ;
#30842 = CARTESIAN_POINT ( 'NONE',  ( 3.796722387233379514, 33.98518628210143788, -8.710071997420127943 ) ) ;
#30844 = CARTESIAN_POINT ( 'NONE',  ( 26.99999999999999645, 198.5750000012290570, -15.58845726811990495 ) ) ;
#30845 = ORIENTED_EDGE ( 'NONE', *, *, #19625, .F. ) ;
#30846 = CARTESIAN_POINT ( 'NONE',  ( 21.00000000000000000, -6.928203230275506996, -1.687500000000023981 ) ) ;
#30847 = CARTESIAN_POINT ( 'NONE',  ( 22.38931379102810837, -5.788467285583099198, -8.000000000000003553 ) ) ;
#30848 = CARTESIAN_POINT ( 'NONE',  ( 24.63668644345436931, -3.604726614523244610, 163.2044439791918080 ) ) ;
#30849 = CARTESIAN_POINT ( 'NONE',  ( 24.77555942491173369, 0.000000000000000000, 161.9971211729523475 ) ) ;
#30850 = CARTESIAN_POINT ( 'NONE',  ( 18.00000000000000355, 242.8750000000000000, 5.196152422706632912 ) ) ;
#30851 = CARTESIAN_POINT ( 'NONE',  ( -100.7560012262353411, 61.79101779669657191, 5.000000000000000000 ) ) ;
#30852 = CARTESIAN_POINT ( 'NONE',  ( -10.49813415416004858, 88.42731371789858485, 7.228626920338839135 ) ) ;
#30853 = CARTESIAN_POINT ( 'NONE',  ( 2.311890736173175753, 83.72268628210144925, 12.53471296425194659 ) ) ;
#30854 = ORIENTED_EDGE ( 'NONE', *, *, #3349, .T. ) ;
#30855 = ORIENTED_EDGE ( 'NONE', *, *, #21878, .F. ) ;
#30856 = CARTESIAN_POINT ( 'NONE',  ( 26.99999999999999645, 198.5750000012290286, -15.58845726811990495 ) ) ;
#30857 = CARTESIAN_POINT ( 'NONE',  ( 15.00000000000000000, 0.000000000000000000, -4.049999999999998046 ) ) ;
#30858 = CARTESIAN_POINT ( 'NONE',  ( 14.25334919248795451, 56.51481371789856212, -6.092822981423661410 ) ) ;
#30859 = CARTESIAN_POINT ( 'NONE',  ( 15.24356964374999990, 3.323476615752268604, -9.740624999385508076 ) ) ;
#30860 = CARTESIAN_POINT ( 'NONE',  ( 18.12178482187500350, 242.7343750006145342, 4.985214923628407568 ) ) ;
#30861 = CARTESIAN_POINT ( 'NONE',  ( -56.53497103062156270, 206.1606490808709111, -2.350049139982163027 ) ) ;
#30862 = CARTESIAN_POINT ( 'NONE',  ( 1.069080835302379631E-14, 199.6625000000000227, 27.00000000000000000 ) ) ;
#30863 = CARTESIAN_POINT ( 'NONE',  ( 7.954856959092311719, 37.82731371789854080, -5.529263428287300108 ) ) ;
#30864 = CARTESIAN_POINT ( 'NONE',  ( 16.56230152254411436, 7.209453229046475009, -7.003124999385537564 ) ) ;
#30865 =( BOUNDED_CURVE ( )  B_SPLINE_CURVE ( 2, ( #28070, #13865, #1731, #10825, #8178, #16336, #27884, #22026, #13683 ),
 .UNSPECIFIED., .F., .F. ) 
 B_SPLINE_CURVE_WITH_KNOTS ( ( 3, 2, 2, 2, 3 ),
 ( 0.3541666666666666852, 0.3611111111111111049, 0.3750000000000000000, 0.3888888888888888951, 0.3958333333333333703 ),
 .UNSPECIFIED. ) 
 CURVE ( )  GEOMETRIC_REPRESENTATION_ITEM ( )  RATIONAL_B_SPLINE_CURVE ( ( 0.9330127018922194093, 0.9330127018922196314, 1.000000000000000000, 0.8660254037844387076, 1.000000000000000000, 0.8660254037844387076, 1.000000000000000000, 0.9330127018922190762, 0.9330127018922194093 ) ) 
 REPRESENTATION_ITEM ( '' )  );
#30866 = VECTOR ( 'NONE', #35472, 1000.000000000000000 ) ;
#30867 = CARTESIAN_POINT ( 'NONE',  ( -8.843639120294245259, 99.06481371789857349, -3.474262827703533230 ) ) ;
#30868 = CARTESIAN_POINT ( 'NONE',  ( 13.62178482187501416, 197.3093750006145513, 23.59362340125806767 ) ) ;
#30869 = CARTESIAN_POINT ( 'NONE',  ( 8.715434833792128799, 19.13981371789855146, -8.962234695871567070 ) ) ;
#30870 = CARTESIAN_POINT ( 'NONE',  ( 12.46528703574805874, 72.79768628210146630, 2.660918448318279950 ) ) ;
#30871 = CARTESIAN_POINT ( 'NONE',  ( 13.56230152254410370, 5.196152422706630247, -9.412499998771028942 ) ) ;
#30872 = CARTESIAN_POINT ( 'NONE',  ( -12.50000000000000355, 143.0000000000000284, -1.353084311261909534E-13 ) ) ;
#30873 = CARTESIAN_POINT ( 'NONE',  ( 30.71105627401454896, -7.209453229046475009, 160.9978811270534891 ) ) ;
#30874 = CARTESIAN_POINT ( 'NONE',  ( 24.00000000000000000, -5.196152422706629359, -1.143749998770954290 ) ) ;
#30875 = CARTESIAN_POINT ( 'NONE',  ( 22.80587116629411781, 7.646167579472024665E-16, -5.821874999385522997 ) ) ;
#30876 = AXIS2_PLACEMENT_3D ( 'NONE', #32628, #18240, #15392 ) ;
#30877 = CARTESIAN_POINT ( 'NONE',  ( 3.474262827703335166, 101.8351862821014606, 8.843639120294326972 ) ) ;
#30878 = DIRECTION ( 'NONE',  ( -1.000000000000000000, 0.000000000000000000, 0.000000000000000000 ) ) ;
#30879 =( BOUNDED_SURFACE ( )  B_SPLINE_SURFACE ( 3, 2, ( 
 ( #33283, #7507, #24564 ),
 ( #6753, #21174, #36117 ),
 ( #18327, #24382, #13194 ),
 ( #35927, #24747, #15477 ),
 ( #12629, #24194, #21915 ),
 ( #7321, #19081, #30252 ),
 ( #4096, #30633, #27593 ),
 ( #869, #12441, #35739 ),
 ( #32901, #9785, #18895 ),
 ( #16045, #21362, #6954 ),
 ( #18522, #15667, #1623 ),
 ( #27218, #18713, #15855 ),
 ( #30445, #36676, #16969 ),
 ( #13377, #34022, #19455 ),
 ( #10900, #19273, #34393 ),
 ( #22288, #22473, #8066 ),
 ( #22846, #31364, #14122 ),
 ( #28511, #4837, #5208 ),
 ( #25119, #33842, #28146 ),
 ( #20003, #13758, #16230 ),
 ( #19643, #31185, #16785 ),
 ( #37229, #37041, #7880 ),
 ( #2554, #16603, #25304 ),
 ( #27962, #13566, #27781 ),
 ( #7692, #11277, #11089 ),
 ( #30814, #24931, #33653 ),
 ( #2367, #31003, #16415 ),
 ( #25678, #5389, #36856 ),
 ( #36484, #10714, #1993 ),
 ( #28329, #22665, #34209 ),
 ( #13940, #5023, #2177 ),
 ( #25489, #8253, #19827 ),
 ( #8434, #4649, #1808 ),
 ( #10528, #22104, #29447 ),
 ( #31919, #5762, #6134 ),
 ( #14489, #31548, #15051 ),
 ( #8616, #12198, #29062 ),
 ( #6331, #31735, #2735 ),
 ( #8804, #14308, #261 ),
 ( #23772, #20185, #11638 ),
 ( #11825, #26046, #35311 ),
 ( #23396, #3293, #73 ),
 ( #26224, #17342, #23213 ),
 ( #17528, #34762, #9366 ),
 ( #5572, #446, #34944 ),
 ( #17157, #23027, #26600 ) ),
 .UNSPECIFIED., .F., .F., .F. ) 
 B_SPLINE_SURFACE_WITH_KNOTS ( ( 4, 2, 2, 2, 2, 2, 2, 2, 2, 2, 2, 2, 2, 2, 2, 2, 2, 2, 2, 2, 2, 2, 4 ),
 ( 3, 3 ),
 ( 4.712388980384689674, 4.908738521234051966, 5.105088062083414258, 5.301437602932775661, 5.497787143782137953, 5.694136684631500245, 5.792311455056180947, 5.890486225480861648, 5.988660995905542350, 6.086835766330223940, 6.185010536754905530, 6.283185307179586232, 6.381360077604266934, 6.479534848028948524, 6.577709618453630114, 6.675884388878310816, 6.774059159302991517, 6.872233929727672219, 7.068583470577034511, 7.264933011426396803, 7.461282552275758206, 7.657632093125120498, 7.853981633974482790 ),
 ( 0.000000000000000000, 1.000000000000000000 ),
 .UNSPECIFIED. ) 
 GEOMETRIC_REPRESENTATION_ITEM ( )  RATIONAL_B_SPLINE_SURFACE ( (
 ( 1.000000000000000000, 1.000000000000000000, 1.000000000000000000),
 ( 1.000000000000000000, 1.000009746410878364, 1.000000000000000000),
 ( 1.000000000000000000, 0.9967613244605102452, 1.000000000000000000),
 ( 1.000000000000000000, 0.9841171504872305853, 1.000000000000000000),
 ( 1.000000000000000000, 0.9747108043634977737, 1.000000000000000000),
 ( 1.000000000000000000, 0.9506740353988157866, 1.000000000000000000),
 ( 1.000000000000000000, 0.9360421842704774731, 1.000000000000000000),
 ( 1.000000000000000000, 0.9031650994159179380, 1.000000000000000000),
 ( 1.000000000000000000, 0.8849191471317067181, 1.000000000000000000),
 ( 1.000000000000000000, 0.8471316604371722514, 1.000000000000000000),
 ( 1.000000000000000000, 0.8275942695927370751, 1.000000000000000000),
 ( 1.000000000000000000, 0.7995620738861383137, 1.000000000000000000),
 ( 1.000000000000000000, 0.7904353558348173880, 1.000000000000000000),
 ( 1.000000000000000000, 0.7730318702305081224, 1.000000000000000000),
 ( 1.000000000000000000, 0.7647559708311986171, 1.000000000000000000),
 ( 1.000000000000000000, 0.7494742688660065433, 1.000000000000000000),
 ( 1.000000000000000000, 0.7424696633570816440, 1.000000000000000000),
 ( 1.000000000000000000, 0.7301234195064296717, 1.000000000000000000),
 ( 1.000000000000000000, 0.7247831711438370572, 1.000000000000000000),
 ( 1.000000000000000000, 0.7160917253994798504, 1.000000000000000000),
 ( 1.000000000000000000, 0.7127418075764269112, 1.000000000000000000),
 ( 1.000000000000000000, 0.7082489452424536314, 1.000000000000000000),
 ( 1.000000000000000000, 0.7071067811865475727, 1.000000000000000000),
 ( 1.000000000000000000, 0.7071067811865475727, 1.000000000000000000),
 ( 1.000000000000000000, 0.7082489452424827192, 1.000000000000000000),
 ( 1.000000000000000000, 0.7127418075763976013, 1.000000000000000000),
 ( 1.000000000000000000, 0.7160917253994796283, 1.000000000000000000),
 ( 1.000000000000000000, 0.7247831711438368352, 1.000000000000000000),
 ( 1.000000000000000000, 0.7301234195064293386, 1.000000000000000000),
 ( 1.000000000000000000, 0.7424696633570813109, 1.000000000000000000),
 ( 1.000000000000000000, 0.7494742688657879404, 1.000000000000000000),
 ( 1.000000000000000000, 0.7647559708314156657, 1.000000000000000000),
 ( 1.000000000000000000, 0.7730318702303776712, 1.000000000000000000),
 ( 1.000000000000000000, 0.7904353558349440645, 1.000000000000000000),
 ( 1.000000000000000000, 0.7995620738860717003, 1.000000000000000000),
 ( 1.000000000000000000, 0.8275942695928699688, 1.000000000000000000),
 ( 1.000000000000000000, 0.8471316604371704750, 1.000000000000000000),
 ( 1.000000000000000000, 0.8849191471317049418, 1.000000000000000000),
 ( 1.000000000000000000, 0.9031650994159176049, 1.000000000000000000),
 ( 1.000000000000000000, 0.9360421842704771400, 1.000000000000000000),
 ( 1.000000000000000000, 0.9506740353988152314, 1.000000000000000000),
 ( 1.000000000000000000, 0.9747108043634972185, 1.000000000000000000),
 ( 1.000000000000000000, 0.9841171504871490949, 1.000000000000000000),
 ( 1.000000000000000000, 0.9967613244605915135, 1.000000000000000000),
 ( 1.000000000000000000, 1.000009746410817302, 1.000000000000000000),
 ( 1.000000000000000000, 1.000000000000000000, 1.000000000000000000) ) ) 
 REPRESENTATION_ITEM ( '' )  SURFACE ( )  );
#30880 = CARTESIAN_POINT ( 'NONE',  ( -8.962234695871760692, 112.7601862821014720, 8.715434833791933400 ) ) ;
#30881 = CARTESIAN_POINT ( 'NONE',  ( 22.56230152254411792, 7.347880794884125653E-16, -4.725000000000035172 ) ) ;
#30882 = FACE_OUTER_BOUND ( 'NONE', #1665, .T. ) ;
#30883 = ORIENTED_EDGE ( 'NONE', *, *, #29518, .F. ) ;
#30884 = CARTESIAN_POINT ( 'NONE',  ( 34.22950430627932406, 5.407089921784857367, 165.3954622995096599 ) ) ;
#30885 = CARTESIAN_POINT ( 'NONE',  ( 15.24356964375000167, -3.323476615752272600, -5.953124999385460470 ) ) ;
#30886 = CARTESIAN_POINT ( 'NONE',  ( 27.24356964375000345, 197.8343750006145569, -3.336375036156643733E-15 ) ) ;
#30887 = CARTESIAN_POINT ( 'NONE',  ( 25.21845102629494306, 3.604726614523240613, 169.8540435889542266 ) ) ;
#30888 = CARTESIAN_POINT ( 'NONE',  ( 37.30185536379416078, 3.464101615137759271, 167.4887799662076020 ) ) ;
#30889 = CARTESIAN_POINT ( 'NONE',  ( 18.00000000000000355, 239.7812500012290400, 5.196152422706632912 ) ) ;
#30890 = CARTESIAN_POINT ( 'NONE',  ( 26.75643035624999655, 240.6343750006145115, -7.049594010296217766E-16 ) ) ;
#30891 = DIRECTION ( 'NONE',  ( 0.8083506638593009885, 0.5887012860850802110, 0.000000000000000000 ) ) ;
#30892 = ADVANCED_FACE ( 'NONE', ( #7949 ), #4904, .F. ) ;
#30893 = CARTESIAN_POINT ( 'NONE',  ( 0.1745138560722779009, 142.1898137178985735, 12.50000000000000355 ) ) ;
#30894 = CARTESIAN_POINT ( 'NONE',  ( -13.62178482187498396, 194.9843750006145626, 23.59362340125808188 ) ) ;
#30895 = CIRCLE ( 'NONE', #19384, 4.000000000000003553 ) ;
#30897 = ORIENTED_EDGE ( 'NONE', *, *, #17818, .T. ) ;
#30896 = ORIENTED_EDGE ( 'NONE', *, *, #2236, .F. ) ;
#30898 = CARTESIAN_POINT ( 'NONE',  ( 26.75643035624999655, 244.6093750006145342, -3.323476615752271712 ) ) ;
#30899 = CARTESIAN_POINT ( 'NONE',  ( -12.53471296425189152, 15.97731371789853938, -2.311890736173453309 ) ) ;
#30900 = CARTESIAN_POINT ( 'NONE',  ( 18.12178482187500350, -4.985214923628407568, -4.115624999385475213 ) ) ;
#30901 = CARTESIAN_POINT ( 'NONE',  ( -14.25334919248795096, 116.3148137178985735, 6.092822981423662299 ) ) ;
#30902 = CARTESIAN_POINT ( 'NONE',  ( 19.56230152254411792, 5.196152422706637353, -2.400000000000013234 ) ) ;
#30903 = CARTESIAN_POINT ( 'NONE',  ( 18.12178482187500350, -4.985214923628407568, -1.528124999385482852 ) ) ;
#30904 = CARTESIAN_POINT ( 'NONE',  ( 22.80587116629412492, -3.604726614523238837, -9.009374999385519445 ) ) ;
#30905 = ORIENTED_EDGE ( 'NONE', *, *, #22347, .F. ) ;
#30906 = CARTESIAN_POINT ( 'NONE',  ( 27.00000000000000355, 198.5375000012290627, -3.306546357697854128E-15 ) ) ;
#30907 = AXIS2_PLACEMENT_3D ( 'NONE', #22168, #16853, #31063 ) ;
#30908 = CARTESIAN_POINT ( 'NONE',  ( -6.932735513423968321, 115.3476862821014635, -10.69584247140445221 ) ) ;
#30909 = CARTESIAN_POINT ( 'NONE',  ( 16.56230152254411436, 7.209453229046475009, -0.2531249993855048674 ) ) ;
#30910 = EDGE_CURVE ( 'NONE', #18816, #11333, #33321, .T. ) ;
#30911 = CARTESIAN_POINT ( 'NONE',  ( -45.44419563604516554, 201.5000000000000000, 0.1155267958018195706 ) ) ;
#30912 = CARTESIAN_POINT ( 'NONE',  ( 15.24356964375000167, 245.2843750006145171, 3.323476615752272600 ) ) ;
#30913 = CARTESIAN_POINT ( 'NONE',  ( 19.56230152254411792, -5.196152422706629359, -2.887499998771053455 ) ) ;
#30914 = CARTESIAN_POINT ( 'NONE',  ( -32.57961230271184405, 211.3212981617417938, 4.469044688360757966 ) ) ;
#30915 = CARTESIAN_POINT ( 'NONE',  ( 11.61527771782819940, 117.9351862821014549, -4.622313124798573369 ) ) ;
#30916 = CARTESIAN_POINT ( 'NONE',  ( 19.56230152254410726, 5.196152422706631135, -0.4874999987710126881 ) ) ;
#30918 = ORIENTED_EDGE ( 'NONE', *, *, #28459, .F. ) ;
#30917 = EDGE_CURVE ( 'NONE', #23609, #4638, #33759, .T. ) ;
#30919 = CARTESIAN_POINT ( 'NONE',  ( -49.80580436395490551, 216.5000000000000000, 0.1155267958017343610 ) ) ;
#30920 = LINE ( 'NONE', #4937, #30043 ) ;
#30921=STYLED_ITEM('',(#37556),#20231);
#30922 = CARTESIAN_POINT ( 'NONE',  ( 13.56230152254411792, -5.196152422706638241, -8.925000000000071765 ) ) ;
#30923 = CARTESIAN_POINT ( 'NONE',  ( -15.53471296425195369, 122.8226862821014294, 2.908627838312118019 ) ) ;
#30924 = CARTESIAN_POINT ( 'NONE',  ( 26.99999999999999645, 199.3625000000000114, -15.58845726811990495 ) ) ;
#30925 = CARTESIAN_POINT ( 'NONE',  ( -12.53471296425194836, 12.42268628210144321, 2.311890736173176641 ) ) ;
#30926 = CARTESIAN_POINT ( 'NONE',  ( 16.56230152254411436, 6.928203230275514990, -8.212500000000009237 ) ) ;
#30927 = ORIENTED_EDGE ( 'NONE', *, *, #198, .T. ) ;
#30928 = CARTESIAN_POINT ( 'NONE',  ( -29.00000000000002487, 210.0000000000000000, 0.000000000000000000 ) ) ;
#30929 = CARTESIAN_POINT ( 'NONE',  ( 8.843639120294328748, 81.13518628210145778, -3.474262827703334722 ) ) ;
#30930 = CARTESIAN_POINT ( 'NONE',  ( 15.00000000000000000, 0.000000000000000000, -2.700000000000008171 ) ) ;
#30931 = CARTESIAN_POINT ( 'NONE',  ( -6.840914352311947333, 127.2398137178985422, -6.594114490232462877 ) ) ;
#30932 = CARTESIAN_POINT ( 'NONE',  ( -13.62178482187500528, 196.1281250006145171, -23.59362340125807123 ) ) ;
#30933 = CARTESIAN_POINT ( 'NONE',  ( 26.99999999999999645, 7.347880794884117764E-16, -5.624999999999991118 ) ) ;
#30934 = CARTESIAN_POINT ( 'NONE',  ( -27.24356964374999635, 198.9968750006145228, 15.72908226750539384 ) ) ;
#30935 = DIRECTION ( 'NONE',  ( 0.000000000000000000, 0.000000000000000000, 1.000000000000000000 ) ) ;
#30936 = CYLINDRICAL_SURFACE ( 'NONE', #28454, 6.000000000000001776 ) ;
#30937 = CARTESIAN_POINT ( 'NONE',  ( 8.710071997420211432, 65.71481371789855075, -3.796722387233181895 ) ) ;
#30938 = CARTESIAN_POINT ( 'NONE',  ( 22.56230152254410370, 7.347880794884117764E-16, -2.362499998771028231 ) ) ;
#30939 = VERTEX_POINT ( 'NONE', #7763 ) ;
#30940 = CARTESIAN_POINT ( 'NONE',  ( 18.00000000000000000, 241.8812500012290343, -5.196152422706630247 ) ) ;
#30941 = CARTESIAN_POINT ( 'NONE',  ( 12.50000000000000355, 57.08981371789855075, -0.1745138560722771515 ) ) ;
#30942 = EDGE_CURVE ( 'NONE', #28321, #190, #25375, .T. ) ;
#30943 = CARTESIAN_POINT ( 'NONE',  ( 22.80587116629411781, 3.604726614523243278, -5.334374999385495641 ) ) ;
#30944 = CARTESIAN_POINT ( 'NONE',  ( -13.62178482187500528, 197.4781250006145399, -23.59362340125807123 ) ) ;
#30945 = CARTESIAN_POINT ( 'NONE',  ( 15.24356964375000167, -3.323476615752272600, -7.415624999385471483 ) ) ;
#30946 = CARTESIAN_POINT ( 'NONE',  ( 8.962234695871567070, 30.63981371789854791, 8.715434833792127023 ) ) ;
#30947 = VECTOR ( 'NONE', #9029, 1000.000000000000000 ) ;
#30948 = EDGE_LOOP ( 'NONE', ( #31672, #34220, #8294, #26542 ) ) ;
#30949 = UNCERTAINTY_MEASURE_WITH_UNIT (LENGTH_MEASURE( 1.000000000000000082E-05 ), #7623, 'distance_accuracy_value', 'NONE');
#30950 = CARTESIAN_POINT ( 'NONE',  ( 10.31873187879410736, -3.604726614523244610, -1.959374999385511185 ) ) ;
#30951 = CARTESIAN_POINT ( 'NONE',  ( -9.000000000000024869, 210.0000000000000000, 0.000000000000000000 ) ) ;
#30952 = EDGE_CURVE ( 'NONE', #26216, #33455, #28428, .T. ) ;
#30953 = CARTESIAN_POINT ( 'NONE',  ( 28.28586808984062628, 5.407089921784862696, 169.0963171987856128 ) ) ;
#30954 = CARTESIAN_POINT ( 'NONE',  ( -47.42336230271183695, 215.6869285224997270, 3.149950860017831200 ) ) ;
#30955 = EDGE_CURVE ( 'NONE', #23622, #22557, #25560, .T. ) ;
#30956 = CARTESIAN_POINT ( 'NONE',  ( -27.00000000000000355, 196.3625000000000114, -15.58845726811989429 ) ) ;
#30957 = CARTESIAN_POINT ( 'NONE',  ( 12.53471296425189330, 66.57731371789856212, 2.311890736173451977 ) ) ;
#30958 = CARTESIAN_POINT ( 'NONE',  ( -65.23586230271183695, 207.8500491399821613, 3.954877714930852495 ) ) ;
#30959 = CARTESIAN_POINT ( 'NONE',  ( -52.57663769728823411, 204.3130714775002730, 3.149950860017883603 ) ) ;
#30960 = CARTESIAN_POINT ( 'NONE',  ( 7.234628195640309123, 195.9299038117966916, -27.00000000000000711 ) ) ;
#30961 = CARTESIAN_POINT ( 'NONE',  ( 24.82785287066792179, -3.464101615138032830, 162.5948379930317174 ) ) ;
#30962 = CARTESIAN_POINT ( 'NONE',  ( 10.83675517735179206, 37.53981371789855359, -11.08355503943118769 ) ) ;
#30963 = CARTESIAN_POINT ( 'NONE',  ( -69.00372103062157692, 218.5309553116391896, -2.162041339862839084 ) ) ;
#30964 = CARTESIAN_POINT ( 'NONE',  ( -11.48171059495397373, 22.48518628210144499, -4.944772684328680334 ) ) ;
#30965 = AXIS2_PLACEMENT_3D ( 'NONE', #20408, #853, #26078 ) ;
#30966 = CARTESIAN_POINT ( 'NONE',  ( 12.46528703574805874, 63.59768628210145636, 2.660918448318279950 ) ) ;
#30967 = CARTESIAN_POINT ( 'NONE',  ( -2.908627838312119351, 5.522686282101450850, -15.53471296425195369 ) ) ;
#30969 = ADVANCED_FACE ( 'NONE', ( #14194 ), #11347, .F. ) ;
#30968 = CARTESIAN_POINT ( 'NONE',  ( 22.56230152254411792, 3.464101615137759271, -2.887500000000023270 ) ) ;
#30970 = LINE ( 'NONE', #13343, #30097 ) ;
#30971 = ORIENTED_EDGE ( 'NONE', *, *, #9243, .T. ) ;
#30972 = CARTESIAN_POINT ( 'NONE',  ( -3.257655550457281723, 29.09768628210144925, 15.46528703574804986 ) ) ;
#30973 = CARTESIAN_POINT ( 'NONE',  ( -27.24356964375000345, 195.2656250006145342, -15.72908226750537786 ) ) ;
#30974 = CARTESIAN_POINT ( 'NONE',  ( -13.62178482187500528, 198.4343750006145228, -23.59362340125807123 ) ) ;
#30975 = CARTESIAN_POINT ( 'NONE',  ( 36.82794601260381029, 7.347880794884125653E-16, 162.0719712953337250 ) ) ;
#30976 = CARTESIAN_POINT ( 'NONE',  ( 36.63184559142159458, 7.347880794884125653E-16, 159.8305332246273167 ) ) ;
#30977 = LINE ( 'NONE', #2151, #8732 ) ;
#30978 = CARTESIAN_POINT ( 'NONE',  ( -11.48171059495397373, 4.085186282101443744, -4.944772684328680334 ) ) ;
#30979 = CARTESIAN_POINT ( 'NONE',  ( 23.87821517812499650, 247.4593750006145285, -4.985214923628404904 ) ) ;
#30980 = CARTESIAN_POINT ( 'NONE',  ( -5.233372021372612259, 115.4523137178985479, 8.152565276336593669 ) ) ;
#30981 = CARTESIAN_POINT ( 'NONE',  ( 26.75643035624999655, 241.0843750006145285, -7.049594010296217766E-16 ) ) ;
#30982 = EDGE_LOOP ( 'NONE', ( #18629, #8606, #36201, #23204 ) ) ;
#30983 = CARTESIAN_POINT ( 'NONE',  ( -54.50000000000000711, 237.0000000000000000, 2.500000000000000000 ) ) ;
#30984 = CARTESIAN_POINT ( 'NONE',  ( 22.56230152254411792, 7.347880794884125653E-16, -6.975000000000036948 ) ) ;
#30985 = CARTESIAN_POINT ( 'NONE',  ( 15.00000000000000000, 248.2562500012290627, 0.000000000000000000 ) ) ;
#30986 = EDGE_CURVE ( 'NONE', #7963, #30563, #19242, .T. ) ;
#30987 = CARTESIAN_POINT ( 'NONE',  ( 12.46528703574811558, 121.2023137178985621, -2.660918448318005947 ) ) ;
#30988 = CARTESIAN_POINT ( 'NONE',  ( 10.31873187879411091, 3.604726614523236616, -8.278124999385530813 ) ) ;
#30989 = CARTESIAN_POINT ( 'NONE',  ( 27.71554269823568362, -5.407089921784859143, 162.5774681431477404 ) ) ;
#30990 = CARTESIAN_POINT ( 'NONE',  ( 26.75643035624999655, 3.323476615752271712, -0.8906249993854854496 ) ) ;
#30991 = CARTESIAN_POINT ( 'NONE',  ( 27.00000000000001066, 198.3875000000000171, 15.58845726811988897 ) ) ;
#30992 = ORIENTED_EDGE ( 'NONE', *, *, #13066, .F. ) ;
#30993 = CARTESIAN_POINT ( 'NONE',  ( -12.50000000000000355, 40.31018628210144783, -0.1745138560725492671 ) ) ;
#30994 = ORIENTED_EDGE ( 'NONE', *, *, #5518, .F. ) ;
#30995 = ORIENTED_EDGE ( 'NONE', *, *, #23537, .F. ) ;
#30996 = CARTESIAN_POINT ( 'NONE',  ( 18.00000000000000355, -5.196152422706632912, -4.818749998770965881 ) ) ;
#30997 = CARTESIAN_POINT ( 'NONE',  ( 26.75643035624999655, -3.323476615752267271, -1.753124999385447857 ) ) ;
#30998 = DIRECTION ( 'NONE',  ( 0.08715574274765150453, 0.000000000000000000, 0.9961946980917461003 ) ) ;
#30999 = DIRECTION ( 'NONE',  ( 0.08715574274765150453, 0.000000000000000000, 0.9961946980917461003 ) ) ;
#31000 = CARTESIAN_POINT ( 'NONE',  ( 21.00000000000000000, 248.2843750006145171, -6.646953231504538984 ) ) ;
#31001 = CARTESIAN_POINT ( 'NONE',  ( -8.962234695871760692, 66.76018628210145778, 8.715434833791933400 ) ) ;
#31002 = CARTESIAN_POINT ( 'NONE',  ( -67.80877896937849414, 211.6261429550004891, -6.530955311639245586 ) ) ;
#31003 = CARTESIAN_POINT ( 'NONE',  ( 14.82946893053589221, 216.1705310694575246, 0.5774388102998520012 ) ) ;
#31004 = CARTESIAN_POINT ( 'NONE',  ( -45.24627896937850835, 205.4690446883607535, -1.090244570138286351 ) ) ;
#31005 = ADVANCED_FACE ( 'NONE', ( #30882 ), #24999, .T. ) ;
#31006 = CARTESIAN_POINT ( 'NONE',  ( 36.99136303036276274, -3.464101615137751278, 163.9398363554801108 ) ) ;
#31007 = CARTESIAN_POINT ( 'NONE',  ( 10.69584247140429589, 122.3523137178985678, 6.932735513424201024 ) ) ;
#31008 = CARTESIAN_POINT ( 'NONE',  ( -66.43080436395490551, 205.4999999999999716, -0.1155267958017894420 ) ) ;
#31009 = CARTESIAN_POINT ( 'NONE',  ( -62.27455436395490551, 203.6929966515020283, 6.137860380172978303 ) ) ;
#31010 = CARTESIAN_POINT ( 'NONE',  ( 26.75643035624999655, 7.049594010296217766E-16, -2.728124999385489247 ) ) ;
#31011 = CARTESIAN_POINT ( 'NONE',  ( -27.24356964374999635, 195.7906250006145115, 15.72908226750539384 ) ) ;
#31012 = CARTESIAN_POINT ( 'NONE',  ( 11.08355503943118769, 95.03981371789855359, 10.83675517735179028 ) ) ;
#31013 = CARTESIAN_POINT ( 'NONE',  ( -66.42336230271182274, 217.4189793300686233, 4.149950860017807663 ) ) ;
#31014 = ORIENTED_EDGE ( 'NONE', *, *, #7976, .T. ) ;
#31015 = CARTESIAN_POINT ( 'NONE',  ( 4.944772684328679446, 125.9851862821014521, -11.48171059495397373 ) ) ;
#31016 = CARTESIAN_POINT ( 'NONE',  ( -8.632099005475501130, 69.34768628210143504, -13.23911966647218996 ) ) ;
#31017 = FACE_OUTER_BOUND ( 'NONE', #30436, .T. ) ;
#31018 = CARTESIAN_POINT ( 'NONE',  ( 37.28548217858939040, -3.604726614523238837, 164.5069853552165284 ) ) ;
#31019 = CARTESIAN_POINT ( 'NONE',  ( 15.46528703574804986, 91.19768628210145778, 3.257655550457285720 ) ) ;
#31020 = CARTESIAN_POINT ( 'NONE',  ( -44.46205436395489130, 214.6737587650351884, 4.842901733360205796 ) ) ;
#31021 = EDGE_CURVE ( 'NONE', #36053, #19993, #4246, .T. ) ;
#31022 = CARTESIAN_POINT ( 'NONE',  ( 19.68408634441910721, -5.407089921784855591, -7.640624999385531524 ) ) ;
#31023 = CARTESIAN_POINT ( 'NONE',  ( -9.465287035748065847, 12.99768628210143362, -2.064181346179273735 ) ) ;
#31024 = DIRECTION ( 'NONE',  ( 0.08715574274765150453, 0.000000000000000000, 0.9961946980917461003 ) ) ;
#31025 = CARTESIAN_POINT ( 'NONE',  ( -57.12872103062157692, 203.4690446883607535, 1.626142955000567936 ) ) ;
#31026 = LINE ( 'NONE', #19849, #1483 ) ;
#31027 = CARTESIAN_POINT ( 'NONE',  ( -2.660918448318275509, 56.69768628210145067, 12.46528703574805874 ) ) ;
#31028 = CARTESIAN_POINT ( 'NONE',  ( 13.49999999999999645, 196.7000000000000171, -23.38268590217984766 ) ) ;
#31029 = CYLINDRICAL_SURFACE ( 'NONE', #230, 6.000000000000001776 ) ;
#31031 = CARTESIAN_POINT ( 'NONE',  ( 16.56230152254411436, -7.209453229046482114, -2.334374999385512961 ) ) ;
#31030 = CARTESIAN_POINT ( 'NONE',  ( 6.840914352312096547, 34.56018628210144783, -6.594114490232313663 ) ) ;
#31032 = CARTESIAN_POINT ( 'NONE',  ( 20.99999999999999645, 247.9468750006144830, -6.646953231504538984 ) ) ;
#31033 = ORIENTED_EDGE ( 'NONE', *, *, #33476, .T. ) ;
#31034 = CARTESIAN_POINT ( 'NONE',  ( 21.00000000000000000, -6.928203230275506996, -3.037500000000010747 ) ) ;
#31035 = CARTESIAN_POINT ( 'NONE',  ( 25.07590970989797086, -4.251393452926127914, -7.999999999999994671 ) ) ;
#31036 = CARTESIAN_POINT ( 'NONE',  ( 29.48995970988985604, 6.148715791637016537, 159.4803054849043917 ) ) ;
#31037 = CARTESIAN_POINT ( 'NONE',  ( 22.80587116629410716, 7.646167579472015790E-16, -1.265624999385539518 ) ) ;
#31038 = CARTESIAN_POINT ( 'NONE',  ( 36.59262550718515428, 7.347880794884125653E-16, 159.3822456104860237 ) ) ;
#31039 = CARTESIAN_POINT ( 'NONE',  ( 24.00000000000000000, 243.8500000000000227, 5.196152422706629359 ) ) ;
#31040 = CARTESIAN_POINT ( 'NONE',  ( -56.70466238434235606, 244.2363183625454894, 7.500000000000000000 ) ) ;
#31041 = ADVANCED_FACE ( 'NONE', ( #32365 ), #26674, .F. ) ;
#31042 = CARTESIAN_POINT ( 'NONE',  ( -8.715434833792127023, 88.13981371789856212, 8.962234695871568846 ) ) ;
#31043 = CARTESIAN_POINT ( 'NONE',  ( -2.660918448318275509, 84.29768628210146630, 12.46528703574805874 ) ) ;
#31044 = ORIENTED_EDGE ( 'NONE', *, *, #908, .F. ) ;
#31045 = ORIENTED_EDGE ( 'NONE', *, *, #32573, .F. ) ;
#31046 = CARTESIAN_POINT ( 'NONE',  ( -1.909035429704832693E-15, 198.2000000012290286, -31.17691453623979214 ) ) ;
#31047 = LINE ( 'NONE', #10387, #8970 ) ;
#31048 = CARTESIAN_POINT ( 'NONE',  ( -8.927990412390371944, 63.12731371789852375, -13.04141134922778988 ) ) ;
#31049 = CARTESIAN_POINT ( 'NONE',  ( 18.12178482187500350, -4.985214923628407568, -10.07812499938548534 ) ) ;
#31050 = CARTESIAN_POINT ( 'NONE',  ( 18.12178482187499640, 242.1343750006145115, -4.985214923628404904 ) ) ;
#31051 = CARTESIAN_POINT ( 'NONE',  ( -54.15997103062156981, 213.8393509191290889, 2.350049139982164359 ) ) ;
#31052 = CARTESIAN_POINT ( 'NONE',  ( 14.99999999999978684, 3.464101615137630485, -6.281249998770925380 ) ) ;
#31053 = CARTESIAN_POINT ( 'NONE',  ( 5.529263428287300108, 40.12731371789853796, 7.954856959092309943 ) ) ;
#31054 = CARTESIAN_POINT ( 'NONE',  ( -67.02455436395489130, 205.1570982666397356, 4.673758765035198159 ) ) ;
#31055 = AXIS2_PLACEMENT_3D ( 'NONE', #10369, #9808, #21944 ) ;
#31056 = CARTESIAN_POINT ( 'NONE',  ( 6.594114490232462877, 101.9398137178985735, -6.840914352311949109 ) ) ;
#31057 = CARTESIAN_POINT ( 'NONE',  ( 27.24356964374999635, 199.2218750006145456, -15.72908226750539029 ) ) ;
#31058 = CARTESIAN_POINT ( 'NONE',  ( 7.228626920338837358, 12.52731371789855785, 10.49813415416005036 ) ) ;
#31059 = CARTESIAN_POINT ( 'NONE',  ( 8.715434833791931624, 55.26018628210144357, 8.962234695871760692 ) ) ;
#31060 = CARTESIAN_POINT ( 'NONE',  ( 22.56230152254410015, 7.347880794884117764E-16, -7.312499998771010645 ) ) ;
#31061 = CARTESIAN_POINT ( 'NONE',  ( 26.99999999999999645, 245.2375000000000114, 3.464101615137751278 ) ) ;
#31062 = CARTESIAN_POINT ( 'NONE',  ( 30.67183618977810156, -7.209453229046475009, 160.5495935129122245 ) ) ;
#31063 = DIRECTION ( 'NONE',  ( -1.000000000000000000, 0.000000000000000000, 0.000000000000000000 ) ) ;
#31064 = CARTESIAN_POINT ( 'NONE',  ( 10.31873187879410736, 3.604726614523240613, -7.434374999385486404 ) ) ;
#31065 = CARTESIAN_POINT ( 'NONE',  ( -43.77105176259354380, 253.6555389399068190, 5.000000000000000000 ) ) ;
#31066 = LINE ( 'NONE', #36176, #27237 ) ;
#31067 = CARTESIAN_POINT ( 'NONE',  ( 8.843639120294328748, 71.93518628210142651, -3.474262827703334722 ) ) ;
#31068 = CIRCLE ( 'NONE', #5029, 4.899999999999999467 ) ;
#31069 = CARTESIAN_POINT ( 'NONE',  ( 22.56230152254411792, 7.347880794884125653E-16, -6.075000000000052580 ) ) ;
#31070 = CARTESIAN_POINT ( 'NONE',  ( 0.1745138560725515708, 116.2101862821014606, -12.50000000000000355 ) ) ;
#31071 = LINE ( 'NONE', #22358, #21526 ) ;
#31072 = CARTESIAN_POINT ( 'NONE',  ( 24.00000000000000000, 240.3062500012290457, 5.196152422706629359 ) ) ;
#31073 = ORIENTED_EDGE ( 'NONE', *, *, #17731, .F. ) ;
#31074 = CARTESIAN_POINT ( 'NONE',  ( 37.17926111711567927, 3.604726614523238837, 163.2928730669172239 ) ) ;
#31075 = CARTESIAN_POINT ( 'NONE',  ( 15.24356964374999990, 0.000000000000000000, -5.540624999385457272 ) ) ;
#31076 = CARTESIAN_POINT ( 'NONE',  ( 27.24356964374999279, 197.8718750006145513, -15.72908226750539207 ) ) ;
#31077 = CARTESIAN_POINT ( 'NONE',  ( 31.39250523762275691, 7.209453229046482114, 168.7868784227583205 ) ) ;
#31078 = CARTESIAN_POINT ( 'NONE',  ( 37.22341519532126597, 3.464101615137759271, 166.5922047379250159 ) ) ;
#31079 = CARTESIAN_POINT ( 'NONE',  ( -29.00000000000002487, 210.0000000000000000, 0.000000000000000000 ) ) ;
#31080 = CARTESIAN_POINT ( 'NONE',  ( 18.12178482187500350, 240.4843750006145342, 4.985214923628407568 ) ) ;
#31081 = CARTESIAN_POINT ( 'NONE',  ( 20.99999999999997868, 210.0000000000000000, 0.000000000000000000 ) ) ;
#31082 = CARTESIAN_POINT ( 'NONE',  ( -8.715434833792127023, 134.1398137178985621, 8.962234695871568846 ) ) ;
#31083 = CARTESIAN_POINT ( 'NONE',  ( -20.86978606573367045, 194.8588513912095266, -17.51182790300216752 ) ) ;
#31085 = EDGE_LOOP ( 'NONE', ( #7365, #22696, #23742, #36666 ) ) ;
#31084 = ORIENTED_EDGE ( 'NONE', *, *, #33003, .F. ) ;
#31086 = CARTESIAN_POINT ( 'NONE',  ( 15.24356964374999990, 245.6968750006145115, 0.000000000000000000 ) ) ;
#31087 = CARTESIAN_POINT ( 'NONE',  ( -11.61527771782809282, 7.064813717898549505, -4.622313124798832717 ) ) ;
#31088 = CARTESIAN_POINT ( 'NONE',  ( 18.12178482187500350, -4.985214923628407568, -3.665624999385469707 ) ) ;
#31089 = CARTESIAN_POINT ( 'NONE',  ( -15.46528703574811736, 116.6023137178985394, 3.257655550456946436 ) ) ;
#31090 =( BOUNDED_CURVE ( )  B_SPLINE_CURVE ( 2, ( #37183, #36812, #33795, #22797, #10854, #28467, #36996 ),
 .UNSPECIFIED., .F., .F. ) 
 B_SPLINE_CURVE_WITH_KNOTS ( ( 3, 2, 2, 3 ),
 ( 0.2608695652173921298, 0.2681159420289864204, 0.2753623188405807110, 0.2826086956521749460 ),
 .UNSPECIFIED. ) 
 CURVE ( )  GEOMETRIC_REPRESENTATION_ITEM ( )  RATIONAL_B_SPLINE_CURVE ( ( 0.9999999999999845679, 0.8660254037844541397, 1.000000000000000000, 0.8660254037844387076, 1.000000000000000000, 0.8660254037844191677, 1.000000000000019540 ) ) 
 REPRESENTATION_ITEM ( '' )  );
#31091 = CARTESIAN_POINT ( 'NONE',  ( 19.56230152254412147, -5.196152422706635576, -9.750000000000063949 ) ) ;
#31092 = CARTESIAN_POINT ( 'NONE',  ( 21.00000000000000000, -6.646953231504538984, -1.040624999385473481 ) ) ;
#31093 = EDGE_CURVE ( 'NONE', #24290, #27888, #37355, .T. ) ;
#31094 = CARTESIAN_POINT ( 'NONE',  ( 10.31873187879410736, -3.604726614523244610, -8.259374999385515892 ) ) ;
#31095 = CARTESIAN_POINT ( 'NONE',  ( 27.00000000000001066, 198.5000000012290400, 15.58845726811988897 ) ) ;
#31096 = CARTESIAN_POINT ( 'NONE',  ( -2.311890736173176641, 106.7226862821014635, -12.53471296425194836 ) ) ;
#31097 = CARTESIAN_POINT ( 'NONE',  ( 10.31873187879411091, -3.604726614523240613, -2.353124999385527882 ) ) ;
#31098 = VECTOR ( 'NONE', #17977, 1000.000000000000000 ) ;
#31099 = CARTESIAN_POINT ( 'NONE',  ( -44.05877896937850124, 212.1620413398627534, -8.530955311639255356 ) ) ;
#31100 = CARTESIAN_POINT ( 'NONE',  ( 26.75643035624999655, 244.0843750006145285, 3.323476615752267271 ) ) ;
#31101 = CARTESIAN_POINT ( 'NONE',  ( 19.56230152254411792, -5.196152422706629359, -7.387499998771030363 ) ) ;
#31102 = CARTESIAN_POINT ( 'NONE',  ( -32.38169563604516554, 210.1155267958017703, 4.499999999999996447 ) ) ;
#31103 = CARTESIAN_POINT ( 'NONE',  ( -8.962234695871760692, 121.9601862821014464, 8.715434833791933400 ) ) ;
#31104 = CARTESIAN_POINT ( 'NONE',  ( 16.56230152254411081, -6.928203230275506996, -1.124999998771007759 ) ) ;
#31105 =( BOUNDED_CURVE ( )  B_SPLINE_CURVE ( 2, ( #21322, #29454, #18481, #32862, #32481, #12398, #32672 ),
 .UNSPECIFIED., .F., .F. ) 
 B_SPLINE_CURVE_WITH_KNOTS ( ( 3, 2, 2, 3 ),
 ( 0.6956521739130421267, 0.7028985507246364728, 0.7101449275362307079, 0.7173913043478249429 ),
 .UNSPECIFIED. ) 
 CURVE ( )  GEOMETRIC_REPRESENTATION_ITEM ( )  RATIONAL_B_SPLINE_CURVE ( ( 1.000000000000024647, 0.8660254037844140607, 1.000000000000000000, 0.8660254037844387076, 1.000000000000000000, 0.8660254037844592467, 0.9999999999999794609 ) ) 
 REPRESENTATION_ITEM ( '' )  );
#31106 = AXIS2_PLACEMENT_3D ( 'NONE', #32311, #26812, #27003 ) ;
#31107 = CARTESIAN_POINT ( 'NONE',  ( -42.08705436395489841, 205.3262412349647263, -4.842901733360204020 ) ) ;
#31108 = DIRECTION ( 'NONE',  ( 0.08715574274765150453, 0.000000000000000000, 0.9961946980917461003 ) ) ;
#31109 = CARTESIAN_POINT ( 'NONE',  ( -27.00000000000000355, 199.5124999999999886, -15.58845726811989429 ) ) ;
#31110 = CARTESIAN_POINT ( 'NONE',  ( -14.38691631536207183, 113.3351862821014606, 5.770363421893814682 ) ) ;
#31111 = CARTESIAN_POINT ( 'NONE',  ( -8.962234695871760692, 20.76018628210144001, 8.715434833791933400 ) ) ;
#31112 = CARTESIAN_POINT ( 'NONE',  ( 13.56230152254411614, -5.196152422706638241, -8.475000000000093792 ) ) ;
#31113 = CARTESIAN_POINT ( 'NONE',  ( 15.00000000000000000, 0.000000000000000000, -4.443749998770951670 ) ) ;
#31114 = ORIENTED_EDGE ( 'NONE', *, *, #15827, .F. ) ;
#31115 = DIRECTION ( 'NONE',  ( -0.000000000000000000, 1.000000000000000000, -0.000000000000000000 ) ) ;
#31116 = MECHANICAL_DESIGN_GEOMETRIC_PRESENTATION_REPRESENTATION (  '', ( #37159 ), #35337 ) ;
#31117 = CARTESIAN_POINT ( 'NONE',  ( 7.954856959092191815, 73.37268628210144072, 5.529263428287477744 ) ) ;
#31118 = AXIS2_PLACEMENT_3D ( 'NONE', #2975, #28750, #34447 ) ;
#31119 = SURFACE_SIDE_STYLE ('',( #1738 ) ) ;
#31120 = CARTESIAN_POINT ( 'NONE',  ( -13.62178482187498396, 196.2781250006145228, 23.59362340125808188 ) ) ;
#31121 = CARTESIAN_POINT ( 'NONE',  ( 22.56230152254410370, 0.000000000000000000, -10.00000000000000000 ) ) ;
#31122 = CARTESIAN_POINT ( 'NONE',  ( 27.24356964374999635, 196.9718750006145456, -15.72908226750539029 ) ) ;
#31123 = LINE ( 'NONE', #4952, #3498 ) ;
#31124 = CIRCLE ( 'NONE', #14779, 5.999999999999999112 ) ;
#31125 = CARTESIAN_POINT ( 'NONE',  ( 13.56230152254410726, 5.196152422706636465, -3.675000000000067324 ) ) ;
#31126 = CARTESIAN_POINT ( 'NONE',  ( -1.715153634034442431, 50.47731371789854649, 9.534712964251900402 ) ) ;
#31127 = CARTESIAN_POINT ( 'NONE',  ( 15.00000000000000000, 0.000000000000000000, -9.449999999999986855 ) ) ;
#31128 = VERTEX_POINT ( 'NONE', #35201 ) ;
#31129 = CARTESIAN_POINT ( 'NONE',  ( 21.00000000000000000, 240.7187500012290400, 6.928203230275506996 ) ) ;
#31130 = CARTESIAN_POINT ( 'NONE',  ( -2.660918448318005058, 54.50231371789855928, -12.46528703574811558 ) ) ;
#31131 = CARTESIAN_POINT ( 'NONE',  ( 16.56230152254411436, 7.209453229046482114, -6.159374999385525129 ) ) ;
#31132 = CARTESIAN_POINT ( 'NONE',  ( 26.75643035624999655, 3.323476615752271712, -5.840624999385470417 ) ) ;
#31133 = CARTESIAN_POINT ( 'NONE',  ( 8.715434833792128799, 28.33981371789855075, -8.962234695871567070 ) ) ;
#31134 = ORIENTED_EDGE ( 'NONE', *, *, #24239, .F. ) ;
#31135 = CARTESIAN_POINT ( 'NONE',  ( 10.31873187879410381, 3.604726614523240613, -2.484374999385501326 ) ) ;
#31136 = CARTESIAN_POINT ( 'NONE',  ( 22.56230152254410370, 0.000000000000000000, -10.00000000000000000 ) ) ;
#31137 = CARTESIAN_POINT ( 'NONE',  ( 28.22050128277989245, -5.407089921784865361, 168.3491711752168385 ) ) ;
#31138 = CARTESIAN_POINT ( 'NONE',  ( -43.26711230271183695, 216.4690446883607535, -1.857196546604089393 ) ) ;
#31139 = LINE ( 'NONE', #30450, #23442 ) ;
#31140 =( BOUNDED_CURVE ( )  B_SPLINE_CURVE ( 2, ( #14885, #35147, #3503, #20961, #21336, #17922, #32493 ),
 .UNSPECIFIED., .F., .F. ) 
 B_SPLINE_CURVE_WITH_KNOTS ( ( 3, 2, 2, 3 ),
 ( 0.1521739130434776044, 0.1594202898550718950, 0.1666666666666661856, 0.1739130434782605039 ),
 .UNSPECIFIED. ) 
 CURVE ( )  GEOMETRIC_REPRESENTATION_ITEM ( )  RATIONAL_B_SPLINE_CURVE ( ( 1.000000000000012212, 0.8660254037844263841, 1.000000000000000000, 0.8660254037844387076, 1.000000000000000000, 0.8660254037844453689, 0.9999999999999933387 ) ) 
 REPRESENTATION_ITEM ( '' )  );
#31141 = CARTESIAN_POINT ( 'NONE',  ( 15.00000000000037481, -3.464101615137971546, -7.612499999999990941 ) ) ;
#31142 = CARTESIAN_POINT ( 'NONE',  ( -39.90997103062156270, 213.8393509191290889, 2.350049139982164359 ) ) ;
#31144 = EDGE_CURVE ( 'NONE', #20323, #24000, #23287, .T. ) ;
#31143 = CARTESIAN_POINT ( 'NONE',  ( -44.46205436395488420, 214.6737587650352168, 4.842901733360204908 ) ) ;
#31145 = ORIENTED_EDGE ( 'NONE', *, *, #34158, .F. ) ;
#31146 = CARTESIAN_POINT ( 'NONE',  ( 16.56230152254410726, 0.000000000000000000, -10.00000000000000000 ) ) ;
#31147 = CARTESIAN_POINT ( 'NONE',  ( -5.732297079746171420, 222.9518338469886203, -2.500000000000000000 ) ) ;
#31148 = CARTESIAN_POINT ( 'NONE',  ( 8.927990412390371944, 40.12731371789853796, 13.04141134922778811 ) ) ;
#31149 = CARTESIAN_POINT ( 'NONE',  ( -35.74627896937850124, 201.4690446883607251, -2.162041339862721845 ) ) ;
#31150 = CARTESIAN_POINT ( 'NONE',  ( 4.944772684328679446, 15.58518628210145351, -11.48171059495397373 ) ) ;
#31151 = CARTESIAN_POINT ( 'NONE',  ( 4.622313124798573369, 74.23518628210145209, 11.61527771782819940 ) ) ;
#31152 = CARTESIAN_POINT ( 'NONE',  ( 14.25334919248782661, 17.88518628210143646, 6.092822981423971385 ) ) ;
#31153 = CARTESIAN_POINT ( 'NONE',  ( 16.56230152254411436, -6.928203230275514990, -3.037500000000043165 ) ) ;
#31154 = CARTESIAN_POINT ( 'NONE',  ( 26.99999999999999645, 194.9750000012290343, -15.58845726811990495 ) ) ;
#31155 = ORIENTED_EDGE ( 'NONE', *, *, #19573, .T. ) ;
#31156 = CARTESIAN_POINT ( 'NONE',  ( 13.23911966647218996, 34.84768628210143504, -8.632099005475504683 ) ) ;
#31157 = DIRECTION ( 'NONE',  ( -1.000000000000000000, -0.000000000000000000, 5.782411586589356653E-16 ) ) ;
#31158 = CARTESIAN_POINT ( 'NONE',  ( 13.62178482187499640, 198.8093750006145513, -23.59362340125807123 ) ) ;
#31159 = CARTESIAN_POINT ( 'NONE',  ( -6.000000000000000888, -30.00000000000000000, -19.99999999999999289 ) ) ;
#31160 = CARTESIAN_POINT ( 'NONE',  ( 25.29195720079856713, 3.464101615137683332, 167.8995747603702853 ) ) ;
#31161 = CARTESIAN_POINT ( 'NONE',  ( 26.99999999999999645, 7.347880794884117764E-16, -5.568749998770966769 ) ) ;
#31162 = CARTESIAN_POINT ( 'NONE',  ( 18.00000000000000355, 247.8249999999999886, 5.196152422706632912 ) ) ;
#31163 = CARTESIAN_POINT ( 'NONE',  ( 26.75643035624999655, 246.8968750006145285, 3.323476615752267715 ) ) ;
#31164 = CARTESIAN_POINT ( 'NONE',  ( -6.840914352311947333, 108.8398137178985507, -6.594114490232462877 ) ) ;
#31165 = CARTESIAN_POINT ( 'NONE',  ( 18.12178482187499640, 241.6843750006145513, -4.985214923628404904 ) ) ;
#31166 = VERTEX_POINT ( 'NONE', #14754 ) ;
#31167 = CARTESIAN_POINT ( 'NONE',  ( -68.21205436395489130, 214.6737587650352168, 4.842901733360204908 ) ) ;
#31168 = CARTESIAN_POINT ( 'NONE',  ( 19.56230152254412502, -5.196152422706635576, -7.050000000000084199 ) ) ;
#31169 = EDGE_CURVE ( 'NONE', #32379, #10385, #7420, .T. ) ;
#31170 = CARTESIAN_POINT ( 'NONE',  ( 21.00000000000000000, 248.5937500012290116, -6.928203230275506996 ) ) ;
#31171 = CARTESIAN_POINT ( 'NONE',  ( 12.53471296425189330, 112.5773137178985621, 2.311890736173451533 ) ) ;
#31172 = CARTESIAN_POINT ( 'NONE',  ( 22.80587116629411071, 3.604726614523238837, -9.778124999385537919 ) ) ;
#31173 = CARTESIAN_POINT ( 'NONE',  ( 24.52066036092156054, 0.000000000000000000, 161.8782597873571660 ) ) ;
#31174 = CARTESIAN_POINT ( 'NONE',  ( 30.91941297146709644, -6.928203230275514990, 163.3794090765669011 ) ) ;
#31175 = CARTESIAN_POINT ( 'NONE',  ( -27.24356964375000345, 198.9593750006145285, 0.000000000000000000 ) ) ;
#31176 = ORIENTED_EDGE ( 'NONE', *, *, #23016, .F. ) ;
#31177 = ORIENTED_EDGE ( 'NONE', *, *, #23485, .F. ) ;
#31178 = EDGE_LOOP ( 'NONE', ( #24817, #21813, #30855, #19154, #3099, #5989, #8233, #31671 ) ) ;
#31179 = CARTESIAN_POINT ( 'NONE',  ( 26.99999999999999645, 7.347880794884117764E-16, -4.218749998770948473 ) ) ;
#31180 = CARTESIAN_POINT ( 'NONE',  ( 20.99999999999999645, 6.646953231504538984, -2.953124999385479121 ) ) ;
#31181 = LINE ( 'NONE', #28506, #10631 ) ;
#31182 = CARTESIAN_POINT ( 'NONE',  ( 25.40308077269482112, 0.000000000000000000, 169.1697229992128939 ) ) ;
#31183 = CARTESIAN_POINT ( 'NONE',  ( 10.49813415415989581, 64.17268628210143788, 7.228626920339068285 ) ) ;
#31184 = CARTESIAN_POINT ( 'NONE',  ( -67.41294563604516554, 214.6737587650350747, -4.842901733360248429 ) ) ;
#31185 = CARTESIAN_POINT ( 'NONE',  ( 14.89154389910886600, 216.1084561008947844, -0.4848545222721730164 ) ) ;
#31186 = CARTESIAN_POINT ( 'NONE',  ( -48.01711230271184405, 214.4690446883608104, -1.321298161741814914 ) ) ;
#31187 = LINE ( 'NONE', #1995, #27496 ) ;
#31188 = CARTESIAN_POINT ( 'NONE',  ( 25.01741661114358450, 3.464101615137752166, 164.7615614613812625 ) ) ;
#31189 = CARTESIAN_POINT ( 'NONE',  ( -4.944772684328424539, 127.8148137178985735, -11.48171059495408031 ) ) ;
#31190 = CARTESIAN_POINT ( 'NONE',  ( -35.35788769728823411, 216.4690446883607535, 1.857196546604031662 ) ) ;
#31191 = CARTESIAN_POINT ( 'NONE',  ( -41.49330436395490551, 210.1155267958016850, -8.500000000000003553 ) ) ;
#31192 = CARTESIAN_POINT ( 'NONE',  ( 26.75643035624999655, -3.323476615752267271, -2.315624999385466509 ) ) ;
#31193 = CARTESIAN_POINT ( 'NONE',  ( 27.24356964375000345, 196.8781250006145171, -3.336375036156643733E-15 ) ) ;
#31194 = CARTESIAN_POINT ( 'NONE',  ( -11.08355503943118592, 99.63981371789857633, -10.83675517735179383 ) ) ;
#31195 = CARTESIAN_POINT ( 'NONE',  ( -66.81919563604516554, 218.5000000000000000, -0.1155267958018185298 ) ) ;
#31196 = VERTEX_POINT ( 'NONE', #517 ) ;
#31197 = DIRECTION ( 'NONE',  ( -1.558072081575740353E-16, -1.134704379232807653E-16, -1.000000000000000000 ) ) ;
#31198 = CARTESIAN_POINT ( 'NONE',  ( -11.48171059495397373, 114.4851862821014521, -4.944772684328680334 ) ) ;
#31199 = CARTESIAN_POINT ( 'NONE',  ( 15.50000000000000533, 63.31018628210144783, 0.1745138560725827404 ) ) ;
#31200 = AXIS2_PLACEMENT_3D ( 'NONE', #27631, #36714, #18749 ) ;
#31201 = DIRECTION ( 'NONE',  ( 1.000000000000000000, 0.000000000000000000, 2.057406622567553516E-16 ) ) ;
#31202 = CARTESIAN_POINT ( 'NONE',  ( 37.05343001352376575, 7.646167579472024665E-16, 161.8546169715473013 ) ) ;
#31203 = CARTESIAN_POINT ( 'NONE',  ( 15.50000000000000533, 90.91018628210146346, 0.1745138560725827404 ) ) ;
#31204 = CARTESIAN_POINT ( 'NONE',  ( 22.80587116629411071, -3.604726614523235284, -7.603124999385552307 ) ) ;
#31205 = CARTESIAN_POINT ( 'NONE',  ( 0.1745138560725194299, 15.01018628210143291, -9.500000000000005329 ) ) ;
#31206 = CARTESIAN_POINT ( 'NONE',  ( -63.06622103062156981, 211.6261429550005744, 6.530955311639227823 ) ) ;
#31207 = CARTESIAN_POINT ( 'NONE',  ( -10.49813415415989581, 59.57268628210145778, -7.228626920339068285 ) ) ;
#31208 = CARTESIAN_POINT ( 'NONE',  ( 13.49999999999999645, 197.1500000000000057, -23.38268590217984766 ) ) ;
#31209 = DIRECTION ( 'NONE',  ( 0.000000000000000000, 0.000000000000000000, -1.000000000000000000 ) ) ;
#31211 = CARTESIAN_POINT ( 'NONE',  ( 10.31873187879410914, 0.000000000000000000, -0.1968749993855323233 ) ) ;
#31210 = CARTESIAN_POINT ( 'NONE',  ( -9.534712964251941258, 30.82268628210143291, 1.715153634034234154 ) ) ;
#31212 = CARTESIAN_POINT ( 'NONE',  ( 15.24356964375000167, 248.5468750006145342, 3.323476615752272600 ) ) ;
#31213 = ORIENTED_EDGE ( 'NONE', *, *, #35754, .F. ) ;
#31214 = CARTESIAN_POINT ( 'NONE',  ( 23.99999999999999645, 5.196152422706631135, -3.750000000000003553 ) ) ;
#31215 = CARTESIAN_POINT ( 'NONE',  ( 26.30554917760220590, -2.480918870684495126, -8.000000000000003553 ) ) ;
#31216 = CARTESIAN_POINT ( 'NONE',  ( 27.63220001923324176, -5.407089921784865361, 161.6248569630975283 ) ) ;
#31217 = CARTESIAN_POINT ( 'NONE',  ( 10.31873187879410736, 3.604726614523236616, -1.978124999385525662 ) ) ;
#31218 = CARTESIAN_POINT ( 'NONE',  ( 34.49097153452227360, -5.407089921784855591, 168.3840463937848995 ) ) ;
#31219 = CARTESIAN_POINT ( 'NONE',  ( 21.00000000000000000, 243.5875000000000057, -6.928203230275506996 ) ) ;
#31220 = DIRECTION ( 'NONE',  ( 0.000000000000000000, 1.000000000000000000, 0.000000000000000000 ) ) ;
#31221 = CARTESIAN_POINT ( 'NONE',  ( -12.46528703574805874, 86.59768628210146346, -2.660918448318280838 ) ) ;
#31222 = ORIENTED_EDGE ( 'NONE', *, *, #35785, .F. ) ;
#31223 = VERTEX_POINT ( 'NONE', #29521 ) ;
#31224 = VECTOR ( 'NONE', #8648, 1000.000000000000000 ) ;
#31225 = CARTESIAN_POINT ( 'NONE',  ( -26.99999999999998934, 194.7500000012290400, 15.58845726811991561 ) ) ;
#31226 = CARTESIAN_POINT ( 'NONE',  ( 24.78209610572444532, 3.464101615137476831, 162.0718357765335895 ) ) ;
#31227 = CARTESIAN_POINT ( 'NONE',  ( 14.25334919248795451, 47.31481371789856638, -6.092822981423661410 ) ) ;
#31228 = CARTESIAN_POINT ( 'NONE',  ( 15.24356964374999990, 3.323476615752268604, -7.940624999385462068 ) ) ;
#31229 = AXIS2_PLACEMENT_3D ( 'NONE', #35818, #6827, #29952 ) ;
#31230 = CARTESIAN_POINT ( 'NONE',  ( 26.75643035624999655, 241.9843750006145342, -7.049594010296217766E-16 ) ) ;
#31231 = CARTESIAN_POINT ( 'NONE',  ( -49.80580436395490551, 214.5000000000000284, 0.1155267958017899832 ) ) ;
#31232 = CARTESIAN_POINT ( 'NONE',  ( 18.00000000000000000, 5.196152422706630247, -6.318749998770966769 ) ) ;
#31233 = CARTESIAN_POINT ( 'NONE',  ( 33.93698784468253393, -5.407089921784861808, 162.0519838440392562 ) ) ;
#31234 = CARTESIAN_POINT ( 'NONE',  ( -9.534712964251895073, 34.37731371789854506, -1.715153634034446428 ) ) ;
#31235 = CARTESIAN_POINT ( 'NONE',  ( 37.06326651802246630, 7.347880794884125653E-16, 164.7616969801814548 ) ) ;
#31236 = CARTESIAN_POINT ( 'NONE',  ( 9.500000000000005329, 103.0898137178985792, -0.1745138560723090149 ) ) ;
#31237 = CARTESIAN_POINT ( 'NONE',  ( 13.62178482187499640, 199.2593750006145399, -23.59362340125807123 ) ) ;
#31238 = CARTESIAN_POINT ( 'NONE',  ( -8.632099005475794229, 143.0523137178985280, 13.23911966647199812 ) ) ;
#31239 = EDGE_CURVE ( 'NONE', #10799, #14365, #27465, .T. ) ;
#31240 = CARTESIAN_POINT ( 'NONE',  ( 11.48171059495397728, 63.88518628210145067, 4.944772684328674117 ) ) ;
#31241 = CARTESIAN_POINT ( 'NONE',  ( 10.56230152254411259, -3.464101615137757051, -9.749999998770984888 ) ) ;
#31242 = EDGE_CURVE ( 'NONE', #20323, #37392, #37176, .T. ) ;
#31243 = CARTESIAN_POINT ( 'NONE',  ( 37.01584409946383403, -3.604726614523235284, 161.4250080079952170 ) ) ;
#31244 = CARTESIAN_POINT ( 'NONE',  ( 19.83830452692372148, 6.917534487978463709, -10.24872752355802064 ) ) ;
#31245 = CARTESIAN_POINT ( 'NONE',  ( 13.44051670066910908, 5.407089921784862696, -6.571874999385523886 ) ) ;
#31246 = CARTESIAN_POINT ( 'NONE',  ( -27.00000000000000355, 199.8312500006145171, 0.000000000000000000 ) ) ;
#31247 = CARTESIAN_POINT ( 'NONE',  ( -27.24356964375000345, 199.3156250006145171, -15.72908226750537786 ) ) ;
#31248 = CARTESIAN_POINT ( 'NONE',  ( 7.954856959092191815, 82.57268628210144357, 5.529263428287477744 ) ) ;
#31249 = DIRECTION ( 'NONE',  ( -0.000000000000000000, -1.000000000000000000, -0.000000000000000000 ) ) ;
#31250 =( GEOMETRIC_REPRESENTATION_CONTEXT ( 3 ) GLOBAL_UNCERTAINTY_ASSIGNED_CONTEXT ( ( #33969 ) ) GLOBAL_UNIT_ASSIGNED_CONTEXT ( ( #32358, #18345, #35014 ) ) REPRESENTATION_CONTEXT ( 'NONE', 'WORKASPACE' ) );
#31251 = EDGE_CURVE ( 'NONE', #31166, #29332, #13564, .T. ) ;
#31252 = CARTESIAN_POINT ( 'NONE',  ( -10.69584247140444866, 122.2476862821014549, 6.932735513423972762 ) ) ;
#31253 = CARTESIAN_POINT ( 'NONE',  ( 1.120210788295102201E-13, 195.8375000000000057, -27.00000000000000711 ) ) ;
#31254 = CARTESIAN_POINT ( 'NONE',  ( 21.00000000000000000, 248.3687500012290741, 5.999999999999998224 ) ) ;
#31255 = ORIENTED_EDGE ( 'NONE', *, *, #12973, .T. ) ;
#31256 = CARTESIAN_POINT ( 'NONE',  ( 30.84832656884210067, 7.209453229046475009, 162.5668877765479863 ) ) ;
#31257 = CARTESIAN_POINT ( 'NONE',  ( 15.24356964374999990, 0.000000000000000000, -4.190624999385467397 ) ) ;
#31258 = CARTESIAN_POINT ( 'NONE',  ( -27.24356964375000345, 195.3593750006145342, 0.000000000000000000 ) ) ;
#31259 = CARTESIAN_POINT ( 'NONE',  ( 31.31406506914986920, 7.209453229046482114, 167.8903031944757629 ) ) ;
#31260 = CARTESIAN_POINT ( 'NONE',  ( 37.18092677073180141, 7.347880794884125653E-16, 166.1065598226053055 ) ) ;
#31261 = DIRECTION ( 'NONE',  ( 0.000000000000000000, 0.000000000000000000, 1.000000000000000000 ) ) ;
#31262 = CARTESIAN_POINT ( 'NONE',  ( 21.00000000000000000, 241.1968750006145399, -6.646953231504538984 ) ) ;
#31263 = CARTESIAN_POINT ( 'NONE',  ( 36.99789971106840625, 3.464101615138000856, 164.0145509578370024 ) ) ;
#31264 = CARTESIAN_POINT ( 'NONE',  ( 10.69584247140429589, 122.3523137178985678, 6.932735513424201024 ) ) ;
#31265 = CARTESIAN_POINT ( 'NONE',  ( 12.46528703574805874, 137.1976862821014720, 2.660918448318279950 ) ) ;
#31267 = ORIENTED_EDGE ( 'NONE', *, *, #17592, .F. ) ;
#31266 = EDGE_LOOP ( 'NONE', ( #29807, #11199, #27433, #31844 ) ) ;
#31268 = CARTESIAN_POINT ( 'NONE',  ( 18.12178482187500350, 244.4218750006145058, 4.985214923628407568 ) ) ;
#31269 = CIRCLE ( 'NONE', #11273, 9.999999999999994671 ) ;
#31270 = CARTESIAN_POINT ( 'NONE',  ( 7.228626920338837358, 12.52731371789855785, 10.49813415416005036 ) ) ;
#31271 = CARTESIAN_POINT ( 'NONE',  ( 26.75643035624999655, 7.049594010296217766E-16, -6.215624999385465976 ) ) ;
#31272 = CARTESIAN_POINT ( 'NONE',  ( -13.23911966647199812, 108.5523137178985422, -8.632099005475788900 ) ) ;
#31273 = CARTESIAN_POINT ( 'NONE',  ( 22.56230152254432042, 3.464101615137637147, -2.437500000000029310 ) ) ;
#31274 = CARTESIAN_POINT ( 'NONE',  ( 23.87821517812500005, -4.985214923628404016, -1.453124999385491112 ) ) ;
#31275 = CARTESIAN_POINT ( 'NONE',  ( 16.56230152254411436, -7.209453229046482114, -8.634374999385517668 ) ) ;
#31276 = CARTESIAN_POINT ( 'NONE',  ( -13.49999999999998401, 199.2875000012290627, 23.38268590217985476 ) ) ;
#31277 = CARTESIAN_POINT ( 'NONE',  ( -8.715434833791929847, 115.0601862821014549, -8.962234695871762469 ) ) ;
#31278 = CARTESIAN_POINT ( 'NONE',  ( 16.56230152254411081, -7.209453229046475009, -2.728124999385529215 ) ) ;
#31279 = CARTESIAN_POINT ( 'NONE',  ( -46.23586230271182984, 205.8500491399821613, 7.418979330068642852 ) ) ;
#31280 = CARTESIAN_POINT ( 'NONE',  ( 26.75643035624999655, 243.7093750006144717, -3.323476615752271268 ) ) ;
#31281 = CARTESIAN_POINT ( 'NONE',  ( -29.00000000000002487, 222.9518338469886203, 12.50000000000000000 ) ) ;
#31282 = CARTESIAN_POINT ( 'NONE',  ( -30.79836230271183339, 206.0451222850691977, -2.149950860017851184 ) ) ;
#31283 = CARTESIAN_POINT ( 'NONE',  ( 12.53471296425194836, 118.2226862821014635, -2.311890736173178418 ) ) ;
#31284 = CARTESIAN_POINT ( 'NONE',  ( 13.56230152254410726, 5.196152422706630247, -3.112499998771029119 ) ) ;
#31285 = EDGE_CURVE ( 'NONE', #14644, #6593, #3532, .T. ) ;
#31286 = CARTESIAN_POINT ( 'NONE',  ( -43.86830436395490551, 209.8844732041982581, 6.500000000000000888 ) ) ;
#31287 = DIRECTION ( 'NONE',  ( 0.000000000000000000, 0.000000000000000000, 1.000000000000000000 ) ) ;
#31288 = CARTESIAN_POINT ( 'NONE',  ( -0.5000000000000052180, 244.5000000000000000, -10.00000000000000000 ) ) ;
#31289 = CARTESIAN_POINT ( 'NONE',  ( -10.83675517735155047, 105.8601862821014379, -11.08355503943142750 ) ) ;
#31290 = CARTESIAN_POINT ( 'NONE',  ( 6.932735513423970097, 9.547686282101450317, 10.69584247140445044 ) ) ;
#31291 = CARTESIAN_POINT ( 'NONE',  ( -51.40635080957662950, 236.9611623878118110, 5.000000000000000000 ) ) ;
#31292 = CARTESIAN_POINT ( 'NONE',  ( 8.152565276336714462, 126.8476862821014635, -5.233372021372432847 ) ) ;
#31293 = CARTESIAN_POINT ( 'NONE',  ( 22.80587116629410360, 7.646167579472015790E-16, -1.715624999385545468 ) ) ;
#31294 = DIRECTION ( 'NONE',  ( 0.000000000000000000, 0.000000000000000000, 1.000000000000000000 ) ) ;
#31295 = EDGE_LOOP ( 'NONE', ( #13909, #21002 ) ) ;
#31296 = CARTESIAN_POINT ( 'NONE',  ( 25.48152094116770883, 0.000000000000000000, 170.0662982274954800 ) ) ;
#31297 = CARTESIAN_POINT ( 'NONE',  ( -6.840914352312096547, 57.56018628210145494, 6.594114490232313663 ) ) ;
#31298 = CARTESIAN_POINT ( 'NONE',  ( 13.62178482187499640, 196.5031250006145456, -23.59362340125807123 ) ) ;
#31300 = DIRECTION ( 'NONE',  ( 0.9961946980917462113, 0.000000000000000000, -0.08715574274765118534 ) ) ;
#31299 =( BOUNDED_CURVE ( )  B_SPLINE_CURVE ( 2, ( #24746, #30251, #35554, #4278, #9599, #21361, #18326, #1054, #36116 ),
 .UNSPECIFIED., .F., .F. ) 
 B_SPLINE_CURVE_WITH_KNOTS ( ( 3, 2, 2, 2, 3 ),
 ( 0.5760869565217391353, 0.5797101449275362528, 0.5869565217391304879, 0.5942028985507246119, 0.5978260869565217295 ),
 .UNSPECIFIED. ) 
 CURVE ( )  GEOMETRIC_REPRESENTATION_ITEM ( )  RATIONAL_B_SPLINE_CURVE ( ( 0.9330127018922194093, 0.9330127018922194093, 1.000000000000000000, 0.8660254037844387076, 1.000000000000000000, 0.8660254037844387076, 1.000000000000000000, 0.9330127018922194093, 0.9330127018922194093 ) ) 
 REPRESENTATION_ITEM ( '' )  );
#31301 = CARTESIAN_POINT ( 'NONE',  ( -1.926257025242585782E-15, 196.1468750006145285, -31.45816453501075927 ) ) ;
#31302 = CARTESIAN_POINT ( 'NONE',  ( -69.00000000000002842, 204.5000000000000000, 0.000000000000000000 ) ) ;
#31303 = DIRECTION ( 'NONE',  ( -0.000000000000000000, 1.000000000000000000, -0.000000000000000000 ) ) ;
#31304 = CARTESIAN_POINT ( 'NONE',  ( 9.500000000000005329, 47.88981371789855501, -0.1745138560723090149 ) ) ;
#31305 = CARTESIAN_POINT ( 'NONE',  ( 26.99999999999999645, 7.347880794884117764E-16, -9.225000000000010303 ) ) ;
#31306 = ORIENTED_EDGE ( 'NONE', *, *, #4954, .F. ) ;
#31307 = CARTESIAN_POINT ( 'NONE',  ( 21.00000000000000000, 241.1687500012290570, 6.928203230275506996 ) ) ;
#31308 = CARTESIAN_POINT ( 'NONE',  ( 7.228626920338837358, 67.72731371789855359, 10.49813415416005036 ) ) ;
#31309 = CARTESIAN_POINT ( 'NONE',  ( 22.80587116629411781, -3.604726614523238837, -7.209374999385536498 ) ) ;
#31310 = CARTESIAN_POINT ( 'NONE',  ( 18.12178482187499640, 4.985214923628404904, -7.528124999385488181 ) ) ;
#31311 = CARTESIAN_POINT ( 'NONE',  ( 2.660918448318002838, 22.30231371789854933, 12.46528703574811558 ) ) ;
#31312 = ORIENTED_EDGE ( 'NONE', *, *, #2314, .T. ) ;
#31313 = CARTESIAN_POINT ( 'NONE',  ( 10.31873187879410558, 0.000000000000000000, -1.546874999385550176 ) ) ;
#31314 = CARTESIAN_POINT ( 'NONE',  ( 15.00000000000000000, 246.0062500012290627, 0.000000000000000000 ) ) ;
#31315 = CARTESIAN_POINT ( 'NONE',  ( 31.31406506914986920, 7.209453229046482114, 167.8903031944757629 ) ) ;
#31316 =( BOUNDED_CURVE ( )  B_SPLINE_CURVE ( 2, ( #11325, #25912, #22895, #37457, #34442, #31598, #11507, #34622, #23263 ),
 .UNSPECIFIED., .F., .F. ) 
 B_SPLINE_CURVE_WITH_KNOTS ( ( 3, 2, 2, 2, 3 ),
 ( 0.6413043478260869179, 0.6449275362318840354, 0.6521739130434782705, 0.6594202898550725056, 0.6630434782608695121 ),
 .UNSPECIFIED. ) 
 CURVE ( )  GEOMETRIC_REPRESENTATION_ITEM ( )  RATIONAL_B_SPLINE_CURVE ( ( 0.9330127018922194093, 0.9330127018922194093, 1.000000000000000000, 0.8660254037844387076, 1.000000000000000000, 0.8660254037844387076, 1.000000000000000000, 0.9330127018922202975, 0.9330127018922192983 ) ) 
 REPRESENTATION_ITEM ( '' )  );
#31317 = CARTESIAN_POINT ( 'NONE',  ( -40.69419563604516554, 203.5000000000000000, 0.1155267958017914542 ) ) ;
#31318 = CYLINDRICAL_SURFACE ( 'NONE', #31901, 2.649999999999992806 ) ;
#31319 = SURFACE_STYLE_FILL_AREA ( #218 ) ;
#31320 = CARTESIAN_POINT ( 'NONE',  ( 20.99999999999999645, -6.928203230275506996, -7.537500000000000533 ) ) ;
#31321 = CARTESIAN_POINT ( 'NONE',  ( -38.12872103062156270, 205.4690446883607535, 1.090244570138264368 ) ) ;
#31322 = CARTESIAN_POINT ( 'NONE',  ( -48.02455436395488420, 205.1570982666397356, 4.673758765035198159 ) ) ;
#31323 = ORIENTED_EDGE ( 'NONE', *, *, #23362, .T. ) ;
#31324 = CARTESIAN_POINT ( 'NONE',  ( 26.97716818855048260, 0.000000000000000000, 49.47706554351410801 ) ) ;
#31325 = CARTESIAN_POINT ( 'NONE',  ( 15.00000000000054712, 3.464101615138070134, -1.331249998770982046 ) ) ;
#31326 = CARTESIAN_POINT ( 'NONE',  ( -10.83675517735179028, 32.93981371789854506, 11.08355503943118947 ) ) ;
#31327 = CARTESIAN_POINT ( 'NONE',  ( -68.01413769728823411, 214.1499508600179240, 7.418979330068584233 ) ) ;
#31328 = CARTESIAN_POINT ( 'NONE',  ( -3.796722387233375073, 139.7851862821014493, 8.710071997420127943 ) ) ;
#31329 = CARTESIAN_POINT ( 'NONE',  ( -10.69584247140444866, 57.84768628210144925, 6.932735513423972762 ) ) ;
#31330 = CARTESIAN_POINT ( 'NONE',  ( 10.56230152254410726, 0.000000000000000000, -3.150000000000041656 ) ) ;
#31331 = LINE ( 'NONE', #26526, #31889 ) ;
#31332 = VERTEX_POINT ( 'NONE', #17607 ) ;
#31333 = CARTESIAN_POINT ( 'NONE',  ( 2.908627838312118019, 19.32268628210144001, 15.53471296425195369 ) ) ;
#31334 = LINE ( 'NONE', #28117, #9705 ) ;
#31335 = CARTESIAN_POINT ( 'NONE',  ( -27.24356964374999635, 199.4468750006145399, 15.72908226750539384 ) ) ;
#31336 = CARTESIAN_POINT ( 'NONE',  ( -71.06414469631722852, 221.4078028065942476, 7.500000000000000000 ) ) ;
#31337 =( NAMED_UNIT ( * ) SI_UNIT ( $, .STERADIAN. ) SOLID_ANGLE_UNIT ( ) );
#31338 = DIRECTION ( 'NONE',  ( 0.000000000000000000, 0.000000000000000000, 1.000000000000000000 ) ) ;
#31339 = CARTESIAN_POINT ( 'NONE',  ( -2.660918448318275509, 10.69768628210143646, 12.46528703574805874 ) ) ;
#31340 = CARTESIAN_POINT ( 'NONE',  ( 26.75643035624999655, 247.8718750006145228, -3.323476615752271712 ) ) ;
#31341 = CARTESIAN_POINT ( 'NONE',  ( 8.843639120294245259, 103.6648137178985678, 3.474262827703527901 ) ) ;
#31342 = CARTESIAN_POINT ( 'NONE',  ( 15.24356964375000167, 242.2468750006145228, 3.323476615752272600 ) ) ;
#31343 = EDGE_LOOP ( 'NONE', ( #33695, #4880, #12709, #27299, #17331 ) ) ;
#31344 = CARTESIAN_POINT ( 'NONE',  ( -67.61830436395489130, 209.8844732041982581, 6.500000000000000888 ) ) ;
#31345 = CARTESIAN_POINT ( 'NONE',  ( -7.234628195640354420, 196.0424038105676630, 26.99999999999996803 ) ) ;
#31346 = CARTESIAN_POINT ( 'NONE',  ( 18.00000000000000355, 247.8812500012290343, 5.196152422706632912 ) ) ;
#31347 = CARTESIAN_POINT ( 'NONE',  ( 4.622313124798831829, 119.7648137178985763, -11.61527771782809282 ) ) ;
#31348 = CARTESIAN_POINT ( 'NONE',  ( 10.31873187879410381, 3.604726614523240613, -0.2343749993854903346 ) ) ;
#31349 = CARTESIAN_POINT ( 'NONE',  ( 30.80910648460565682, 7.209453229046475009, 162.1186001624066932 ) ) ;
#31350 = LINE ( 'NONE', #16771, #24440 ) ;
#31351 = CARTESIAN_POINT ( 'NONE',  ( -1.926257025242585782E-15, 199.2968750006145342, -31.45816453501075927 ) ) ;
#31352 = ADVANCED_FACE ( 'NONE', ( #11899 ), #3178, .T. ) ;
#31353 = ORIENTED_EDGE ( 'NONE', *, *, #35141, .T. ) ;
#31354 = ORIENTED_EDGE ( 'NONE', *, *, #13538, .F. ) ;
#31355 = ORIENTED_EDGE ( 'NONE', *, *, #14775, .F. ) ;
#31356 = CARTESIAN_POINT ( 'NONE',  ( 23.99999999999999645, 5.196152422706631135, -5.943749998770952558 ) ) ;
#31357 = CARTESIAN_POINT ( 'NONE',  ( 20.99999999999999645, -6.646953231504538984, -3.628124999385488714 ) ) ;
#31358 = CARTESIAN_POINT ( 'NONE',  ( 15.00000000000000000, 0.000000000000000000, -6.299999999999999822 ) ) ;
#31359 =( BOUNDED_CURVE ( )  B_SPLINE_CURVE ( 2, ( #28351, #36320, #21755, #25143, #19665, #19105, #22128 ),
 .UNSPECIFIED., .F., .F. ) 
 B_SPLINE_CURVE_WITH_KNOTS ( ( 3, 2, 2, 3 ),
 ( 0.7173913043478249429, 0.7246376811594192890, 0.7318840579710137462, 0.7391304347826079812 ),
 .UNSPECIFIED. ) 
 CURVE ( )  GEOMETRIC_REPRESENTATION_ITEM ( )  RATIONAL_B_SPLINE_CURVE ( ( 1.000000000000020428, 0.8660254037844181685, 1.000000000000000000, 0.8660254037844387076, 1.000000000000000000, 0.8660254037844510311, 0.9999999999999876765 ) ) 
 REPRESENTATION_ITEM ( '' )  );
#31360 = CARTESIAN_POINT ( 'NONE',  ( 31.39005398230441912, -6.928203230275514990, 168.7588604462623039 ) ) ;
#31361 = CARTESIAN_POINT ( 'NONE',  ( 21.00000000000000000, 248.7343750006145342, -6.646953231504538984 ) ) ;
#31362 = CARTESIAN_POINT ( 'NONE',  ( -2.311890736173176641, 51.52268628210145351, -12.53471296425194836 ) ) ;
#31363 = CARTESIAN_POINT ( 'NONE',  ( -62.06919563604516554, 216.5000000000000000, -0.1155267958017906493 ) ) ;
#31364 = CARTESIAN_POINT ( 'NONE',  ( 14.43174379454686829, 216.5682562054522009, -0.6968546016497452200 ) ) ;
#31365 = CIRCLE ( 'NONE', #7785, 2.649999999999985700 ) ;
#31366 = CARTESIAN_POINT ( 'NONE',  ( -40.10044563604517265, 206.6211998817775566, -3.209657149897419348 ) ) ;
#31367 = FILL_AREA_STYLE ('',( #31550 ) ) ;
#31368 = CARTESIAN_POINT ( 'NONE',  ( 28.08117253353866971, 5.196152422706630247, 165.3593121602424674 ) ) ;
#31369 = CARTESIAN_POINT ( 'NONE',  ( -4.944772684328424539, 100.2148137178985650, -11.48171059495408031 ) ) ;
#31370 = CARTESIAN_POINT ( 'NONE',  ( -37.33705436395490551, 205.3262412349647263, -4.842901733360204020 ) ) ;
#31371 = CARTESIAN_POINT ( 'NONE',  ( -48.22247103062156981, 205.6499508600178956, 7.303452534266880569 ) ) ;
#31372 = EDGE_CURVE ( 'NONE', #17676, #17383, #32179, .T. ) ;
#31373 = CONTEXT_DEPENDENT_SHAPE_REPRESENTATION ( #5216, #37075 ) ;
#31374 = CARTESIAN_POINT ( 'NONE',  ( 26.75643035624999655, 7.049594010296217766E-16, -4.078124999385480010 ) ) ;
#31375 = CARTESIAN_POINT ( 'NONE',  ( -54.50000000000000711, 244.5000000000000000, -5.000000000000000000 ) ) ;
#31376 = AXIS2_PLACEMENT_3D ( 'NONE', #13172, #23665, #11907 ) ;
#31377 = CARTESIAN_POINT ( 'NONE',  ( 2.908627838312458636, 101.0773137178985479, -15.53471296425188442 ) ) ;
#31378 = CARTESIAN_POINT ( 'NONE',  ( -37.92336230271182984, 215.6869285224997270, 3.149950860017831200 ) ) ;
#31379 = ORIENTED_EDGE ( 'NONE', *, *, #20765, .T. ) ;
#31380 = CARTESIAN_POINT ( 'NONE',  ( 20.99999999999999289, 242.2937500012290570, -5.999999999999997335 ) ) ;
#31381 = CARTESIAN_POINT ( 'NONE',  ( -10.69584247140444866, 131.4476862821014436, 6.932735513423972762 ) ) ;
#31382 = CARTESIAN_POINT ( 'NONE',  ( -0.1745138560725817967, 65.61018628210146630, 15.50000000000000533 ) ) ;
#31383 = EDGE_CURVE ( 'NONE', #11836, #6657, #2531, .T. ) ;
#31384 = CARTESIAN_POINT ( 'NONE',  ( 15.02283181144952628, 7.347880794884122694E-16, 50.52293445648592751 ) ) ;
#31385 = CARTESIAN_POINT ( 'NONE',  ( 27.69756682629397915, 5.407089921784862696, 162.3720029866663594 ) ) ;
#31386 = CARTESIAN_POINT ( 'NONE',  ( 6.092822981423978490, 61.58518628210146062, -14.25334919248782306 ) ) ;
#31387 = CARTESIAN_POINT ( 'NONE',  ( 19.68408634441910721, 5.407089921784857367, -6.140624999385558169 ) ) ;
#31388 = CARTESIAN_POINT ( 'NONE',  ( 9.500000000000005329, 26.51018628210144001, 0.1745138560725188748 ) ) ;
#31389 = DIRECTION ( 'NONE',  ( 0.000000000000000000, 0.000000000000000000, 1.000000000000000000 ) ) ;
#31390 = CARTESIAN_POINT ( 'NONE',  ( -63.26413769728824121, 213.1499508600178672, 5.686928522499718142 ) ) ;
#31391 = FILL_AREA_STYLE ('',( #34047 ) ) ;
#31392 = CARTESIAN_POINT ( 'NONE',  ( 11.61527771782819940, 53.53518628210144925, -4.622313124798573369 ) ) ;
#31393 = CARTESIAN_POINT ( 'NONE',  ( -27.00000000000000355, 198.1625000000000227, -15.58845726811989429 ) ) ;
#31394 = VECTOR ( 'NONE', #27049, 1000.000000000000000 ) ;
#31395 = CARTESIAN_POINT ( 'NONE',  ( -69.00000000000002842, 215.5000000000000000, 6.735557395310435121E-16 ) ) ;
#31397 = CARTESIAN_POINT ( 'NONE',  ( 13.44051670066911086, -5.407089921784865361, -2.821874999385520777 ) ) ;
#31396 = CARTESIAN_POINT ( 'NONE',  ( 6.840914352312096547, 25.36018628210144854, -6.594114490232313663 ) ) ;
#31398 = CARTESIAN_POINT ( 'NONE',  ( 23.87821517812499650, 248.8093750006145228, -4.985214923628404904 ) ) ;
#31399 = EDGE_LOOP ( 'NONE', ( #34166, #23364, #36340, #8928 ) ) ;
#31400 = CARTESIAN_POINT ( 'NONE',  ( 26.99999999999999645, -3.464101615137751278, -5.212499999999995914 ) ) ;
#31401 = CARTESIAN_POINT ( 'NONE',  ( 14.99999999999999289, 204.0000000000000000, 0.000000000000000000 ) ) ;
#31402 = CARTESIAN_POINT ( 'NONE',  ( 24.40136593803570975, -3.604726614523244610, 160.5147182943441067 ) ) ;
#31403 = CARTESIAN_POINT ( 'NONE',  ( 22.80587116629410716, 3.604726614523238837, -2.578124999385541738 ) ) ;
#31404 = CARTESIAN_POINT ( 'NONE',  ( 37.56492527877403376, -3.604726614523235284, 167.7010346059732342 ) ) ;
#31405 = CARTESIAN_POINT ( 'NONE',  ( 18.00000000000000355, 244.6750000000000114, 5.196152422706632912 ) ) ;
#31406 = DIRECTION ( 'NONE',  ( 0.08715574274765150453, 0.000000000000000000, 0.9961946980917461003 ) ) ;
#31407 = CARTESIAN_POINT ( 'NONE',  ( -11.61527771782819940, 67.33518628210144641, 4.622313124798574258 ) ) ;
#31408 = ORIENTED_EDGE ( 'NONE', *, *, #20954, .T. ) ;
#31409 = ORIENTED_EDGE ( 'NONE', *, *, #20778, .T. ) ;
#31410 = CARTESIAN_POINT ( 'NONE',  ( -26.99999999999998934, 196.5500000012290229, 15.58845726811991561 ) ) ;
#31411 = CARTESIAN_POINT ( 'NONE',  ( 20.99999999999999645, 243.4187500012290002, 5.999999999999998224 ) ) ;
#31412 = ADVANCED_FACE ( 'NONE', ( #7351 ), #6778, .F. ) ;
#31413 = CARTESIAN_POINT ( 'NONE',  ( 15.46528703574811736, 38.40231371789853654, -3.257655550456947768 ) ) ;
#31414 = CARTESIAN_POINT ( 'NONE',  ( 15.24356964374999990, 0.000000000000000000, -8.803124999385486760 ) ) ;
#31415 = CARTESIAN_POINT ( 'NONE',  ( 21.00000000000000000, 242.5468750006145342, -6.646953231504538984 ) ) ;
#31416 = CARTESIAN_POINT ( 'NONE',  ( -47.23288769728824121, 205.5309553116392465, -1.321298161741839117 ) ) ;
#31417 = CYLINDRICAL_SURFACE ( 'NONE', #17994, 5.999999999999998224 ) ;
#31418 = CARTESIAN_POINT ( 'NONE',  ( 27.73678691053042300, 5.407089921784862696, 162.8202906008076241 ) ) ;
#31419 = CARTESIAN_POINT ( 'NONE',  ( 6.840914352311949109, 30.63981371789855146, 6.594114490232462877 ) ) ;
#31420 = ADVANCED_FACE ( 'NONE', ( #6982, #9626 ), #36325, .F. ) ;
#31421 = CARTESIAN_POINT ( 'NONE',  ( -68.40997103062156270, 215.5714017266979852, 3.350049139982118618 ) ) ;
#31422 = CARTESIAN_POINT ( 'NONE',  ( 22.69185864259442198, 195.0000000000000284, -14.73983514314510401 ) ) ;
#31423 = CARTESIAN_POINT ( 'NONE',  ( 27.24356964375000700, 197.3468750006145740, 15.72908226750537075 ) ) ;
#31424 = CARTESIAN_POINT ( 'NONE',  ( -2.311890736173448424, 13.67731371789854400, 12.53471296425189330 ) ) ;
#31425 = ADVANCED_FACE ( 'NONE', ( #18353 ), #15506, .F. ) ;
#31426 = CARTESIAN_POINT ( 'NONE',  ( 8.715434833791931624, 64.46018628210146062, 8.962234695871760692 ) ) ;
#31427 = CARTESIAN_POINT ( 'NONE',  ( 15.00000000000000178, 240.5875000000000057, 3.464101615137757051 ) ) ;
#31428 = FACE_OUTER_BOUND ( 'NONE', #20144, .T. ) ;
#31429 = CARTESIAN_POINT ( 'NONE',  ( 37.63846293671737442, -3.604726614523238837, 168.5415738824881373 ) ) ;
#31430 = CARTESIAN_POINT ( 'NONE',  ( 21.00000000000000000, -6.928203230275506996, -0.7312499987709595306 ) ) ;
#31431 = CARTESIAN_POINT ( 'NONE',  ( 13.44051670066911441, -5.407089921784865361, -9.571874999385554972 ) ) ;
#31432 = CARTESIAN_POINT ( 'NONE',  ( 26.99999999999999645, 197.2250000012290343, -15.58845726811990495 ) ) ;
#31433 = CARTESIAN_POINT ( 'NONE',  ( 5.233372021372432847, 83.14768628210143220, 8.152565276336710909 ) ) ;
#31434 = CARTESIAN_POINT ( 'NONE',  ( 19.39230484541326049, 249.4575961894323655, -5.999999999999997335 ) ) ;
#31435 = CARTESIAN_POINT ( 'NONE',  ( 10.49813415415989581, 110.1726862821014521, 7.228626920339068285 ) ) ;
#31436 = LINE ( 'NONE', #17040, #13650 ) ;
#31437 = CARTESIAN_POINT ( 'NONE',  ( 16.56230152254410726, 6.928203230275506996, -3.599999998771000520 ) ) ;
#31438 = EDGE_LOOP ( 'NONE', ( #13695, #19856, #9127, #29386, #14836 ) ) ;
#31439 = CARTESIAN_POINT ( 'NONE',  ( 24.56314878551104286, -3.604726614523240613, 162.3639047026769049 ) ) ;
#31440 = CARTESIAN_POINT ( 'NONE',  ( 21.00000000000000000, 6.646953231504538984, -8.803124999385454785 ) ) ;
#31441 = CARTESIAN_POINT ( 'NONE',  ( -13.62178482187500528, 195.2843750006145456, -23.59362340125807123 ) ) ;
#31442 = CARTESIAN_POINT ( 'NONE',  ( 31.37289519550453321, -7.209453229046482114, 168.5627346156876740 ) ) ;
#31443 = CARTESIAN_POINT ( 'NONE',  ( 34.18580599575048495, -5.196152422706635576, 166.2933124484913492 ) ) ;
#31444 = CARTESIAN_POINT ( 'NONE',  ( 16.56230152254411081, 6.928203230275514990, -9.112500000000034461 ) ) ;
#31445 = CARTESIAN_POINT ( 'NONE',  ( 26.75643035624999655, 241.5718750006145115, -3.323476615752271712 ) ) ;
#31446 = CARTESIAN_POINT ( 'NONE',  ( -27.24356964375000345, 197.5531250006145285, 0.000000000000000000 ) ) ;
#31447 = CARTESIAN_POINT ( 'NONE',  ( -7.228626920338836470, 118.3273137178985621, -10.49813415416005213 ) ) ;
#31448 = CARTESIAN_POINT ( 'NONE',  ( -12.53471296425194659, 132.0226862821014606, 2.311890736173176641 ) ) ;
#31450 = EDGE_LOOP ( 'NONE', ( #32460, #9682 ) ) ;
#31449 = VERTEX_POINT ( 'NONE', #9995 ) ;
#31451 = CARTESIAN_POINT ( 'NONE',  ( 18.12178482187499640, 241.5718750006145399, -4.985214923628404904 ) ) ;
#31452 = FACE_OUTER_BOUND ( 'NONE', #22373, .T. ) ;
#31453 = EDGE_CURVE ( 'NONE', #3975, #25890, #15696, .T. ) ;
#31454 = CARTESIAN_POINT ( 'NONE',  ( -8.927990412390371944, 99.92731371789854222, -13.04141134922778988 ) ) ;
#31455 = CARTESIAN_POINT ( 'NONE',  ( -2.660918448318275509, 93.49768628210145494, 12.46528703574805874 ) ) ;
#31456 = CARTESIAN_POINT ( 'NONE',  ( 15.24356964375000167, -3.323476615752272600, -1.565624999385462957 ) ) ;
#31457 = CARTESIAN_POINT ( 'NONE',  ( -26.99999999999998934, 198.3500000012290627, 15.58845726811991561 ) ) ;
#31458 = CARTESIAN_POINT ( 'NONE',  ( 12.53471296425194836, 118.2226862821014635, -2.311890736173178418 ) ) ;
#31459 = CARTESIAN_POINT ( 'NONE',  ( 16.56230152254410370, -7.209453229046475009, -4.078124999385484450 ) ) ;
#31460 = CARTESIAN_POINT ( 'NONE',  ( 26.75643035624999655, 245.0218750006145001, -7.049594010296217766E-16 ) ) ;
#31461 = CARTESIAN_POINT ( 'NONE',  ( 0.000000000000000000, 148.0000000000000000, 0.000000000000000000 ) ) ;
#31462 = AXIS2_PLACEMENT_3D ( 'NONE', #802, #4028, #15415 ) ;
#31463 = CARTESIAN_POINT ( 'NONE',  ( -55.14211230271182274, 203.5309553116391612, 1.857196546604092280 ) ) ;
#31464 = CARTESIAN_POINT ( 'NONE',  ( -6.932735513423968321, 115.3476862821014635, -10.69584247140445221 ) ) ;
#31465 = CARTESIAN_POINT ( 'NONE',  ( 22.56230152254410015, 7.347880794884117764E-16, -2.812499998771006204 ) ) ;
#31466 = CARTESIAN_POINT ( 'NONE',  ( -50.00372103062157692, 216.5309553116391612, -1.626142955000564383 ) ) ;
#31467 = FACE_OUTER_BOUND ( 'NONE', #24423, .T. ) ;
#31468 = CARTESIAN_POINT ( 'NONE',  ( 20.99999999999995026, 240.9437500012290911, -5.999999999999998224 ) ) ;
#31469 = CARTESIAN_POINT ( 'NONE',  ( -3.257655550457281723, 102.6976862821014294, 15.46528703574804986 ) ) ;
#31470 = CARTESIAN_POINT ( 'NONE',  ( 4.622313124798573369, 9.835186282101449962, 11.61527771782819940 ) ) ;
#31471 = CARTESIAN_POINT ( 'NONE',  ( 33.92433876750752830, 5.196152422706637353, 163.3047283542161381 ) ) ;
#31472 = CARTESIAN_POINT ( 'NONE',  ( 22.56230152254411792, 7.347880794884125653E-16, -2.475000000000060485 ) ) ;
#31473 = CARTESIAN_POINT ( 'NONE',  ( 0.1745138560725194299, 134.6101862821014947, -9.500000000000005329 ) ) ;
#31474 = CARTESIAN_POINT ( 'NONE',  ( 22.80587116629410716, -3.604726614523235284, -2.203124999385539962 ) ) ;
#31476 = ORIENTED_EDGE ( 'NONE', *, *, #10112, .T. ) ;
#31475 = CIRCLE ( 'NONE', #32066, 7.500000000000000000 ) ;
#31477 = CARTESIAN_POINT ( 'NONE',  ( 37.60741370336351252, 7.646167579472015790E-16, 168.1866795212929446 ) ) ;
#31478 = CARTESIAN_POINT ( 'NONE',  ( 1.715153634034233487, 56.12268628210142651, 9.534712964251941258 ) ) ;
#31479 = CARTESIAN_POINT ( 'NONE',  ( 15.24356964374999990, 3.323476615752268604, -1.078124999385470462 ) ) ;
#31480 = CARTESIAN_POINT ( 'NONE',  ( 18.00000000000000000, 5.196152422706630247, -5.025000000000002132 ) ) ;
#31481 = CARTESIAN_POINT ( 'NONE',  ( -56.70466238434234185, 244.2363183625454894, -2.499999999999996447 ) ) ;
#31482 = CARTESIAN_POINT ( 'NONE',  ( -27.24356964374999635, 195.3968750006145569, 15.72908226750539384 ) ) ;
#31483 = EDGE_CURVE ( 'NONE', #5552, #23197, #17825, .T. ) ;
#31484 = CARTESIAN_POINT ( 'NONE',  ( 26.99999999999999645, 246.2124999999999773, -3.464101615137755275 ) ) ;
#31485 = LINE ( 'NONE', #22966, #3021 ) ;
#31486 = CARTESIAN_POINT ( 'NONE',  ( -5.529263428287297444, 44.72731371789853938, -7.954856959092311719 ) ) ;
#31487 = CARTESIAN_POINT ( 'NONE',  ( 26.99999999999999645, 3.464101615137755275, -9.187499999999994671 ) ) ;
#31488 = VERTEX_POINT ( 'NONE', #15314 ) ;
#31489 = CARTESIAN_POINT ( 'NONE',  ( 26.75643035624999655, 249.0343750006145456, 3.323476615752267715 ) ) ;
#31490 = AXIS2_PLACEMENT_3D ( 'NONE', #759, #9491, #23710 ) ;
#31491 = CARTESIAN_POINT ( 'NONE',  ( -12.53471296425189152, 61.97731371789855359, -2.311890736173453309 ) ) ;
#31492 = CARTESIAN_POINT ( 'NONE',  ( 22.80587116629411071, 3.604726614523243278, -9.384374999385521221 ) ) ;
#31493 = CARTESIAN_POINT ( 'NONE',  ( 15.24356964374999990, 3.323476615752268604, -0.1781249993854788494 ) ) ;
#31494 = CARTESIAN_POINT ( 'NONE',  ( 7.228626920338837358, 12.52731371789855785, 10.49813415416005036 ) ) ;
#31495 = ADVANCED_FACE ( 'NONE', ( #1652 ), #24775, .T. ) ;
#31496 = EDGE_LOOP ( 'NONE', ( #33909, #18318, #4452, #28684 ) ) ;
#31497 = PRODUCT_DEFINITION ( 'UNKNOWN', '', #25071, #17984 ) ;
#31498 = CARTESIAN_POINT ( 'NONE',  ( -12.46528703574805697, 3.797686282101447652, -2.660918448318280838 ) ) ;
#31499 = CARTESIAN_POINT ( 'NONE',  ( 37.33123894353190764, 3.604726614523243278, 165.0299875717147415 ) ) ;
#31500 = CARTESIAN_POINT ( 'NONE',  ( -45.64211230271183695, 203.5309553116391612, 1.857196546604092280 ) ) ;
#31501 = CARTESIAN_POINT ( 'NONE',  ( 24.73633934067528983, 0.000000000000000000, 161.5488335588110544 ) ) ;
#31502 =( NAMED_UNIT ( * ) PLANE_ANGLE_UNIT ( ) SI_UNIT ( $, .RADIAN. ) );
#31503 = CARTESIAN_POINT ( 'NONE',  ( -23.43450404749491156, 195.0000000000001137, -13.63327128574096037 ) ) ;
#31504 = CARTESIAN_POINT ( 'NONE',  ( -37.33705436395491262, 206.7903428501026042, -3.378800118222489157 ) ) ;
#31505 = CARTESIAN_POINT ( 'NONE',  ( -48.61830436395490551, 209.8844732041982581, 6.500000000000000888 ) ) ;
#31506 = CARTESIAN_POINT ( 'NONE',  ( 25.11222996482124259, -3.604726614523240613, 168.6399313006548653 ) ) ;
#31507 = EDGE_LOOP ( 'NONE', ( #36308, #34752, #624, #1702 ) ) ;
#31508 = CARTESIAN_POINT ( 'NONE',  ( -28.78272864601244763, 202.8264516967929865, 3.550837175518763544 ) ) ;
#31509 = CARTESIAN_POINT ( 'NONE',  ( 8.927990412390371944, 12.52731371789855963, 13.04141134922778811 ) ) ;
#31510 = CARTESIAN_POINT ( 'NONE',  ( -37.52752896937849414, 214.3500491399821897, 7.303452534266821949 ) ) ;
#31511 = CARTESIAN_POINT ( 'NONE',  ( 8.962234695871762469, 16.16018628210144570, -8.715434833791931624 ) ) ;
#31512 =( BOUNDED_CURVE ( )  B_SPLINE_CURVE ( 2, ( #23246, #35538, #9020, #9583, #35158, #20779, #32695 ),
 .UNSPECIFIED., .F., .F. ) 
 B_SPLINE_CURVE_WITH_KNOTS ( ( 3, 2, 2, 3 ),
 ( 0.6086956521739130821, 0.6159420289855073172, 0.6231884057971016633, 0.6304347826086960094 ),
 .UNSPECIFIED. ) 
 CURVE ( )  GEOMETRIC_REPRESENTATION_ITEM ( )  RATIONAL_B_SPLINE_CURVE ( ( 1.000000000000000000, 0.8660254037844387076, 1.000000000000000000, 0.8660254037844387076, 1.000000000000000000, 0.8660254037844326014, 1.000000000000006217 ) ) 
 REPRESENTATION_ITEM ( '' )  );
#31513 = CARTESIAN_POINT ( 'NONE',  ( -12.50000000000000355, 49.51018628210145067, -0.1745138560725492671 ) ) ;
#31514 = CARTESIAN_POINT ( 'NONE',  ( 22.56230152254412502, 7.347880794884125653E-16, -3.375000000000044409 ) ) ;
#31515 = VERTEX_POINT ( 'NONE', #30475 ) ;
#31516 = CARTESIAN_POINT ( 'NONE',  ( 6.092822981423978490, 15.58518628210145351, -14.25334919248782306 ) ) ;
#31517 = CARTESIAN_POINT ( 'NONE',  ( -27.24356964374999279, 195.3406250006145228, 15.72908226750539384 ) ) ;
#31518 = CARTESIAN_POINT ( 'NONE',  ( -27.24356964374999635, 196.2968750006145342, 15.72908226750539384 ) ) ;
#31519 = DIRECTION ( 'NONE',  ( 0.000000000000000000, -0.000000000000000000, 1.000000000000000000 ) ) ;
#31520 = CARTESIAN_POINT ( 'NONE',  ( 20.99999999999999645, 6.928203230275506996, -4.106249998770976184 ) ) ;
#31521 = DIRECTION ( 'NONE',  ( 0.000000000000000000, 0.000000000000000000, 1.000000000000000000 ) ) ;
#31522 = CARTESIAN_POINT ( 'NONE',  ( 25.33771396574129042, -3.464101615137802348, 168.4225769768684131 ) ) ;
#31523 = CARTESIAN_POINT ( 'NONE',  ( 26.75643035624999655, 244.6468750006145285, 3.323476615752267715 ) ) ;
#31524 = CARTESIAN_POINT ( 'NONE',  ( 6.594114490232462877, 101.9398137178985735, -6.840914352311949109 ) ) ;
#31525 = CARTESIAN_POINT ( 'NONE',  ( 26.75643035624999655, 242.8843750006145115, -7.049594010296217766E-16 ) ) ;
#31526 = CIRCLE ( 'NONE', #34554, 24.80000000000000426 ) ;
#31527 = VERTEX_POINT ( 'NONE', #18551 ) ;
#31528 = CARTESIAN_POINT ( 'NONE',  ( -63.46205436395489841, 214.6737587650352168, 4.842901733360204908 ) ) ;
#31529 = CARTESIAN_POINT ( 'NONE',  ( 25.17756528844239483, 0.000000000000000000, 166.5920692191248804 ) ) ;
#31530 = CARTESIAN_POINT ( 'NONE',  ( 21.00000000000000000, 249.4937500012290741, -6.928203230275506996 ) ) ;
#31531 = ORIENTED_EDGE ( 'NONE', *, *, #17031, .F. ) ;
#31532 = CARTESIAN_POINT ( 'NONE',  ( 10.49813415416005213, 111.4273137178985564, -7.228626920338837358 ) ) ;
#31533 = CARTESIAN_POINT ( 'NONE',  ( 16.56230152254411436, 7.209453229046482114, -1.209374999385475657 ) ) ;
#31534 = CARTESIAN_POINT ( 'NONE',  ( 36.94067227134398479, 7.646167579472015790E-16, 160.5657900808910767 ) ) ;
#31535 = CARTESIAN_POINT ( 'NONE',  ( 23.87821517812500005, -4.985214923628404016, -1.003124999385485161 ) ) ;
#31536 = CARTESIAN_POINT ( 'NONE',  ( 27.24356964375000700, 199.5968750006145456, 15.72908226750537075 ) ) ;
#31537 = ORIENTED_EDGE ( 'NONE', *, *, #32431, .F. ) ;
#31538 = EDGE_LOOP ( 'NONE', ( #27994, #31114, #18041, #14529 ) ) ;
#31539 =( BOUNDED_CURVE ( )  B_SPLINE_CURVE ( 2, ( #2511, #20337, #11044, #17489, #22620, #11420, #3067, #5720, #17301 ),
 .UNSPECIFIED., .F., .F. ) 
 B_SPLINE_CURVE_WITH_KNOTS ( ( 3, 2, 2, 2, 3 ),
 ( 0.3125000000000000000, 0.3194444444444444198, 0.3333333333333333148, 0.3472222222222222099, 0.3541666666666666852 ),
 .UNSPECIFIED. ) 
 CURVE ( )  GEOMETRIC_REPRESENTATION_ITEM ( )  RATIONAL_B_SPLINE_CURVE ( ( 0.9330127018922194093, 0.9330127018922194093, 1.000000000000000000, 0.8660254037844387076, 1.000000000000000000, 0.8660254037844387076, 1.000000000000000000, 0.9330127018922190762, 0.9330127018922194093 ) ) 
 REPRESENTATION_ITEM ( '' )  );
#31540 = VERTEX_POINT ( 'NONE', #15885 ) ;
#31541 = CARTESIAN_POINT ( 'NONE',  ( 26.99999999999999645, -3.464101615137751278, -7.406249998770965348 ) ) ;
#31542 = CARTESIAN_POINT ( 'NONE',  ( 15.24356964374999990, 0.000000000000000000, -2.840624999385477079 ) ) ;
#31543 = CARTESIAN_POINT ( 'NONE',  ( 36.56321044411491528, 7.347880794884117764E-16, 159.0460299011043901 ) ) ;
#31544 = CARTESIAN_POINT ( 'NONE',  ( 15.24356964374999990, 248.3968750006145285, 0.000000000000000000 ) ) ;
#31545 = CARTESIAN_POINT ( 'NONE',  ( -11.48171059495397373, 50.08518628210144641, -4.944772684328680334 ) ) ;
#31546 = CARTESIAN_POINT ( 'NONE',  ( -56.32961230271183695, 211.8571965466040581, 6.469044688360755302 ) ) ;
#31547 = EDGE_CURVE ( 'NONE', #26761, #12005, #6592, .T. ) ;
#31548 = CARTESIAN_POINT ( 'NONE',  ( 14.06021656787535434, 216.9397834321072480, -0.8200469388708427898 ) ) ;
#31549 = CARTESIAN_POINT ( 'NONE',  ( -47.62127896937850124, 214.5309553116392749, 1.090244570138288127 ) ) ;
#31550 = FILL_AREA_STYLE_COLOUR ( '', #24414 ) ;
#31551 = CARTESIAN_POINT ( 'NONE',  ( 25.06317337608610174, -3.464101615137757051, 165.2845636778794471 ) ) ;
#31552 = CARTESIAN_POINT ( 'NONE',  ( -4.944772684328424539, 109.4148137178985536, -11.48171059495408031 ) ) ;
#31553 = CARTESIAN_POINT ( 'NONE',  ( -38.72247103062156981, 206.6499508600178672, 5.571401726697986057 ) ) ;
#31554 = CARTESIAN_POINT ( 'NONE',  ( -50.00372103062156981, 218.5309553116391896, -2.162041339862839084 ) ) ;
#31555 = CARTESIAN_POINT ( 'NONE',  ( 15.24356964375000167, -3.323476615752272600, -3.815624999385473615 ) ) ;
#31556 = LINE ( 'NONE', #31375, #27693 ) ;
#31557 = CARTESIAN_POINT ( 'NONE',  ( 14.38691631536194393, 85.26481371789857633, 5.770363421894124656 ) ) ;
#31558 = CARTESIAN_POINT ( 'NONE',  ( -31.98586230271182984, 206.8500491399821328, 5.686928522499748340 ) ) ;
#31559 = ORIENTED_EDGE ( 'NONE', *, *, #19562, .F. ) ;
#31560 = CARTESIAN_POINT ( 'NONE',  ( 26.99999999999999645, 248.9312500012290457, -7.347880794884117764E-16 ) ) ;
#31561 = CARTESIAN_POINT ( 'NONE',  ( -12.50000000000000355, 95.51018628210144357, -0.1745138560725492671 ) ) ;
#31562 = EDGE_CURVE ( 'NONE', #2980, #26922, #7641, .T. ) ;
#31563 = CARTESIAN_POINT ( 'NONE',  ( 8.632099005475504683, 64.74768628210144072, 13.23911966647218996 ) ) ;
#31564 = CARTESIAN_POINT ( 'NONE',  ( 10.56230152254612520, 3.464101615138916568, -9.824999998771035692 ) ) ;
#31565 = CARTESIAN_POINT ( 'NONE',  ( 27.71064018770612947, -5.407089921784865361, 162.5214321913800859 ) ) ;
#31566 = EDGE_CURVE ( 'NONE', #18034, #10170, #24036, .T. ) ;
#31567 = CARTESIAN_POINT ( 'NONE',  ( -13.04141134922759804, 59.57268628210145067, -8.927990412390657937 ) ) ;
#31568 = CARTESIAN_POINT ( 'NONE',  ( 10.31873187879411091, 3.604726614523236616, -5.578124999385555505 ) ) ;
#31569 = CARTESIAN_POINT ( 'NONE',  ( 16.56230152254410726, 0.000000000000000000, -10.00000000000000000 ) ) ;
#31570 = CARTESIAN_POINT ( 'NONE',  ( -68.01413769728823411, 213.1499508600178672, 5.686928522499718142 ) ) ;
#31571 = CARTESIAN_POINT ( 'NONE',  ( 15.00000000000000178, 243.3437500012290400, 3.464101615137757051 ) ) ;
#31572 = CARTESIAN_POINT ( 'NONE',  ( 12.53471296425194836, 44.62268628210144783, -2.311890736173178418 ) ) ;
#31573 = CARTESIAN_POINT ( 'NONE',  ( -13.50000000000000533, 197.6750000000000114, -23.38268590217984411 ) ) ;
#31574 = CARTESIAN_POINT ( 'NONE',  ( 15.00000000000000178, 240.1375000000000171, 3.464101615137757051 ) ) ;
#31575 = CARTESIAN_POINT ( 'NONE',  ( -2.064181346179269738, 29.09768628210144925, 9.465287035748067623 ) ) ;
#31576 = CARTESIAN_POINT ( 'NONE',  ( 26.75643035624999655, 249.2218750006145171, -3.323476615752271268 ) ) ;
#31577 = ORIENTED_EDGE ( 'NONE', *, *, #31954, .F. ) ;
#31578 = CARTESIAN_POINT ( 'NONE',  ( 24.00000000000000000, -5.196152422706629359, -4.349999999999992539 ) ) ;
#31579 =( BOUNDED_SURFACE ( )  B_SPLINE_SURFACE ( 1, 2, ( 
 ( #17675, #2691, #23544, #2874, #11229, #23354, #11786, #29212, #3253, #14448, #14267, #14827, #28470, #8574, #35089, #20523, #14080, #8394, #34535, #37365, #11417, #32248, #9139, #25818, #5907, #20705, #16928, #26184, #31877, #20143, #32, #31689, #11597, #37186, #5718, #31506, #23172, #17299, #8761, #34906, #19963, #20335, #17487, #29020, #3065, #32063, #4006, #35656, #21089, #33007, #7057, #18434, #35465, #15202, #15580, #6288, #12733, #20896, #32438, #782, #21646, #1350, #6482, #32815, #36031, #10075, #27134, #21279, #12351, #3816, #18054, #29785, #12922, #26751, #29596, #971, #9516, #23924, #1161, #15009, #18628, #9702, #32629, #6858, #3633, #24300, #29975, #6666, #30168, #4195, #35843, #18241, #15393, #9885, #17864, #21467, #26941, #12547, #15772, #27322, #23732, #24113, #24485, #29409, #3440, #26561, #589, #12158, #35271, #9326, #9997, #1120, #15158, #930, #35235, #9659, #24442, #9472, #12504, #4338, #7202, #21607, #23883, #24068, #18386, #27277, #9285, #32585, #6438, #21047, #3964, #18774, #15348, #35614, #6811, #21236, #29936, #3774, #15727, #20859, #27096, #15538, #12686, #18201, #12116, #6625, #29741, #24258, #26902, #35801, #30125, #33156, #32775, #30314, #9844, #32398, #12309, #21422, #3594, #32963, #7014, #18583, #1306, #18011, #26707, #738, #12874, #4157, #35991, #10026, #15918, #550, #35422, #23689, #29555, #13633, #2240, #13068, #36546, #36172, #27837, #30693, #13819, #21792, #34082, #4529, #8133, #27656, #7382, #1493, #7752, #10961, #25183, #10218, #24806, #36913, #19703, #19334, #10406, #31243, #16664, #5272, #13257, #33345, #2056, #27467, #33526, #10588, #1868, #30509, #18954, #36358, #28023, #16105, #13438, #24624, #22167, #25366, #21980, #24988, #1682, #7568, #22535, #19143, #33711, #30873, #28210, #4710, #16290, #4896, #16477, #36736, #10775, #22349, #33898, #7940, #19516, #31062, #5086, #31984, #13999, #5828, #34634, #20251, #34455, #28389, #11338, #25738, #17407, #37290, #2985, #8864, #11889, #22909, #35011, #31791, #11152, #28571, #2798, #19887, #28948, #8497, #14554, #6012, #22725, #5450, #17033, #17596, #28759, #20065, #26107 ),
 ( #25926, #25551, #17221, #31610, #3169, #34271, #23457, #31429, #9054, #20625, #29127, #11520, #37103, #8680, #37469, #5636, #8316, #32167, #23090, #140, #2610, #11703, #23278, #14186, #14370, #34821, #20441, #14742, #26289, #324, #16852, #2426, #18157, #12830, #32540, #32731, #18343, #23650, #6395, #15305, #26857, #6582, #29890, #21566, #24397, #24210, #15494, #12075, #3552, #26475, #29698, #15114, #3921, #20814, #6768, #23837, #35944, #4113, #886, #3732, #3359, #27050, #6971, #12458, #18539, #508, #12646, #1076, #35193, #24027, #35572, #17968, #9617, #29320, #9241, #29511, #35378, #35756, #32356, #9428, #26665, #14929, #695, #21192, #6205, #12267, #21379, #17777, #30078, #21006, #15685, #9800, #32917, #27236, #1260, #9985, #33111, #16620, #22122, #21749, #36501, #7340, #13395, #1642, #22305, #33300, #5040, #7525, #27418, #2010, #16433, #7898, #19472, #19100, #30465, #31018, #7155, #24763, #28164, #36692, #30270, #24581, #13213, #16063, #27610, #10917, #2194, #18913, #33670, #25323, #36872, #30831, #10545, #36313, #30650, #4484, #4666, #13775, #10362, #10174, #27798, #21935, #33482, #4854, #4296, #18729, #24945, #16249, #1825, #15873, #7710, #19292, #27980, #33857, #1449, #13584, #25138, #10732, #13025, #36133, #28901, #37060, #11107, #16985, #34591, #17545, #11294, #25507, #11475, #5966, #22681, #2384, #34040, #2753, #29081, #20202, #5227, #19842, #31934, #3123, #14324, #5405, #14691, #11653, #276, #8269, #31202, #8634, #26241, #28527, #31565, #34412, #34226, #16805, #31385, #23046, #2569, #22863, #19659, #5588, #8820, #14140, #8451, #22493, #8085, #28347, #25694, #20019, #25878, #23229, #13957, #37245, #17175, #28716, #37426, #31751, #5781, #17359, #2936, #14506, #26061, #91, #34777, #20393, #838, #29652, #15255, #29462, #23411, #6348, #20762, #12406, #32307, #35523, #3873, #6917, #17918, #30028, #26808, #6154, #23598, #35327, #14881, #23979, #3497, #9567, #1024, #17728, #461, #12030, #12596, #23788, #15067, #21142, #9381, #32680, #35142, #26617, #646, #6723, #24161, #34961, #20957, #20575, #12217, #32488, #35705, #29270, #18488, #26427, #4060 ) ),
 .UNSPECIFIED., .F., .F., .F. ) 
 B_SPLINE_SURFACE_WITH_KNOTS ( ( 2, 2 ),
 ( 3, 2, 2, 2, 2, 2, 2, 2, 2, 2, 2, 2, 2, 2, 2, 2, 2, 2, 2, 2, 2, 2, 2, 2, 2, 2, 2, 2, 2, 2, 2, 2, 2, 2, 2, 2, 2, 2, 2, 2, 2, 2, 2, 2, 2, 2, 2, 2, 2, 2, 2, 2, 2, 2, 2, 2, 2, 2, 2, 2, 2, 2, 2, 2, 2, 2, 2, 2, 2, 2, 2, 2, 2, 2, 2, 2, 2, 2, 2, 2, 2, 2, 2, 2, 2, 2, 2, 2, 2, 2, 2, 2, 2, 2, 2, 2, 2, 2, 2, 2, 2, 2, 2, 2, 2, 2, 2, 2, 2, 2, 2, 2, 2, 2, 2, 2, 2, 2, 2, 2, 2, 2, 2, 2, 2, 2, 2, 2, 2, 2, 2, 2, 2, 2, 2, 3 ),
 ( 0.000000000000000000, 1.000000000000000000 ),
 ( 0.000000000000000000, 0.007246376811594202987, 0.01449275362318840597, 0.02173913043478260809, 0.02898550724637681195, 0.03623188405797101580, 0.04347826086956521618, 0.05072463768115942351, 0.05797101449275362389, 0.06521739130434782428, 0.07246376811594203160, 0.07971014492753622505, 0.08695652173913043237, 0.09420289855072463969, 0.1014492753623188470, 0.1086956521739130405, 0.1159420289855072478, 0.1231884057971014551, 0.1304347826086956486, 0.1376811594202898559, 0.1449275362318840632, 0.1521739130434782705, 0.1594202898550724501, 0.1666666666666666574, 0.1739130434782608647, 0.1811594202898550721, 0.1884057971014492794, 0.1956521739130434867, 0.2028985507246376940, 0.2101449275362318736, 0.2173913043478260809, 0.2246376811594202882, 0.2318840579710144956, 0.2391304347826087029, 0.2463768115942029102, 0.2536231884057971175, 0.2608695652173912971, 0.2681159420289855322, 0.2753623188405797118, 0.2826086956521738913, 0.2898550724637681264, 0.2971014492753623060, 0.3043478260869565410, 0.3115942028985507206, 0.3188405797101449002, 0.3260869565217391353, 0.3333333333333333148, 0.3405797101449275499, 0.3478260869565217295, 0.3550724637681159646, 0.3623188405797101441, 0.3695652173913043237, 0.3768115942028985588, 0.3840579710144927383, 0.3913043478260869734, 0.3985507246376811530, 0.4057971014492753881, 0.4130434782608695676, 0.4202898550724637472, 0.4275362318840579823, 0.4347826086956521618, 0.4420289855072463969, 0.4492753623188405765, 0.4565217391304347561, 0.4637681159420289911, 0.4710144927536231707, 0.4782608695652174058, 0.4855072463768115854, 0.4927536231884058204, 0.5000000000000000000, 0.5072463768115942351, 0.5144927536231883591, 0.5217391304347825942, 0.5289855072463768293, 0.5362318840579710644, 0.5434782608695651884, 0.5507246376811594235, 0.5579710144927536586, 0.5652173913043477826, 0.5724637681159420177, 0.5797101449275362528, 0.5869565217391304879, 0.5942028985507246119, 0.6014492753623188470, 0.6086956521739130821, 0.6159420289855072062, 0.6231884057971014412, 0.6304347826086956763, 0.6376811594202898004, 0.6449275362318840354, 0.6521739130434782705, 0.6594202898550725056, 0.6666666666666666297, 0.6739130434782608647, 0.6811594202898550998, 0.6884057971014492239, 0.6956521739130434590, 0.7028985507246376940, 0.7101449275362319291, 0.7173913043478260532, 0.7246376811594202882, 0.7318840579710145233, 0.7391304347826086474, 0.7463768115942028825, 0.7536231884057971175, 0.7608695652173913526, 0.7681159420289854767, 0.7753623188405797118, 0.7826086956521739468, 0.7898550724637680709, 0.7971014492753623060, 0.8043478260869565410, 0.8115942028985507761, 0.8188405797101449002, 0.8260869565217391353, 0.8333333333333333703, 0.8405797101449274944, 0.8478260869565217295, 0.8550724637681159646, 0.8623188405797101996, 0.8695652173913043237, 0.8768115942028985588, 0.8840579710144927938, 0.8913043478260869179, 0.8985507246376811530, 0.9057971014492753881, 0.9130434782608695121, 0.9202898550724637472, 0.9275362318840579823, 0.9347826086956522174, 0.9420289855072463414, 0.9492753623188405765, 0.9565217391304348116, 0.9637681159420289356, 0.9662082893573751274, 0.9758703722509488587 ),
 .UNSPECIFIED. ) 
 GEOMETRIC_REPRESENTATION_ITEM ( )  RATIONAL_B_SPLINE_SURFACE ( (
 ( 1.000000000000000000, 0.8660254037844387076, 1.000000000000000000, 0.8660254037844387076, 1.000000000000000000, 0.8660254037844387076, 1.000000000000000000, 0.8660254037844387076, 1.000000000000000000, 0.8660254037844387076, 1.000000000000000000, 0.8660254037844387076, 1.000000000000000000, 0.8660254037844387076, 1.000000000000000000, 0.8660254037844387076, 1.000000000000000000, 0.8660254037844387076, 1.000000000000000000, 0.8660254037844387076, 1.000000000000000000, 0.8660254037844387076, 1.000000000000000000, 0.8660254037844387076, 1.000000000000000000, 0.8660254037844387076, 1.000000000000000000, 0.8660254037844387076, 1.000000000000000000, 0.8660254037844387076, 1.000000000000000000, 0.8660254037844387076, 1.000000000000000000, 0.8660254037844387076, 1.000000000000000000, 0.8660254037844387076, 1.000000000000000000, 0.8660254037844387076, 1.000000000000000000, 0.8660254037844387076, 1.000000000000000000, 0.8660254037844387076, 1.000000000000000000, 0.8660254037844387076, 1.000000000000000000, 0.8660254037844387076, 1.000000000000000000, 0.8660254037844387076, 1.000000000000000000, 0.8660254037844387076, 1.000000000000000000, 0.8660254037844387076, 1.000000000000000000, 0.8660254037844387076, 1.000000000000000000, 0.8660254037844387076, 1.000000000000000000, 0.8660254037844387076, 1.000000000000000000, 0.8660254037844387076, 1.000000000000000000, 0.8660254037844387076, 1.000000000000000000, 0.8660254037844387076, 1.000000000000000000, 0.8660254037844387076, 1.000000000000000000, 0.8660254037844387076, 1.000000000000000000, 0.8660254037844387076, 1.000000000000000000, 0.8660254037844387076, 1.000000000000000000, 0.8660254037844387076, 1.000000000000000000, 0.8660254037844387076, 1.000000000000000000, 0.8660254037844387076, 1.000000000000000000, 0.8660254037844387076, 1.000000000000000000, 0.8660254037844387076, 1.000000000000000000, 0.8660254037844387076, 1.000000000000000000, 0.8660254037844387076, 1.000000000000000000, 0.8660254037844387076, 1.000000000000000000, 0.8660254037844387076, 1.000000000000000000, 0.8660254037844387076, 1.000000000000000000, 0.8660254037844387076, 1.000000000000000000, 0.8660254037844387076, 1.000000000000000000, 0.8660254037844387076, 1.000000000000000000, 0.8660254037844387076, 1.000000000000000000, 0.8660254037844387076, 1.000000000000000000, 0.8660254037844387076, 1.000000000000000000, 0.8660254037844387076, 1.000000000000000000, 0.8660254037844387076, 1.000000000000000000, 0.8660254037844387076, 1.000000000000000000, 0.8660254037844387076, 1.000000000000000000, 0.8660254037844387076, 1.000000000000000000, 0.8660254037844387076, 1.000000000000000000, 0.8660254037844387076, 1.000000000000000000, 0.8660254037844387076, 1.000000000000000000, 0.8660254037844387076, 1.000000000000000000, 0.8660254037844387076, 1.000000000000000000, 0.8660254037844387076, 1.000000000000000000, 0.8660254037844387076, 1.000000000000000000, 0.8660254037844387076, 1.000000000000000000, 0.8660254037844387076, 1.000000000000000000, 0.8660254037844387076, 1.000000000000000000, 0.8660254037844387076, 1.000000000000000000, 0.8660254037844387076, 1.000000000000000000, 0.8660254037844387076, 1.000000000000000000, 0.8660254037844387076, 1.000000000000000000, 0.8660254037844387076, 1.000000000000000000, 0.8660254037844387076, 1.000000000000000000, 0.8660254037844387076, 1.000000000000000000, 0.8660254037844387076, 1.000000000000000000, 0.8660254037844387076, 1.000000000000000000, 0.8660254037844387076, 1.000000000000000000, 0.8660254037844387076, 1.000000000000000000, 0.8660254037844387076, 1.000000000000000000, 0.8660254037844387076, 1.000000000000000000, 0.8660254037844387076, 1.000000000000000000, 0.8660254037844387076, 1.000000000000000000, 0.8660254037844387076, 1.000000000000000000, 0.8660254037844387076, 1.000000000000000000, 0.8660254037844387076, 1.000000000000000000, 0.8660254037844387076, 1.000000000000000000, 0.8660254037844387076, 1.000000000000000000, 0.8660254037844387076, 1.000000000000000000, 0.8660254037844387076, 1.000000000000000000, 0.8660254037844387076, 1.000000000000000000, 0.8660254037844387076, 1.000000000000000000, 0.8660254037844387076, 1.000000000000000000, 0.8660254037844387076, 1.000000000000000000, 0.8660254037844387076, 1.000000000000000000, 0.8660254037844387076, 1.000000000000000000, 0.8660254037844387076, 1.000000000000000000, 0.8660254037844387076, 1.000000000000000000, 0.8660254037844387076, 1.000000000000000000, 0.8660254037844387076, 1.000000000000000000, 0.8660254037844387076, 1.000000000000000000, 0.8660254037844387076, 1.000000000000000000, 0.8660254037844387076, 1.000000000000000000, 0.8660254037844387076, 1.000000000000000000, 0.8660254037844387076, 1.000000000000000000, 0.8660254037844387076, 1.000000000000000000, 0.8660254037844387076, 1.000000000000000000, 0.8660254037844387076, 1.000000000000000000, 0.8660254037844387076, 1.000000000000000000, 0.8660254037844387076, 1.000000000000000000, 0.8660254037844387076, 1.000000000000000000, 0.8660254037844387076, 1.000000000000000000, 0.8660254037844387076, 1.000000000000000000, 0.8660254037844387076, 1.000000000000000000, 0.8660254037844387076, 1.000000000000000000, 0.8660254037844387076, 1.000000000000000000, 0.8660254037844387076, 1.000000000000000000, 0.8660254037844387076, 1.000000000000000000, 0.8660254037844387076, 1.000000000000000000, 0.8660254037844387076, 1.000000000000000000, 0.8660254037844387076, 1.000000000000000000, 0.8660254037844387076, 1.000000000000000000, 0.8660254037844387076, 1.000000000000000000, 0.8660254037844387076, 1.000000000000000000, 0.8660254037844387076, 1.000000000000000000, 0.8660254037844387076, 1.000000000000000000, 0.8660254037844387076, 1.000000000000000000, 0.8660254037844387076, 1.000000000000000000, 0.8660254037844387076, 1.000000000000000000, 0.8660254037844387076, 1.000000000000000000, 0.8660254037844387076, 1.000000000000000000, 0.8660254037844387076, 1.000000000000000000, 0.8660254037844387076, 1.000000000000000000, 0.8660254037844387076, 1.000000000000000000, 0.9548848677736607726, 0.9401542295229587953, 0.9401542295229587953, 0.9401542295229587953),
 ( 1.000000000000000000, 0.8660254037844387076, 1.000000000000000000, 0.8660254037844387076, 1.000000000000000000, 0.8660254037844387076, 1.000000000000000000, 0.8660254037844387076, 1.000000000000000000, 0.8660254037844387076, 1.000000000000000000, 0.8660254037844387076, 1.000000000000000000, 0.8660254037844387076, 1.000000000000000000, 0.8660254037844387076, 1.000000000000000000, 0.8660254037844387076, 1.000000000000000000, 0.8660254037844387076, 1.000000000000000000, 0.8660254037844387076, 1.000000000000000000, 0.8660254037844387076, 1.000000000000000000, 0.8660254037844387076, 1.000000000000000000, 0.8660254037844387076, 1.000000000000000000, 0.8660254037844387076, 1.000000000000000000, 0.8660254037844387076, 1.000000000000000000, 0.8660254037844387076, 1.000000000000000000, 0.8660254037844387076, 1.000000000000000000, 0.8660254037844387076, 1.000000000000000000, 0.8660254037844387076, 1.000000000000000000, 0.8660254037844387076, 1.000000000000000000, 0.8660254037844387076, 1.000000000000000000, 0.8660254037844387076, 1.000000000000000000, 0.8660254037844387076, 1.000000000000000000, 0.8660254037844387076, 1.000000000000000000, 0.8660254037844387076, 1.000000000000000000, 0.8660254037844387076, 1.000000000000000000, 0.8660254037844387076, 1.000000000000000000, 0.8660254037844387076, 1.000000000000000000, 0.8660254037844387076, 1.000000000000000000, 0.8660254037844387076, 1.000000000000000000, 0.8660254037844387076, 1.000000000000000000, 0.8660254037844387076, 1.000000000000000000, 0.8660254037844387076, 1.000000000000000000, 0.8660254037844387076, 1.000000000000000000, 0.8660254037844387076, 1.000000000000000000, 0.8660254037844387076, 1.000000000000000000, 0.8660254037844387076, 1.000000000000000000, 0.8660254037844387076, 1.000000000000000000, 0.8660254037844387076, 1.000000000000000000, 0.8660254037844387076, 1.000000000000000000, 0.8660254037844387076, 1.000000000000000000, 0.8660254037844387076, 1.000000000000000000, 0.8660254037844387076, 1.000000000000000000, 0.8660254037844387076, 1.000000000000000000, 0.8660254037844387076, 1.000000000000000000, 0.8660254037844387076, 1.000000000000000000, 0.8660254037844387076, 1.000000000000000000, 0.8660254037844387076, 1.000000000000000000, 0.8660254037844387076, 1.000000000000000000, 0.8660254037844387076, 1.000000000000000000, 0.8660254037844387076, 1.000000000000000000, 0.8660254037844387076, 1.000000000000000000, 0.8660254037844387076, 1.000000000000000000, 0.8660254037844387076, 1.000000000000000000, 0.8660254037844387076, 1.000000000000000000, 0.8660254037844387076, 1.000000000000000000, 0.8660254037844387076, 1.000000000000000000, 0.8660254037844387076, 1.000000000000000000, 0.8660254037844387076, 1.000000000000000000, 0.8660254037844387076, 1.000000000000000000, 0.8660254037844387076, 1.000000000000000000, 0.8660254037844387076, 1.000000000000000000, 0.8660254037844387076, 1.000000000000000000, 0.8660254037844387076, 1.000000000000000000, 0.8660254037844387076, 1.000000000000000000, 0.8660254037844387076, 1.000000000000000000, 0.8660254037844387076, 1.000000000000000000, 0.8660254037844387076, 1.000000000000000000, 0.8660254037844387076, 1.000000000000000000, 0.8660254037844387076, 1.000000000000000000, 0.8660254037844387076, 1.000000000000000000, 0.8660254037844387076, 1.000000000000000000, 0.8660254037844387076, 1.000000000000000000, 0.8660254037844387076, 1.000000000000000000, 0.8660254037844387076, 1.000000000000000000, 0.8660254037844387076, 1.000000000000000000, 0.8660254037844387076, 1.000000000000000000, 0.8660254037844387076, 1.000000000000000000, 0.8660254037844387076, 1.000000000000000000, 0.8660254037844387076, 1.000000000000000000, 0.8660254037844387076, 1.000000000000000000, 0.8660254037844387076, 1.000000000000000000, 0.8660254037844387076, 1.000000000000000000, 0.8660254037844387076, 1.000000000000000000, 0.8660254037844387076, 1.000000000000000000, 0.8660254037844387076, 1.000000000000000000, 0.8660254037844387076, 1.000000000000000000, 0.8660254037844387076, 1.000000000000000000, 0.8660254037844387076, 1.000000000000000000, 0.8660254037844387076, 1.000000000000000000, 0.8660254037844387076, 1.000000000000000000, 0.8660254037844387076, 1.000000000000000000, 0.8660254037844387076, 1.000000000000000000, 0.8660254037844387076, 1.000000000000000000, 0.8660254037844387076, 1.000000000000000000, 0.8660254037844387076, 1.000000000000000000, 0.8660254037844387076, 1.000000000000000000, 0.8660254037844387076, 1.000000000000000000, 0.8660254037844387076, 1.000000000000000000, 0.8660254037844387076, 1.000000000000000000, 0.8660254037844387076, 1.000000000000000000, 0.8660254037844387076, 1.000000000000000000, 0.8660254037844387076, 1.000000000000000000, 0.8660254037844387076, 1.000000000000000000, 0.8660254037844387076, 1.000000000000000000, 0.8660254037844387076, 1.000000000000000000, 0.8660254037844387076, 1.000000000000000000, 0.8660254037844387076, 1.000000000000000000, 0.8660254037844387076, 1.000000000000000000, 0.8660254037844387076, 1.000000000000000000, 0.8660254037844387076, 1.000000000000000000, 0.8660254037844387076, 1.000000000000000000, 0.8660254037844387076, 1.000000000000000000, 0.8660254037844387076, 1.000000000000000000, 0.8660254037844387076, 1.000000000000000000, 0.8660254037844387076, 1.000000000000000000, 0.8660254037844387076, 1.000000000000000000, 0.8660254037844387076, 1.000000000000000000, 0.8660254037844387076, 1.000000000000000000, 0.8660254037844387076, 1.000000000000000000, 0.8660254037844387076, 1.000000000000000000, 0.8660254037844387076, 1.000000000000000000, 0.8660254037844387076, 1.000000000000000000, 0.8660254037844387076, 1.000000000000000000, 0.8660254037844387076, 1.000000000000000000, 0.8660254037844387076, 1.000000000000000000, 0.8660254037844387076, 1.000000000000000000, 0.8660254037844387076, 1.000000000000000000, 0.8660254037844387076, 1.000000000000000000, 0.8660254037844387076, 1.000000000000000000, 0.8660254037844387076, 1.000000000000000000, 0.8660254037844387076, 1.000000000000000000, 0.9548848677736607726, 0.9401542295229587953, 0.9401542295229587953, 0.9401542295229587953) ) ) 
 REPRESENTATION_ITEM ( '' )  SURFACE ( )  );
#31580 = CARTESIAN_POINT ( 'NONE',  ( 25.17756528844239483, 0.000000000000000000, 166.5920692191248804 ) ) ;
#31581 = CARTESIAN_POINT ( 'NONE',  ( 36.89981801693102170, 3.604726614523243278, 160.0988238161605750 ) ) ;
#31582 = CARTESIAN_POINT ( 'NONE',  ( 22.80587116629410360, 7.646167579472015790E-16, -1.715624999385545468 ) ) ;
#31583 = CARTESIAN_POINT ( 'NONE',  ( 24.61541074761292336, 3.464101615137757051, 160.1666134152087579 ) ) ;
#31584 = CARTESIAN_POINT ( 'NONE',  ( 24.00000000000000000, 243.4000000000000057, 5.196152422706629359 ) ) ;
#31585 = CARTESIAN_POINT ( 'NONE',  ( 1.069080835302379631E-14, 196.6250000012290400, 27.00000000000000000 ) ) ;
#31586 = CARTESIAN_POINT ( 'NONE',  ( -2.311890736173176641, 60.72268628210144925, -12.53471296425194659 ) ) ;
#31587 = ORIENTED_EDGE ( 'NONE', *, *, #18960, .T. ) ;
#31588 = ORIENTED_EDGE ( 'NONE', *, *, #12470, .T. ) ;
#31589 = CARTESIAN_POINT ( 'NONE',  ( 24.97492818644736445, -3.464101615137975543, 164.2759165448371732 ) ) ;
#31590 = AXIS2_PLACEMENT_3D ( 'NONE', #24586, #16068, #13780 ) ;
#31591 = CARTESIAN_POINT ( 'NONE',  ( 13.49999999999999645, 196.3625000012290513, -23.38268590217984766 ) ) ;
#31592 = CARTESIAN_POINT ( 'NONE',  ( 25.46681340963260354, 0.000000000000000000, 169.8981903728046916 ) ) ;
#31593 = CARTESIAN_POINT ( 'NONE',  ( 8.632099005475788900, 37.25231371789855217, -13.23911966647199812 ) ) ;
#31594 = CARTESIAN_POINT ( 'NONE',  ( 18.12178482187499640, 4.985214923628404904, -9.328124999385483562 ) ) ;
#31595 = ADVANCED_FACE ( 'NONE', ( #30280 ), #35581, .T. ) ;
#31596 = CARTESIAN_POINT ( 'NONE',  ( 26.75643035624999655, 243.8218750006145399, -3.323476615752271712 ) ) ;
#31597 = CARTESIAN_POINT ( 'NONE',  ( -41.88913769728823411, 207.8500491399821613, -3.954877714930864485 ) ) ;
#31598 = CARTESIAN_POINT ( 'NONE',  ( 15.00000000000000000, 242.8187500012290343, -3.464101615137752610 ) ) ;
#31599 = CARTESIAN_POINT ( 'NONE',  ( 36.93250142046140638, -3.604726614523238837, 160.4723968279450048 ) ) ;
#31600 = CARTESIAN_POINT ( 'NONE',  ( 1.715153634034445762, 18.27731371789853299, -9.534712964251895073 ) ) ;
#31601 = CARTESIAN_POINT ( 'NONE',  ( -68.60788769728823411, 216.4690446883607535, 1.857196546604031662 ) ) ;
#31602 = CARTESIAN_POINT ( 'NONE',  ( 27.05874960237330384, 195.0000000000000000, 2.090475941528396220 ) ) ;
#31603 = CARTESIAN_POINT ( 'NONE',  ( 27.24356964374999635, 195.6218750006145228, -15.72908226750539029 ) ) ;
#31604 = CARTESIAN_POINT ( 'NONE',  ( -6.092822981423666739, 137.0148137178985621, -14.25334919248795096 ) ) ;
#31605 = EDGE_LOOP ( 'NONE', ( #20086, #2035, #10984, #21498 ) ) ;
#31606 = CARTESIAN_POINT ( 'NONE',  ( -11.48171059495397373, 59.28518628210144215, -4.944772684328680334 ) ) ;
#31607 = CARTESIAN_POINT ( 'NONE',  ( 15.00000000000000000, 240.5500000000000114, 0.000000000000000000 ) ) ;
#31608 = EDGE_CURVE ( 'NONE', #32409, #34685, #11505, .T. ) ;
#31609 = CARTESIAN_POINT ( 'NONE',  ( 20.99999999999999289, 241.7874999999999659, -5.999999999999997335 ) ) ;
#31610 = CARTESIAN_POINT ( 'NONE',  ( 31.43172532185919721, 7.209453229046482114, 169.2351660368996420 ) ) ;
#31611 = CARTESIAN_POINT ( 'NONE',  ( 23.99999999999999645, 5.196152422706631135, -2.793749998770966858 ) ) ;
#31612 = CARTESIAN_POINT ( 'NONE',  ( 13.44051670066910731, 5.407089921784862696, -7.921874999385513760 ) ) ;
#31613 = CARTESIAN_POINT ( 'NONE',  ( -7.234628195640263826, 196.8700961906613713, -27.00000000000003553 ) ) ;
#31614 = CARTESIAN_POINT ( 'NONE',  ( 3.474262827703335166, 83.43518628210145494, 8.843639120294326972 ) ) ;
#31615 = CARTESIAN_POINT ( 'NONE',  ( 3.306546357697854128E-15, 200.0000000000000000, 27.00000000000000355 ) ) ;
#31616 = CARTESIAN_POINT ( 'NONE',  ( -10.69584247140444866, 94.64768628210146062, 6.932735513423972762 ) ) ;
#31617 = CARTESIAN_POINT ( 'NONE',  ( 22.60769515458673951, 249.6825961894323882, 5.999999999999998224 ) ) ;
#31618 = CYLINDRICAL_SURFACE ( 'NONE', #34340, 5.999999999999998224 ) ;
#31619 = ORIENTED_EDGE ( 'NONE', *, *, #670, .F. ) ;
#31620 = CARTESIAN_POINT ( 'NONE',  ( 30.78949644248743667, -7.209453229046475009, 161.8944563553360183 ) ) ;
#31621 = CARTESIAN_POINT ( 'NONE',  ( 18.12178482187499640, 4.985214923628404904, -6.515624999385460470 ) ) ;
#31622 = CARTESIAN_POINT ( 'NONE',  ( 3.373323998396211998, 195.0311615700027801, 29.51057501647288461 ) ) ;
#31623 = CARTESIAN_POINT ( 'NONE',  ( 28.25972136701633630, -5.407089921784865361, 168.7974587893581315 ) ) ;
#31624 = CARTESIAN_POINT ( 'NONE',  ( 28.11058759660888740, 5.196152422706636465, 165.6955278696240725 ) ) ;
#31625 = CARTESIAN_POINT ( 'NONE',  ( 25.21678537267883868, 0.000000000000000000, 167.0403568332661450 ) ) ;
#31626 = CARTESIAN_POINT ( 'NONE',  ( 21.00000000000000000, 240.0718750006145399, 6.646953231504538984 ) ) ;
#31627 = CARTESIAN_POINT ( 'NONE',  ( -13.62178482187500528, 199.7281250006145399, -23.59362340125807123 ) ) ;
#31628 = CARTESIAN_POINT ( 'NONE',  ( -10.49813415416004858, 116.0273137178985650, 7.228626920338839135 ) ) ;
#31629 = CARTESIAN_POINT ( 'NONE',  ( -0.1745138560725500443, 120.8101862821014691, 12.50000000000000355 ) ) ;
#31631 = VERTEX_POINT ( 'NONE', #16633 ) ;
#31630 = VERTEX_POINT ( 'NONE', #33492 ) ;
#31632 = CARTESIAN_POINT ( 'NONE',  ( 5.778771075727756162E-15, 197.6656250006145399, 31.45816453501075927 ) ) ;
#31633 = CARTESIAN_POINT ( 'NONE',  ( 15.24356964374999990, 241.1593750006145171, -3.323476615752268604 ) ) ;
#31634 = EDGE_CURVE ( 'NONE', #30240, #22958, #28175, .T. ) ;
#31635 = CARTESIAN_POINT ( 'NONE',  ( 15.00000000000000178, 243.7374999999999829, 3.464101615137757051 ) ) ;
#31636 = CARTESIAN_POINT ( 'NONE',  ( -11.08355503943118592, 90.43981371789854506, -10.83675517735179383 ) ) ;
#31637 = AXIS2_PLACEMENT_3D ( 'NONE', #17745, #29286, #3325 ) ;
#31638 = CARTESIAN_POINT ( 'NONE',  ( -2.311890736173176641, 88.32268628210144357, -12.53471296425194836 ) ) ;
#31639 = CARTESIAN_POINT ( 'NONE',  ( 21.00000000000000000, 6.646953231504538984, -2.615624999385474325 ) ) ;
#31640 = CARTESIAN_POINT ( 'NONE',  ( 13.49999999999999645, 196.8125000012290400, -23.38268590217984766 ) ) ;
#31641 = CARTESIAN_POINT ( 'NONE',  ( 2.064181346179061460, 68.30231371789852801, 9.465287035748106703 ) ) ;
#31642 = CARTESIAN_POINT ( 'NONE',  ( 16.56230152254411081, 7.209453229046475009, -3.403124999385538807 ) ) ;
#31643 =( BOUNDED_CURVE ( )  B_SPLINE_CURVE ( 2, ( #37485, #28774, #11536, #5287, #31808, #16867, #37119 ),
 .UNSPECIFIED., .F., .F. ) 
 B_SPLINE_CURVE_WITH_KNOTS ( ( 3, 2, 2, 3 ),
 ( 0.000000000000000000, 0.007246376811594299264, 0.01449275362318859853, 0.02173913043478289606 ),
 .UNSPECIFIED. ) 
 CURVE ( )  GEOMETRIC_REPRESENTATION_ITEM ( )  RATIONAL_B_SPLINE_CURVE ( ( 1.000000000000000000, 0.8660254037844387076, 1.000000000000000000, 0.8660254037844387076, 1.000000000000000000, 0.8660254037844333785, 1.000000000000005329 ) ) 
 REPRESENTATION_ITEM ( '' )  );
#31644 = CARTESIAN_POINT ( 'NONE',  ( 26.75643035624999655, 242.8093750006144944, -3.323476615752271268 ) ) ;
#31645 = CARTESIAN_POINT ( 'NONE',  ( 11.61527771782809637, 66.86481371789855643, 4.622313124798827388 ) ) ;
#31646 = CIRCLE ( 'NONE', #25675, 5.000000000000000000 ) ;
#31647 = LINE ( 'NONE', #17255, #11561 ) ;
#31648 = CARTESIAN_POINT ( 'NONE',  ( -10.49813415415989581, 123.9726862821014493, -7.228626920339068285 ) ) ;
#31649 = CARTESIAN_POINT ( 'NONE',  ( 22.56230152254409660, 3.464101615137755275, -2.774999998771003007 ) ) ;
#31650 = CARTESIAN_POINT ( 'NONE',  ( -48.81622103062156270, 211.6261429550005744, 6.530955311639227823 ) ) ;
#31651 = CARTESIAN_POINT ( 'NONE',  ( 5.438367727407757775E-14, 197.7500000012290400, -27.00000000000000355 ) ) ;
#31652 = FACE_OUTER_BOUND ( 'NONE', #9872, .T. ) ;
#31653 = CARTESIAN_POINT ( 'NONE',  ( 14.25334919248782661, 100.6851862821014834, 6.092822981423971385 ) ) ;
#31654 = CARTESIAN_POINT ( 'NONE',  ( -6.932735513423968321, 14.14768628210144641, -10.69584247140445221 ) ) ;
#31655 = DIRECTION ( 'NONE',  ( 0.000000000000000000, 1.000000000000000000, 0.000000000000000000 ) ) ;
#31656 = CARTESIAN_POINT ( 'NONE',  ( 18.00000000000000355, -5.196152422706632912, -2.568749998770964105 ) ) ;
#31657 = CARTESIAN_POINT ( 'NONE',  ( 3.474262827703335166, 129.4351862821014549, 8.843639120294326972 ) ) ;
#31658 = DIRECTION ( 'NONE',  ( 0.000000000000000000, 1.000000000000000000, 0.000000000000000000 ) ) ;
#31659 = ORIENTED_EDGE ( 'NONE', *, *, #31837, .T. ) ;
#31660 = CARTESIAN_POINT ( 'NONE',  ( 25.22662187717753568, 0.000000000000000000, 169.9474368419002985 ) ) ;
#31661 = CARTESIAN_POINT ( 'NONE',  ( -9.534712964251941258, 67.62268628210145494, 1.715153634034234154 ) ) ;
#31662 = DIRECTION ( 'NONE',  ( 0.08715574274765150453, 0.000000000000000000, 0.9961946980917461003 ) ) ;
#31663 = VECTOR ( 'NONE', #7657, 1000.000000000000000 ) ;
#31664 = DIRECTION ( 'NONE',  ( 0.000000000000000000, 0.000000000000000000, -1.000000000000000000 ) ) ;
#31665 = CARTESIAN_POINT ( 'NONE',  ( -49.64999999999999858, 244.5000000000000000, -2.499999999999997335 ) ) ;
#31666 = DIRECTION ( 'NONE',  ( 2.057406622567553763E-16, -0.000000000000000000, -1.000000000000000000 ) ) ;
#31667 = CARTESIAN_POINT ( 'NONE',  ( 15.00000000000000000, 0.000000000000000000, -3.093749998770961795 ) ) ;
#31668 = DIRECTION ( 'NONE',  ( 0.8191520442889772546, 0.000000000000000000, -0.5735764363510669206 ) ) ;
#31669 = CARTESIAN_POINT ( 'NONE',  ( 9.500000000000005329, 29.48981371789855288, -0.1745138560723090149 ) ) ;
#31670 = CARTESIAN_POINT ( 'NONE',  ( -13.62178482187498396, 199.0343750006145456, 23.59362340125808188 ) ) ;
#31671 = ORIENTED_EDGE ( 'NONE', *, *, #16982, .T. ) ;
#31672 = ORIENTED_EDGE ( 'NONE', *, *, #34842, .F. ) ;
#31673 = CARTESIAN_POINT ( 'NONE',  ( 23.87821517812500005, 248.5468750006145058, 4.985214923628404016 ) ) ;
#31674 = CARTESIAN_POINT ( 'NONE',  ( -12.53471296425189152, 43.57731371789855501, -2.311890736173453309 ) ) ;
#31675 = CARTESIAN_POINT ( 'NONE',  ( 22.80587116629412137, 7.646167579472024665E-16, -9.421874999385515537 ) ) ;
#31676 = CARTESIAN_POINT ( 'NONE',  ( 23.87821517812499650, 4.985214923628404904, -0.2906249993854803648 ) ) ;
#31677 = CARTESIAN_POINT ( 'NONE',  ( 8.927990412390371944, 141.3273137178985621, 13.04141134922778811 ) ) ;
#31678 = ORIENTED_EDGE ( 'NONE', *, *, #3211, .F. ) ;
#31679 = CARTESIAN_POINT ( 'NONE',  ( 13.44051670066911441, -5.407089921784865361, -4.621874999385545024 ) ) ;
#31680 = CARTESIAN_POINT ( 'NONE',  ( -13.62178482187498396, 198.5281250006145228, 23.59362340125808188 ) ) ;
#31681 = CARTESIAN_POINT ( 'NONE',  ( 24.87200694887302532, -3.604726614523244610, 165.8941696640395378 ) ) ;
#31682 = VECTOR ( 'NONE', #5920, 1000.000000000000000 ) ;
#31683 = CARTESIAN_POINT ( 'NONE',  ( -36.53794563604517265, 205.3262412349647832, 4.842901733360250205 ) ) ;
#31684 = FACE_OUTER_BOUND ( 'NONE', #32050, .T. ) ;
#31685 = SURFACE_STYLE_USAGE ( .BOTH. , #28285 ) ;
#31686 = CARTESIAN_POINT ( 'NONE',  ( 26.99999999999999289, 0.000000000000000000, 49.73803434254939759 ) ) ;
#31687 = CARTESIAN_POINT ( 'NONE',  ( -52.96502896937850124, 213.8393509191290889, -2.350049139982142155 ) ) ;
#31688 = CARTESIAN_POINT ( 'NONE',  ( -46.63913769728824121, 206.8500491399821044, -5.686928522499717253 ) ) ;
#31689 = CARTESIAN_POINT ( 'NONE',  ( 37.56492527877403376, -3.604726614523235284, 167.7010346059732342 ) ) ;
#31690 = ORIENTED_EDGE ( 'NONE', *, *, #33252, .F. ) ;
#31691 = DIRECTION ( 'NONE',  ( 0.000000000000000000, 0.000000000000000000, 1.000000000000000000 ) ) ;
#31692 = CARTESIAN_POINT ( 'NONE',  ( 31.29200377171331127, 6.928203230275514990, 167.6381414109090997 ) ) ;
#31693 = CARTESIAN_POINT ( 'NONE',  ( -8.927990412390371944, 26.32731371789854791, -13.04141134922778988 ) ) ;
#31694 = CARTESIAN_POINT ( 'NONE',  ( -57.12872103062156270, 201.4690446883607819, 2.162041339862843525 ) ) ;
#31695 =( GEOMETRIC_REPRESENTATION_CONTEXT ( 3 ) GLOBAL_UNCERTAINTY_ASSIGNED_CONTEXT ( ( #32824 ) ) GLOBAL_UNIT_ASSIGNED_CONTEXT ( ( #13710, #36811, #24887 ) ) REPRESENTATION_CONTEXT ( 'NONE', 'WORKASPACE' ) );
#31696 = CARTESIAN_POINT ( 'NONE',  ( 12.46528703574805874, 8.397686282101442856, 2.660918448318279950 ) ) ;
#31697 = EDGE_CURVE ( 'NONE', #19092, #12755, #13786, .T. ) ;
#31698 = CARTESIAN_POINT ( 'NONE',  ( 11.61527771782819940, 53.53518628210144925, -4.622313124798573369 ) ) ;
#31699 = EDGE_CURVE ( 'NONE', #17695, #6301, #25334, .T. ) ;
#31700 = CARTESIAN_POINT ( 'NONE',  ( 10.56230152254410726, 3.464101615137757051, -4.987500000000046008 ) ) ;
#31701 = ORIENTED_EDGE ( 'NONE', *, *, #11660, .T. ) ;
#31702 = CARTESIAN_POINT ( 'NONE',  ( -39.51413769728823411, 213.1499508600178672, 5.686928522499718142 ) ) ;
#31703 = CARTESIAN_POINT ( 'NONE',  ( 22.56230152254410370, 0.000000000000000000, -10.00000000000000000 ) ) ;
#31704 = CARTESIAN_POINT ( 'NONE',  ( 5.778771075727756162E-15, 196.8218750006145399, 31.45816453501075927 ) ) ;
#31705 = CARTESIAN_POINT ( 'NONE',  ( 36.86716609684025059, 7.347880794884125653E-16, 162.5202589094750181 ) ) ;
#31706 = CARTESIAN_POINT ( 'NONE',  ( 10.49999999999999467, 237.0000000000000000, 2.500000000000000000 ) ) ;
#31707 = LINE ( 'NONE', #14463, #27336 ) ;
#31708 = FACE_OUTER_BOUND ( 'NONE', #37353, .T. ) ;
#31709 = ADVANCED_FACE ( 'NONE', ( #25148 ), #31029, .T. ) ;
#31710 = CARTESIAN_POINT ( 'NONE',  ( 23.87821517812500005, 245.0593750006145228, 4.985214923628404016 ) ) ;
#31711 = CARTESIAN_POINT ( 'NONE',  ( -0.1745138560723084320, 91.58981371789856496, -9.500000000000005329 ) ) ;
#31712 = CARTESIAN_POINT ( 'NONE',  ( 26.75643035624999655, 242.4718750006145456, -3.323476615752271268 ) ) ;
#31713 = ORIENTED_EDGE ( 'NONE', *, *, #26383, .T. ) ;
#31714 = CARTESIAN_POINT ( 'NONE',  ( -51.58705436395488420, 205.3262412349647263, -4.842901733360204020 ) ) ;
#31715 = DIRECTION ( 'NONE',  ( -0.1219804832088933616, -0.9925324990730152175, 0.000000000000000000 ) ) ;
#31716 = CARTESIAN_POINT ( 'NONE',  ( 15.00000000000000178, 247.3937500012290229, 3.464101615137757051 ) ) ;
#31717 = EDGE_LOOP ( 'NONE', ( #6093, #1690, #28138, #10332 ) ) ;
#31718 = CARTESIAN_POINT ( 'NONE',  ( -2.311890736173447980, 96.47731371789855359, 12.53471296425189330 ) ) ;
#31719 = CARTESIAN_POINT ( 'NONE',  ( 22.80587116629411426, 3.604726614523243278, -2.184374999385525040 ) ) ;
#31720 = CARTESIAN_POINT ( 'NONE',  ( 33.78501001826630556, -5.407089921784855591, 160.3148693392417670 ) ) ;
#31721 = CARTESIAN_POINT ( 'NONE',  ( 15.24356964375000167, -3.323476615752272600, -1.565624999385462957 ) ) ;
#31722 = CARTESIAN_POINT ( 'NONE',  ( 12.53471296425189330, 57.37731371789855928, 2.311890736173451977 ) ) ;
#31723 = CARTESIAN_POINT ( 'NONE',  ( 5.778771075727756162E-15, 199.0718750006145399, 31.45816453501075927 ) ) ;
#31724 = ORIENTED_EDGE ( 'NONE', *, *, #6389, .T. ) ;
#31725 = ORIENTED_EDGE ( 'NONE', *, *, #4364, .T. ) ;
#31726 = VERTEX_POINT ( 'NONE', #31395 ) ;
#31727 = CARTESIAN_POINT ( 'NONE',  ( 26.99999999999999645, 7.347880794884117764E-16, -6.468749998770951137 ) ) ;
#31729 = PRESENTATION_LAYER_ASSIGNMENT (  '', '', ( #34135 ) ) ;
#31728 = CARTESIAN_POINT ( 'NONE',  ( 15.24356964374999990, 0.000000000000000000, -2.390624999385471128 ) ) ;
#31730 = CARTESIAN_POINT ( 'NONE',  ( 26.97716818855048260, 0.000000000000000000, 49.47706554351410801 ) ) ;
#31731 = CARTESIAN_POINT ( 'NONE',  ( 26.75643035624999655, 247.7593750006145399, -3.323476615752271712 ) ) ;
#31732 = CARTESIAN_POINT ( 'NONE',  ( 10.69584247140445221, 53.24768628210144072, -6.932735513423970097 ) ) ;
#31733 = CIRCLE ( 'NONE', #3891, 2.649999999999985700 ) ;
#31734 = CARTESIAN_POINT ( 'NONE',  ( -53.75669563604516554, 209.8844732041982013, -6.500000000000000888 ) ) ;
#31735 = CARTESIAN_POINT ( 'NONE',  ( 14.62176384545913699, 216.3782361545713400, -2.408991313803013679 ) ) ;
#31736 = CARTESIAN_POINT ( 'NONE',  ( -40.29836230271183695, 206.0451222850691977, -2.149950860017851184 ) ) ;
#31737 = CARTESIAN_POINT ( 'NONE',  ( 36.79526260918054703, -3.464101615137751278, 161.6983982847737025 ) ) ;
#31738 = CARTESIAN_POINT ( 'NONE',  ( -12.53471296425189152, 98.77731371789855075, -2.311890736173453753 ) ) ;
#31739 = CARTESIAN_POINT ( 'NONE',  ( -57.32663769728824121, 206.0451222850691408, 2.149950860017832532 ) ) ;
#31740 =( BOUNDED_CURVE ( )  B_SPLINE_CURVE ( 2, ( #12503, #24067, #9658, #21235, #28022, #13998, #36545 ),
 .UNSPECIFIED., .F., .F. ) 
 B_SPLINE_CURVE_WITH_KNOTS ( ( 3, 2, 2, 3 ),
 ( 0.1304347826086947049, 0.1376811594202889955, 0.1449275362318833138, 0.1521739130434776044 ),
 .UNSPECIFIED. ) 
 CURVE ( )  GEOMETRIC_REPRESENTATION_ITEM ( )  RATIONAL_B_SPLINE_CURVE ( ( 1.000000000000017319, 0.8660254037844211661, 1.000000000000000000, 0.8660254037844387076, 1.000000000000000000, 0.8660254037844510311, 0.9999999999999876765 ) ) 
 REPRESENTATION_ITEM ( '' )  );
#31741 = CARTESIAN_POINT ( 'NONE',  ( -45.45163769728823411, 217.4189793300686233, -4.149950860017907139 ) ) ;
#31742 = CARTESIAN_POINT ( 'NONE',  ( 20.99999999999999645, 6.646953231504538984, -4.865624999385484983 ) ) ;
#31743 = DIRECTION ( 'NONE',  ( -0.000000000000000000, -0.000000000000000000, -1.000000000000000000 ) ) ;
#31744 = CARTESIAN_POINT ( 'NONE',  ( 13.04141134922778988, 74.62731371789853085, -8.927990412390371944 ) ) ;
#31745 = CARTESIAN_POINT ( 'NONE',  ( -34.75669563604516554, 209.8844732041982013, -6.500000000000000888 ) ) ;
#31746 = EDGE_LOOP ( 'NONE', ( #1232, #12363, #25642, #33084, #18804, #31073, #24279, #23533, #3615, #34240, #31355, #14577, #5941, #11630, #15710, #12097, #9766, #27205, #2307, #8377, #11982, #2349, #7336, #2397, #12803, #4691 ) ) ;
#31747 = LINE ( 'NONE', #11103, #9562 ) ;
#31748 = CARTESIAN_POINT ( 'NONE',  ( -8.962234695871760692, 112.7601862821014720, 8.715434833791933400 ) ) ;
#31749 = CARTESIAN_POINT ( 'NONE',  ( -14.25334919248782306, 40.88518628210145067, -6.092822981423979378 ) ) ;
#31750 = DIRECTION ( 'NONE',  ( 1.045431693899523378E-14, 0.1163425707149433885, -0.9932091452657081376 ) ) ;
#31751 = CARTESIAN_POINT ( 'NONE',  ( 24.51902619074504130, -3.604726614523244610, 161.8595811367679573 ) ) ;
#31752 = CARTESIAN_POINT ( 'NONE',  ( 15.53471296425195369, 72.22268628210143504, -2.908627838312120684 ) ) ;
#31753 = CARTESIAN_POINT ( 'NONE',  ( 16.56230152254411081, 7.209453229046475009, -8.803124999385520510 ) ) ;
#31754 = CARTESIAN_POINT ( 'NONE',  ( 20.99999999999999645, 240.2687500012290513, 5.999999999999998224 ) ) ;
#31755 = CARTESIAN_POINT ( 'NONE',  ( -52.37872103062156270, 203.4690446883607535, 1.626142955000567936 ) ) ;
#31756 = CARTESIAN_POINT ( 'NONE',  ( 28.38512818626399081, 5.196152422706636465, 168.8335411686130669 ) ) ;
#31757 = CARTESIAN_POINT ( 'NONE',  ( -8.715434833791929847, 41.46018628210144641, -8.962234695871762469 ) ) ;
#31758 = CARTESIAN_POINT ( 'NONE',  ( -13.49999999999998401, 195.5749999999999886, 23.38268590217985476 ) ) ;
#31759 = PLANE ( 'NONE',  #28082 ) ;
#31760 = CARTESIAN_POINT ( 'NONE',  ( -6.594114490232462877, 143.3398137178985507, 6.840914352311949109 ) ) ;
#31761 = CARTESIAN_POINT ( 'NONE',  ( 26.75643035624999655, 249.1843750006145228, -7.049594010296217766E-16 ) ) ;
#31762 = VERTEX_POINT ( 'NONE', #2020 ) ;
#31763 = CARTESIAN_POINT ( 'NONE',  ( 21.00000000000000000, -6.928203230275506996, -3.937500000000003109 ) ) ;
#31764 = CARTESIAN_POINT ( 'NONE',  ( 30.66693367924855096, -7.209453229046482114, 160.4935575611445415 ) ) ;
#31765 = CARTESIAN_POINT ( 'NONE',  ( 10.31873187879411091, 0.000000000000000000, -4.640624999385528859 ) ) ;
#31766 = CARTESIAN_POINT ( 'NONE',  ( 37.61068204371655099, 3.604726614523238837, 168.2240368224713620 ) ) ;
#31767 = CARTESIAN_POINT ( 'NONE',  ( 18.00000000000000000, 242.2749999999999773, -5.196152422706630247 ) ) ;
#31768 = CARTESIAN_POINT ( 'NONE',  ( -11.48171059495397373, 59.28518628210144215, -4.944772684328680334 ) ) ;
#31769 = ORIENTED_EDGE ( 'NONE', *, *, #32048, .F. ) ;
#31770 = ORIENTED_EDGE ( 'NONE', *, *, #25170, .T. ) ;
#31771 = CARTESIAN_POINT ( 'NONE',  ( 24.63175244948454434, -3.464101615137358703, 160.3533999223253943 ) ) ;
#31772 = CARTESIAN_POINT ( 'NONE',  ( -27.00000000000000355, 196.0625000012290400, 0.000000000000000000 ) ) ;
#31773 = CARTESIAN_POINT ( 'NONE',  ( -13.49999999999998401, 196.5875000012290457, 23.38268590217985476 ) ) ;
#31774 = CARTESIAN_POINT ( 'NONE',  ( 11.08355503943118769, 39.83981371789855075, 10.83675517735179028 ) ) ;
#31775 = CARTESIAN_POINT ( 'NONE',  ( 22.60769515458673595, 249.2325961894323711, 5.999999999999999112 ) ) ;
#31776 = CARTESIAN_POINT ( 'NONE',  ( 18.12178482187500350, 240.4843750006145342, 4.985214923628407568 ) ) ;
#31777 = CARTESIAN_POINT ( 'NONE',  ( -44.85788769728823411, 214.4690446883608104, 1.321298161741840893 ) ) ;
#31778 = CARTESIAN_POINT ( 'NONE',  ( 10.56230152254410548, 0.000000000000000000, -9.000000000000035527 ) ) ;
#31779 = CARTESIAN_POINT ( 'NONE',  ( 24.39809759768267128, 0.000000000000000000, 160.4773609931656608 ) ) ;
#31780 = CARTESIAN_POINT ( 'NONE',  ( -5.233372021372612259, 23.45231371789854435, 8.152565276336593669 ) ) ;
#31781 = CARTESIAN_POINT ( 'NONE',  ( 10.31873187879411091, 0.000000000000000000, -9.140624999385559946 ) ) ;
#31782 = AXIS2_PLACEMENT_3D ( 'NONE', #9105, #17645, #14793 ) ;
#31783 = DIRECTION ( 'NONE',  ( 0.9961946980917462113, -0.08715574274765144902, 0.000000000000000000 ) ) ;
#31784 = CARTESIAN_POINT ( 'NONE',  ( 21.00000000000016342, 4.000000000000002665, 50.00000000000000000 ) ) ;
#31785 = CARTESIAN_POINT ( 'NONE',  ( 5.778771075727756162E-15, 196.8218750006145399, 31.45816453501075927 ) ) ;
#31786 = CARTESIAN_POINT ( 'NONE',  ( 8.927990412390371944, 122.9273137178985422, 13.04141134922778811 ) ) ;
#31787 = EDGE_LOOP ( 'NONE', ( #37401, #36896 ) ) ;
#31788 = CARTESIAN_POINT ( 'NONE',  ( 6.932735513423970097, 46.34768628210145636, 10.69584247140445044 ) ) ;
#31789 = CARTESIAN_POINT ( 'NONE',  ( 22.56230152254410015, 7.347880794884117764E-16, -8.212499998771022547 ) ) ;
#31790 = CARTESIAN_POINT ( 'NONE',  ( 0.000000000000000000, 195.0000000000000000, 0.000000000000000000 ) ) ;
#31791 = CARTESIAN_POINT ( 'NONE',  ( 30.61300606342344111, 7.209453229046475009, 159.8771620917002565 ) ) ;
#31792 = CARTESIAN_POINT ( 'NONE',  ( 21.00000000000000000, 6.928203230275506996, -3.206249998770952292 ) ) ;
#31793 = CARTESIAN_POINT ( 'NONE',  ( 16.56230152254411436, 7.209453229046482114, -7.959374999385476102 ) ) ;
#31794 = CARTESIAN_POINT ( 'NONE',  ( 20.99999999999997868, 244.7687500012290513, 5.999999999999999112 ) ) ;
#31795 = CARTESIAN_POINT ( 'NONE',  ( 3.796722387233379514, 70.78518628210143504, -8.710071997420127943 ) ) ;
#31796 = CARTESIAN_POINT ( 'NONE',  ( 0.000000000000000000, 143.0000000000000000, 0.000000000000000000 ) ) ;
#31797 = CARTESIAN_POINT ( 'NONE',  ( 22.60769515458672885, 245.8174038105676971, -5.999999999999998224 ) ) ;
#31798 = CARTESIAN_POINT ( 'NONE',  ( 8.715434833791931624, 92.06018628210145494, 8.962234695871760692 ) ) ;
#31799 = CARTESIAN_POINT ( 'NONE',  ( 26.99999999999999645, 249.8125000000000000, -3.464101615137755275 ) ) ;
#31800 = DIRECTION ( 'NONE',  ( 1.000000000000000000, 0.000000000000000000, 0.000000000000000000 ) ) ;
#31801 = ORIENTED_EDGE ( 'NONE', *, *, #6126, .T. ) ;
#31802 = CARTESIAN_POINT ( 'NONE',  ( 37.05833252405330569, 7.646167579472015790E-16, 161.9106529233149274 ) ) ;
#31803 = AXIS2_PLACEMENT_3D ( 'NONE', #32226, #29571, #18217 ) ;
#31804 = CARTESIAN_POINT ( 'NONE',  ( 15.24356964374999990, 0.000000000000000000, -6.890624999385474680 ) ) ;
#31805 = CARTESIAN_POINT ( 'NONE',  ( -13.62178482187498396, 195.8843750006145399, 23.59362340125808188 ) ) ;
#31806 = CARTESIAN_POINT ( 'NONE',  ( 28.22050128277989245, -5.407089921784865361, 168.3491711752168385 ) ) ;
#31807 = CARTESIAN_POINT ( 'NONE',  ( 37.06326651802246630, 7.347880794884125653E-16, 164.7616969801814548 ) ) ;
#31808 = CARTESIAN_POINT ( 'NONE',  ( 23.99999999999999645, 5.196152422706631135, -0.1500000000000112355 ) ) ;
#31809 = CARTESIAN_POINT ( 'NONE',  ( 21.00000000000000000, 247.1875000000000000, -6.928203230275506996 ) ) ;
#31810 = CARTESIAN_POINT ( 'NONE',  ( -13.62178482187500528, 198.8281250006145342, -23.59362340125807123 ) ) ;
#31811 = AXIS2_PLACEMENT_3D ( 'NONE', #32414, #9115, #35065 ) ;
#31812 = CARTESIAN_POINT ( 'NONE',  ( 2.311890736173452865, 119.4773137178985678, -12.53471296425189152 ) ) ;
#31813 = CARTESIAN_POINT ( 'NONE',  ( -8.962234695871760692, 121.9601862821014464, 8.715434833791933400 ) ) ;
#31815 = ORIENTED_EDGE ( 'NONE', *, *, #18426, .T. ) ;
#31814 = ORIENTED_EDGE ( 'NONE', *, *, #26302, .F. ) ;
#31816 = CARTESIAN_POINT ( 'NONE',  ( -27.24356964375000345, 199.3531250006145399, 0.000000000000000000 ) ) ;
#31817 = CARTESIAN_POINT ( 'NONE',  ( 26.75643035624999655, 243.2218750006145171, -7.049594010296217766E-16 ) ) ;
#31818 = CARTESIAN_POINT ( 'NONE',  ( 15.00000000000000355, 7.347880794884112834E-16, -8.000000000000000000 ) ) ;
#31819 = CARTESIAN_POINT ( 'NONE',  ( -8.927990412390371944, 90.72731371789855359, -13.04141134922778988 ) ) ;
#31820 = EDGE_CURVE ( 'NONE', #27666, #34054, #28357, .T. ) ;
#31821 = CARTESIAN_POINT ( 'NONE',  ( 26.75643035624999655, 3.323476615752271712, -3.590624999385491734 ) ) ;
#31822 = CARTESIAN_POINT ( 'NONE',  ( 18.12178482187499640, 247.5343750006145456, -4.985214923628404904 ) ) ;
#31823 = CARTESIAN_POINT ( 'NONE',  ( -13.50000000000000533, 195.9875000012290229, -23.38268590217984411 ) ) ;
#31824 = CARTESIAN_POINT ( 'NONE',  ( -3.474262827703527901, 78.36481371789855643, 8.843639120294245259 ) ) ;
#31825 = CARTESIAN_POINT ( 'NONE',  ( 13.44051670066911441, -5.407089921784859143, -2.315624999385534899 ) ) ;
#31826 = ADVANCED_FACE ( 'NONE', ( #19482 ), #2393, .F. ) ;
#31827 = CARTESIAN_POINT ( 'NONE',  ( 15.24356964374999990, 242.5468750006145058, 0.000000000000000000 ) ) ;
#31828 = CARTESIAN_POINT ( 'NONE',  ( 0.1745138560722779009, 50.18981371789854506, 12.50000000000000355 ) ) ;
#31829 = DIRECTION ( 'NONE',  ( 1.000000000000000000, 0.000000000000000000, 0.000000000000000000 ) ) ;
#31830 = CARTESIAN_POINT ( 'NONE',  ( -8.962234695871760692, 94.36018628210145209, 8.715434833791933400 ) ) ;
#31831 = CARTESIAN_POINT ( 'NONE',  ( 22.56230152254410370, 7.347880794884117764E-16, -4.162499998770996967 ) ) ;
#31832 = ADVANCED_FACE ( 'NONE', ( #13967 ), #33680, .F. ) ;
#31833 = CARTESIAN_POINT ( 'NONE',  ( -35.95163769728823411, 215.6869285224996986, -3.149950860017881382 ) ) ;
#31834 = LINE ( 'NONE', #5867, #19191 ) ;
#31835 = CARTESIAN_POINT ( 'NONE',  ( 27.71838675424445597, 5.196152422706636465, 161.2126517282112275 ) ) ;
#31836 = CARTESIAN_POINT ( 'NONE',  ( -14.25334919248782306, 105.2851862821014777, -6.092822981423979378 ) ) ;
#31837 = EDGE_CURVE ( 'NONE', #3147, #4722, #5063, .T. ) ;
#31838 = CARTESIAN_POINT ( 'NONE',  ( 12.50000000000000355, 8.110186282101444988, 0.1745138560725507937 ) ) ;
#31839 = DIRECTION ( 'NONE',  ( 0.08715574274765150453, 0.000000000000000000, 0.9961946980917461003 ) ) ;
#31840 =( BOUNDED_CURVE ( )  B_SPLINE_CURVE ( 2, ( #22552, #8697, #31627, #2627, #9073, #32000, #14573, #11169, #25944, #5847, #22742, #11722, #20643, #28406, #6030, #5289, #17616, #16869, #20083, #28589, #37487, #2816, #37121, #26125, #2445, #26307, #31810, #5469, #14019, #25569, #23476, #29146, #34292, #5655, #34473, #8335, #22928, #14386, #11538, #28964, #8516, #28776, #23109, #11909, #11357, #19905, #3187, #17237, #14203, #3003, #34653, #20271, #25754, #157, #23296, #17425, #34841, #8881, #20459, #35029, #31446, #14762, #37307, #17051, #344, #526, #15515, #15325, #27257, #32375, #21025, #32938, #6992, #32560, #6413, #21212, #15132, #12093, #12286, #29340, #23667, #21398, #907, #27071, #35967, #35211, #1095, #6602, #23859, #12664, #35398, #9261, #14947, #32751, #9820, #24420, #18560, #3571, #29911, #9635, #9446, #29531, #6224, #18176, #35590, #29717, #26684, #24232, #3750, #26876, #12477, #24045, #714, #10005, #6788, #4134, #17988, #18363, #3940, #35776, #32190, #30102, #15706, #20833, #1280, #26494, #12851, #17797, #3378, #16644, #16455 ),
 .UNSPECIFIED., .F., .F. ) 
 B_SPLINE_CURVE_WITH_KNOTS ( ( 3, 2, 2, 2, 2, 2, 2, 2, 2, 2, 2, 2, 2, 2, 2, 2, 2, 2, 2, 2, 2, 2, 2, 2, 2, 2, 2, 2, 2, 2, 2, 2, 2, 2, 2, 2, 2, 2, 2, 2, 2, 2, 2, 2, 2, 2, 2, 2, 2, 2, 2, 2, 2, 2, 2, 2, 2, 2, 2, 2, 2, 2, 2, 2, 2, 3 ),
 ( 0.000000000000000000, 0.01388888888888888812, 0.02777777777777777624, 0.04166666666666666435, 0.05555555555555555247, 0.06944444444444444753, 0.08333333333333332871, 0.09722222222222223764, 0.1111111111111111049, 0.1250000000000000000, 0.1388888888888888951, 0.1527777777777777901, 0.1666666666666666574, 0.1805555555555555247, 0.1944444444444444753, 0.2083333333333333426, 0.2222222222222222099, 0.2361111111111111049, 0.2500000000000000000, 0.2638888888888888951, 0.2777777777777777901, 0.2916666666666666852, 0.3055555555555555802, 0.3194444444444444198, 0.3333333333333333148, 0.3472222222222222099, 0.3611111111111110494, 0.3750000000000000000, 0.3888888888888889506, 0.4027777777777777901, 0.4166666666666666852, 0.4305555555555555802, 0.4444444444444444198, 0.4583333333333333148, 0.4722222222222222099, 0.4861111111111110494, 0.5000000000000000000, 0.5138888888888888395, 0.5277777777777777901, 0.5416666666666666297, 0.5555555555555555802, 0.5694444444444444198, 0.5833333333333333703, 0.5972222222222222099, 0.6111111111111111605, 0.6250000000000001110, 0.6388888888888888395, 0.6527777777777777901, 0.6666666666666666297, 0.6805555555555555802, 0.6944444444444444198, 0.7083333333333333703, 0.7222222222222220989, 0.7361111111111111605, 0.7500000000000000000, 0.7638888888888888395, 0.7777777777777779011, 0.7916666666666666297, 0.8055555555555555802, 0.8194444444444444198, 0.8333333333333333703, 0.8472222222222222099, 0.8611111111111111605, 0.8749999999999998890, 0.8888888888888888395, 0.8895442836098168549 ),
 .UNSPECIFIED. ) 
 CURVE ( )  GEOMETRIC_REPRESENTATION_ITEM ( )  RATIONAL_B_SPLINE_CURVE ( ( 1.000000000000000000, 0.8660254037844387076, 1.000000000000000000, 0.8660254037844387076, 1.000000000000000000, 0.8660254037844387076, 1.000000000000000000, 0.8660254037844387076, 1.000000000000000000, 0.8660254037844387076, 1.000000000000000000, 0.8660254037844387076, 1.000000000000000000, 0.8660254037844387076, 1.000000000000000000, 0.8660254037844387076, 1.000000000000000000, 0.8660254037844387076, 1.000000000000000000, 0.8660254037844387076, 1.000000000000000000, 0.8660254037844387076, 1.000000000000000000, 0.8660254037844387076, 1.000000000000000000, 0.8660254037844387076, 1.000000000000000000, 0.8660254037844387076, 1.000000000000000000, 0.8660254037844387076, 1.000000000000000000, 0.8660254037844387076, 1.000000000000000000, 0.8660254037844387076, 1.000000000000000000, 0.8660254037844387076, 1.000000000000000000, 0.8660254037844387076, 1.000000000000000000, 0.8660254037844387076, 1.000000000000000000, 0.8660254037844387076, 1.000000000000000000, 0.8660254037844387076, 1.000000000000000000, 0.8660254037844387076, 1.000000000000000000, 0.8660254037844387076, 1.000000000000000000, 0.8660254037844387076, 1.000000000000000000, 0.8660254037844387076, 1.000000000000000000, 0.8660254037844387076, 1.000000000000000000, 0.8660254037844387076, 1.000000000000000000, 0.8660254037844387076, 1.000000000000000000, 0.8660254037844387076, 1.000000000000000000, 0.8660254037844387076, 1.000000000000000000, 0.8660254037844387076, 1.000000000000000000, 0.8660254037844387076, 1.000000000000000000, 0.8660254037844387076, 1.000000000000000000, 0.8660254037844387076, 1.000000000000000000, 0.8660254037844387076, 1.000000000000000000, 0.8660254037844387076, 1.000000000000000000, 0.8660254037844387076, 1.000000000000000000, 0.8660254037844387076, 1.000000000000000000, 0.8660254037844387076, 1.000000000000000000, 0.8660254037844387076, 1.000000000000000000, 0.8660254037844387076, 1.000000000000000000, 0.8660254037844387076, 1.000000000000000000, 0.8660254037844387076, 1.000000000000000000, 0.8660254037844387076, 1.000000000000000000, 0.8660254037844387076, 1.000000000000000000, 0.8660254037844387076, 1.000000000000000000, 0.8660254037844387076, 1.000000000000000000, 0.8660254037844387076, 1.000000000000000000, 0.8660254037844387076, 1.000000000000000000, 0.8660254037844387076, 1.000000000000000000, 0.8660254037844387076, 1.000000000000000000, 0.8660254037844387076, 1.000000000000000000, 0.8660254037844387076, 1.000000000000000000, 0.8660254037844387076, 1.000000000000000000, 0.8660254037844387076, 1.000000000000000000, 0.8660254037844387076, 1.000000000000000000, 0.8660254037844387076, 1.000000000000000000, 0.8660254037844387076, 1.000000000000000000, 0.8660254037844387076, 1.000000000000000000, 0.8660254037844387076, 1.000000000000000000, 0.8660254037844387076, 1.000000000000000000, 0.8660254037844387076, 1.000000000000000000, 0.8660254037844387076, 1.000000000000000000, 0.9936779504969338594, 0.9879525560471125178 ) ) 
 REPRESENTATION_ITEM ( '' )  );
#31841 = CARTESIAN_POINT ( 'NONE',  ( 13.49999999999999645, 196.8125000012290400, -23.38268590217984766 ) ) ;
#31842 = CARTESIAN_POINT ( 'NONE',  ( -9.534712964251941258, 132.0226862821014322, 1.715153634034234154 ) ) ;
#31843 = CARTESIAN_POINT ( 'NONE',  ( 15.24356964374999990, 242.5468750006145058, 0.000000000000000000 ) ) ;
#31844 = ORIENTED_EDGE ( 'NONE', *, *, #9236, .F. ) ;
#31845 = CARTESIAN_POINT ( 'NONE',  ( 28.22540379330944660, -5.407089921784859143, 168.4052071269844930 ) ) ;
#31846 = CARTESIAN_POINT ( 'NONE',  ( -6.594114490232312775, 59.86018628210145209, -6.840914352312096547 ) ) ;
#31847 = CARTESIAN_POINT ( 'NONE',  ( 21.00000000000000000, 6.646953231504538984, -1.153124999385464200 ) ) ;
#31848 = AXIS2_PLACEMENT_3D ( 'NONE', #29882, #6385, #20996 ) ;
#31849 = CARTESIAN_POINT ( 'NONE',  ( -20.86978604919638869, 194.8026013911397456, -17.51182792271053046 ) ) ;
#31850 = DIRECTION ( 'NONE',  ( -0.000000000000000000, 1.000000000000000000, -0.000000000000000000 ) ) ;
#31851 = DIRECTION ( 'NONE',  ( -0.000000000000000000, -1.000000000000000000, -0.000000000000000000 ) ) ;
#31852 = CARTESIAN_POINT ( 'NONE',  ( 0.6823418707358707147, 194.9999999999999716, 27.29152404244862495 ) ) ;
#31853 = CARTESIAN_POINT ( 'NONE',  ( -27.00000000000000355, 196.9625000012290172, 0.000000000000000000 ) ) ;
#31854 = CARTESIAN_POINT ( 'NONE',  ( 7.954856959092311719, 37.82731371789854080, -5.529263428287300108 ) ) ;
#31855 = FACE_OUTER_BOUND ( 'NONE', #6405, .T. ) ;
#31856 = VERTEX_POINT ( 'NONE', #10742 ) ;
#31857 = VERTEX_POINT ( 'NONE', #8097 ) ;
#31858 = CARTESIAN_POINT ( 'NONE',  ( 23.87821517812500005, 248.9968750006145228, 4.985214923628404016 ) ) ;
#31859 = CARTESIAN_POINT ( 'NONE',  ( -0.1745138560722763466, 36.38981371789855501, -12.50000000000000355 ) ) ;
#31860 = CARTESIAN_POINT ( 'NONE',  ( 10.31873187879410736, -3.604726614523244610, -8.709374999385511629 ) ) ;
#31861 = CARTESIAN_POINT ( 'NONE',  ( 15.24356964374999990, 3.323476615752268604, -8.840624999385484628 ) ) ;
#31862 = CARTESIAN_POINT ( 'NONE',  ( 8.715434833792128799, 9.939813717898537959, -8.962234695871567070 ) ) ;
#31863 = ORIENTED_EDGE ( 'NONE', *, *, #23768, .T. ) ;
#31864 = CARTESIAN_POINT ( 'NONE',  ( 13.44051670066910908, 5.407089921784862696, -4.771874999385556038 ) ) ;
#31865 = CARTESIAN_POINT ( 'NONE',  ( -13.62178482187500528, 198.3781250006145171, -23.59362340125807123 ) ) ;
#31866 = ADVANCED_FACE ( 'NONE', ( #19670 ), #16445, .T. ) ;
#31867 = CARTESIAN_POINT ( 'NONE',  ( 25.06157068934916765, 3.604726614523240613, 168.0608931323890829 ) ) ;
#31868 = EDGE_CURVE ( 'NONE', #30804, #33968, #16995, .T. ) ;
#31869 = CARTESIAN_POINT ( 'NONE',  ( -64.44419563604517975, 201.5000000000000000, 0.1155267958018195706 ) ) ;
#31870 = CARTESIAN_POINT ( 'NONE',  ( 15.24356964375000167, 247.9843750006145058, 3.323476615752272600 ) ) ;
#31871 =( NAMED_UNIT ( * ) PLANE_ANGLE_UNIT ( ) SI_UNIT ( $, .RADIAN. ) );
#31872 = AXIS2_PLACEMENT_3D ( 'NONE', #4480, #23688, #26148 ) ;
#31873 = CARTESIAN_POINT ( 'NONE',  ( -22.74142690944354683, 194.9999999999999716, 14.88791141736823498 ) ) ;
#31874 = EDGE_CURVE ( 'NONE', #31762, #11777, #23348, .T. ) ;
#31875 = CARTESIAN_POINT ( 'NONE',  ( -60.48586230271183695, 207.8500491399821613, 3.954877714930852495 ) ) ;
#31876 = CARTESIAN_POINT ( 'NONE',  ( -50.79538769728821990, 211.8571965466039444, -6.469044688360768625 ) ) ;
#31877 = CARTESIAN_POINT ( 'NONE',  ( 34.46482481169798717, 5.407089921784857367, 168.0851879843573897 ) ) ;
#31878 = ORIENTED_EDGE ( 'NONE', *, *, #10257, .T. ) ;
#31879 = CARTESIAN_POINT ( 'NONE',  ( 2.999999999999997335, 244.5000000000000000, -2.499999999999999556 ) ) ;
#31880 = CARTESIAN_POINT ( 'NONE',  ( 34.27731952563551232, 5.196152422706637353, 167.3393168814877185 ) ) ;
#31881 = CARTESIAN_POINT ( 'NONE',  ( -15.50000000000000533, 24.88981371789854080, 0.1745138560722471477 ) ) ;
#31882 = CARTESIAN_POINT ( 'NONE',  ( -58.11830436395491262, 209.8844732041983150, 8.500000000000003553 ) ) ;
#31883 = CARTESIAN_POINT ( 'NONE',  ( -5.529263428287477744, 140.0726862821014151, 7.954856959092191815 ) ) ;
#31884 = CARTESIAN_POINT ( 'NONE',  ( 4.622313124798573369, 46.63518628210145067, 11.61527771782819940 ) ) ;
#31885 = CARTESIAN_POINT ( 'NONE',  ( 19.56230152254412502, -5.196152422706635576, -3.900000000000070077 ) ) ;
#31886 = ORIENTED_EDGE ( 'NONE', *, *, #27416, .T. ) ;
#31887 = CARTESIAN_POINT ( 'NONE',  ( -37.73288769728822700, 203.5309553116391896, -1.857196546604028997 ) ) ;
#31888 = CARTESIAN_POINT ( 'NONE',  ( 10.56230152254410726, 0.000000000000000000, -0.9000000000000396572 ) ) ;
#31889 = VECTOR ( 'NONE', #32405, 1000.000000000000000 ) ;
#31890 = CARTESIAN_POINT ( 'NONE',  ( 5.778771075727756162E-15, 195.4718750006145456, 31.45816453501075927 ) ) ;
#31891 = CARTESIAN_POINT ( 'NONE',  ( -7.234628195640316228, 199.0075961894323200, -27.00000000000000000 ) ) ;
#31892 = CARTESIAN_POINT ( 'NONE',  ( -26.99999999999999645, 198.6875000000000284, 15.58845726811991561 ) ) ;
#31893 = CARTESIAN_POINT ( 'NONE',  ( 27.00000000000001421, 197.4875000000000114, 15.58845726811988897 ) ) ;
#31894 = LINE ( 'NONE', #2706, #32076 ) ;
#31895 = CARTESIAN_POINT ( 'NONE',  ( 21.00000000000000000, 246.3718750006145228, 6.646953231504538984 ) ) ;
#31896 = CARTESIAN_POINT ( 'NONE',  ( -7.954856959092309943, 97.62731371789854506, 5.529263428287300108 ) ) ;
#31897 = CARTESIAN_POINT ( 'NONE',  ( 26.75643035624999655, 240.1843750006145513, -7.049594010296217766E-16 ) ) ;
#31898 = VERTEX_POINT ( 'NONE', #2946 ) ;
#31899 = CARTESIAN_POINT ( 'NONE',  ( -59.30580436395489841, 216.5000000000000000, 0.1155267958017343610 ) ) ;
#31900 = DIRECTION ( 'NONE',  ( 0.08715574274765150453, 0.000000000000000000, 0.9961946980917461003 ) ) ;
#31901 = AXIS2_PLACEMENT_3D ( 'NONE', #5346, #16924, #2501 ) ;
#31902 = CARTESIAN_POINT ( 'NONE',  ( 26.99999999999999645, 245.7812500012290400, -7.347880794884117764E-16 ) ) ;
#31903 = VERTEX_POINT ( 'NONE', #11664 ) ;
#31904 = CARTESIAN_POINT ( 'NONE',  ( -11.61527771782809282, 108.2648137178985621, -4.622313124798832717 ) ) ;
#31905 = CARTESIAN_POINT ( 'NONE',  ( 19.68408634441911076, 5.407089921784862696, -1.246874999385527705 ) ) ;
#31906 = CARTESIAN_POINT ( 'NONE',  ( 36.86550044322413555, 3.604726614523238837, 159.7065721537869365 ) ) ;
#31907 = CARTESIAN_POINT ( 'NONE',  ( 15.24356964375000167, -3.323476615752272600, -2.015624999385490668 ) ) ;
#31908 = CARTESIAN_POINT ( 'NONE',  ( -12.53471296425189152, 61.97731371789854649, -2.311890736173453753 ) ) ;
#31909 = CARTESIAN_POINT ( 'NONE',  ( -1.909035429704832693E-15, 195.8375000000000057, -31.17691453623979214 ) ) ;
#31910 = ORIENTED_EDGE ( 'NONE', *, *, #24664, .T. ) ;
#31911 = VERTEX_POINT ( 'NONE', #32315 ) ;
#31912 = EDGE_LOOP ( 'NONE', ( #11067, #6325 ) ) ;
#31913 = CARTESIAN_POINT ( 'NONE',  ( 20.99999999999999645, 6.646953231504538984, -4.753124999385462068 ) ) ;
#31914 = DIRECTION ( 'NONE',  ( 0.000000000000000000, 0.000000000000000000, 1.000000000000000000 ) ) ;
#31915 = CARTESIAN_POINT ( 'NONE',  ( 15.24356964374999990, 245.6593750006145171, -3.323476615752268604 ) ) ;
#31916 = CARTESIAN_POINT ( 'NONE',  ( 2.660918448318279950, 42.89768628210143930, -12.46528703574805697 ) ) ;
#31917 = EDGE_CURVE ( 'NONE', #27522, #13344, #8459, .T. ) ;
#31918 = CARTESIAN_POINT ( 'NONE',  ( -52.76711230271182984, 216.4690446883607535, -1.857196546604089393 ) ) ;
#31919 = CARTESIAN_POINT ( 'NONE',  ( 7.405590309536301596, 215.0979036339257391, -3.170162721590327859 ) ) ;
#31920 = CARTESIAN_POINT ( 'NONE',  ( -33.96502896937850124, 213.8393509191290889, -2.350049139982142155 ) ) ;
#31921 = CARTESIAN_POINT ( 'NONE',  ( 30.81155773992399460, -6.928203230275506996, 162.1466181389027099 ) ) ;
#31922 = CARTESIAN_POINT ( 'NONE',  ( -7.228626920338836470, 109.1273137178985735, -10.49813415416005213 ) ) ;
#31923 = CARTESIAN_POINT ( 'NONE',  ( -65.04538769728823411, 211.3212981617418222, -4.469044688360751749 ) ) ;
#31924 = CARTESIAN_POINT ( 'NONE',  ( -45.25372103062157692, 218.5309553116391896, -2.162041339862839084 ) ) ;
#31925 = CARTESIAN_POINT ( 'NONE',  ( 23.87821517812500005, -4.985214923628404016, -3.253124999385486937 ) ) ;
#31926 = CARTESIAN_POINT ( 'NONE',  ( 10.56230152254410726, 0.000000000000000000, -5.400000000000043876 ) ) ;
#31927 = CARTESIAN_POINT ( 'NONE',  ( 3.257655550456945548, 77.50231371789855928, 15.46528703574811736 ) ) ;
#31928 = CARTESIAN_POINT ( 'NONE',  ( -57.12127896937850124, 218.5309553116392465, 2.162041339862725842 ) ) ;
#31929 = EDGE_LOOP ( 'NONE', ( #11315, #3884, #2794, #3066, #1524, #485, #439, #691, #17196, #12341, #5379, #28594, #16396, #14208, #22229, #13170, #20276, #28093, #21765, #17621, #23480, #530, #19396, #29535, #15468, #6080, #14981, #32094, #7848, #5380, #18263, #32996, #11854, #10828, #34817, #29397, #22319, #20436, #26084, #21302, #5418, #23851, #7826, #12321, #14268, #5897, #35568, #16086 ) ) ;
#31930 = CARTESIAN_POINT ( 'NONE',  ( 13.56230152254410548, 5.196152422706636465, -9.975000000000012079 ) ) ;
#31931 = CARTESIAN_POINT ( 'NONE',  ( -12.46528703574805697, 104.9976862821014691, -2.660918448318280838 ) ) ;
#31932 = CARTESIAN_POINT ( 'NONE',  ( -13.23911966647218463, 48.64768628210144641, 8.632099005475506459 ) ) ;
#31933 = CARTESIAN_POINT ( 'NONE',  ( 20.00041244883536606, 239.7473985345926053, -5.668978318349186196 ) ) ;
#31934 = CARTESIAN_POINT ( 'NONE',  ( 27.74986027194257332, -5.407089921784865361, 162.9697198055213789 ) ) ;
#31935 = CARTESIAN_POINT ( 'NONE',  ( 8.632099005475504683, 73.94768628210142936, 13.23911966647218996 ) ) ;
#31936 = LINE ( 'NONE', #5968, #9084 ) ;
#31937 = CARTESIAN_POINT ( 'NONE',  ( 13.44051670066911264, 5.407089921784856479, -8.315624999385541116 ) ) ;
#31938 = CARTESIAN_POINT ( 'NONE',  ( 38.04237167757703020, 114.1383727779938511, -2.499999999999996447 ) ) ;
#31939 = CARTESIAN_POINT ( 'NONE',  ( -55.54538769728823411, 211.8571965466039444, -6.469044688360768625 ) ) ;
#31940 = CARTESIAN_POINT ( 'NONE',  ( 26.99999999999999645, 241.3187500012290343, -3.464101615137755275 ) ) ;
#31941 = CARTESIAN_POINT ( 'NONE',  ( -4.622313124798576922, 32.83518628210143930, -11.61527771782819762 ) ) ;
#31942 = CARTESIAN_POINT ( 'NONE',  ( -27.00000000000000355, 195.9125000000000796, -15.58845726811989429 ) ) ;
#31943 = CARTESIAN_POINT ( 'NONE',  ( 26.99999999999952038, 3.464101615138031054, -3.731249998770935772 ) ) ;
#31944 = CARTESIAN_POINT ( 'NONE',  ( 8.843639120294245259, 140.4648137178985507, 3.474262827703527901 ) ) ;
#31945 = CARTESIAN_POINT ( 'NONE',  ( 26.75643035624999655, 246.9718750006145740, -3.323476615752271268 ) ) ;
#31946 = VERTEX_POINT ( 'NONE', #5975 ) ;
#31947 = CARTESIAN_POINT ( 'NONE',  ( 26.99999999999999645, -3.464101615137751278, -5.662499999999991651 ) ) ;
#31949 = CARTESIAN_POINT ( 'NONE',  ( 20.99999999999999645, 0.000000000000000000, -8.000000000000000000 ) ) ;
#31948 = PRODUCT_DEFINITION_SHAPE ( 'NONE', 'NONE',  #37508 ) ;
#31950 = CARTESIAN_POINT ( 'NONE',  ( 24.94224478302373527, 0.000000000000000000, 163.9023435342771506 ) ) ;
#31951 = CARTESIAN_POINT ( 'NONE',  ( 10.31873187879411269, 3.604726614523236616, -3.778124999385508609 ) ) ;
#31952 = CARTESIAN_POINT ( 'NONE',  ( 28.09467017918796472, 5.407089921784856479, 166.9109150798468306 ) ) ;
#31953 = CARTESIAN_POINT ( 'NONE',  ( 18.00000000000000355, 240.6250000000000000, 5.196152422706632912 ) ) ;
#31954 = EDGE_CURVE ( 'NONE', #26829, #1610, #15386, .T. ) ;
#31955 = CARTESIAN_POINT ( 'NONE',  ( 25.33444562538816669, 0.000000000000000000, 168.3852196756899957 ) ) ;
#31956 = CARTESIAN_POINT ( 'NONE',  ( 12.46528703574805874, 63.59768628210145636, 2.660918448318279950 ) ) ;
#31957 = ORIENTED_EDGE ( 'NONE', *, *, #5683, .F. ) ;
#31958 = ORIENTED_EDGE ( 'NONE', *, *, #30011, .T. ) ;
#31959 = PLANE ( 'NONE',  #16423 ) ;
#31960 = CARTESIAN_POINT ( 'NONE',  ( 36.56321044411491528, 7.347880794884117764E-16, 159.0460299011043901 ) ) ;
#31961 = CARTESIAN_POINT ( 'NONE',  ( -13.50000000000000533, 196.4375000012290400, -23.38268590217984411 ) ) ;
#31962 = CARTESIAN_POINT ( 'NONE',  ( 15.24356964375000167, -3.323476615752272600, -5.953124999385460470 ) ) ;
#31963 = PRODUCT_DEFINITION_CONTEXT ( 'detailed design', #12693, 'design' ) ;
#31964 = CARTESIAN_POINT ( 'NONE',  ( -2.908627838312453306, 32.07731371789855501, 15.53471296425188797 ) ) ;
#31965 = EDGE_CURVE ( 'NONE', #3146, #8675, #20479, .T. ) ;
#31966 = CARTESIAN_POINT ( 'NONE',  ( 24.00000000000000000, 249.2500000000000000, 5.196152422706629359 ) ) ;
#31967 = CARTESIAN_POINT ( 'NONE',  ( 19.00081571707366379, 239.8729221881839635, -5.492723647597353320 ) ) ;
#31968 = VECTOR ( 'NONE', #13836, 1000.000000000000000 ) ;
#31969 = CARTESIAN_POINT ( 'NONE',  ( -38.72247103062156981, 207.6499508600178387, 3.839350919129076445 ) ) ;
#31970 = CARTESIAN_POINT ( 'NONE',  ( 2.999999999999997335, 244.5000000000000000, -11.00000000000000000 ) ) ;
#31971 = CARTESIAN_POINT ( 'NONE',  ( 37.30839204460733782, 7.347880794884117764E-16, 167.5634945697888440 ) ) ;
#31972 = CARTESIAN_POINT ( 'NONE',  ( 3.796722387233182339, 22.01481371789855501, 8.710071997420207879 ) ) ;
#31973 = CARTESIAN_POINT ( 'NONE',  ( -61.28497103062156981, 204.4285982733020148, -3.350049139982115509 ) ) ;
#31974 = CARTESIAN_POINT ( 'NONE',  ( -44.25669563604517265, 209.8844732041981729, -8.500000000000003553 ) ) ;
#31975 =( LENGTH_UNIT ( ) NAMED_UNIT ( * ) SI_UNIT ( .MILLI., .METRE. ) );
#31976 = CYLINDRICAL_SURFACE ( 'NONE', #22796, 28.99999999999999645 ) ;
#31977 = CARTESIAN_POINT ( 'NONE',  ( 27.24356964375000345, 196.0343750006145456, -3.336375036156643733E-15 ) ) ;
#31978 = CARTESIAN_POINT ( 'NONE',  ( 8.927990412390371944, 132.1273137178985735, 13.04141134922778811 ) ) ;
#31979 = VERTEX_POINT ( 'NONE', #20029 ) ;
#31980 = CARTESIAN_POINT ( 'NONE',  ( 0.1745138560725515708, 51.81018628210144783, -12.50000000000000355 ) ) ;
#31981 = CARTESIAN_POINT ( 'NONE',  ( 13.56230152254411614, -5.196152422706632912, -9.712499998771024323 ) ) ;
#31982 = DIRECTION ( 'NONE',  ( -0.000000000000000000, 0.000000000000000000, 1.000000000000000000 ) ) ;
#31983 = AXIS2_PLACEMENT_3D ( 'NONE', #32683, #1594, #26811 ) ;
#31984 = CARTESIAN_POINT ( 'NONE',  ( 24.44548853280170775, -3.604726614523240613, 161.0190418602530258 ) ) ;
#31985 = CARTESIAN_POINT ( 'NONE',  ( 15.00000000000000000, 3.464101615137752166, -1.781249998770938925 ) ) ;
#31986 = CARTESIAN_POINT ( 'NONE',  ( 19.68408634441911076, 5.407089921784862696, -8.446874999385538985 ) ) ;
#31987 = CARTESIAN_POINT ( 'NONE',  ( 7.954856959092191815, 64.17268628210143788, 5.529263428287477744 ) ) ;
#31988 = DIRECTION ( 'NONE',  ( -0.000000000000000000, 1.000000000000000000, -0.000000000000000000 ) ) ;
#31989 = DIRECTION ( 'NONE',  ( 0.000000000000000000, 0.000000000000000000, -1.000000000000000000 ) ) ;
#31990 = CARTESIAN_POINT ( 'NONE',  ( 6.932735513423970097, 92.34768628210144925, 10.69584247140445044 ) ) ;
#31991 = CARTESIAN_POINT ( 'NONE',  ( 3.253724281355069334E-15, 199.5500000012290513, -27.00000000000000000 ) ) ;
#31992 = CARTESIAN_POINT ( 'NONE',  ( -26.99999999999999645, 195.0875000000000341, 15.58845726811991561 ) ) ;
#31993 = VERTEX_POINT ( 'NONE', #14701 ) ;
#31994 = CARTESIAN_POINT ( 'NONE',  ( 24.59583218904140978, 3.604726614523236616, 162.7374777144612494 ) ) ;
#31995 = CARTESIAN_POINT ( 'NONE',  ( 23.87821517812499650, 4.985214923628404904, -8.390624999385476457 ) ) ;
#31996 = DIRECTION ( 'NONE',  ( -0.000000000000000000, 1.000000000000000000, -0.000000000000000000 ) ) ;
#31997 = CARTESIAN_POINT ( 'NONE',  ( 24.90469035240339934, 3.604726614523240613, 166.2677426758239108 ) ) ;
#31998 = CARTESIAN_POINT ( 'NONE',  ( 33.92433876750752830, 5.196152422706637353, 163.3047283542161381 ) ) ;
#31999 = CARTESIAN_POINT ( 'NONE',  ( 15.00000000000000178, 248.2375000000000114, 3.464101615137757051 ) ) ;
#32000 = CARTESIAN_POINT ( 'NONE',  ( 27.24356964374999279, 199.6156250006145285, -15.72908226750539207 ) ) ;
#32001 = CARTESIAN_POINT ( 'NONE',  ( 12.53471296425189330, 112.5773137178985621, 2.311890736173451977 ) ) ;
#32002 = CARTESIAN_POINT ( 'NONE',  ( -11.48171059495397373, 123.6851862821014549, -4.944772684328680334 ) ) ;
#32004 = EDGE_LOOP ( 'NONE', ( #26975, #7260, #28593, #6449 ) ) ;
#32003 = VERTEX_POINT ( 'NONE', #20402 ) ;
#32005 = CARTESIAN_POINT ( 'NONE',  ( 27.24356964374999635, 197.8156250006145171, -15.72908226750539029 ) ) ;
#32006 = CARTESIAN_POINT ( 'NONE',  ( 18.12178482187500350, 242.6218750006145228, 4.985214923628407568 ) ) ;
#32007 = CARTESIAN_POINT ( 'NONE',  ( 14.25334919248795451, 93.31481371789855928, -6.092822981423661410 ) ) ;
#32008 = CARTESIAN_POINT ( 'NONE',  ( 15.24356964374999990, 3.323476615752268604, -3.440624999385503813 ) ) ;
#32009 = CARTESIAN_POINT ( 'NONE',  ( 18.12178482187500350, 247.6843750006145228, 4.985214923628407568 ) ) ;
#32010 = CARTESIAN_POINT ( 'NONE',  ( -27.00000000000000355, 196.5125000012290570, 0.000000000000000000 ) ) ;
#32011 = CARTESIAN_POINT ( 'NONE',  ( -8.152565276336593669, 80.95231371789854791, -5.233372021372610483 ) ) ;
#32012 = CARTESIAN_POINT ( 'NONE',  ( 22.80587116629410716, 3.604726614523238837, -5.278124999385515714 ) ) ;
#32013 = CARTESIAN_POINT ( 'NONE',  ( 23.87821517812499650, 242.8468750006145171, -4.985214923628404904 ) ) ;
#32014 = CARTESIAN_POINT ( 'NONE',  ( 0.1745138560722779009, 40.98981371789854933, 12.50000000000000355 ) ) ;
#32015 = DIRECTION ( 'NONE',  ( 0.000000000000000000, 1.000000000000000000, 0.000000000000000000 ) ) ;
#32016 = CARTESIAN_POINT ( 'NONE',  ( -0.1745138560725500443, 93.21018628210146062, 12.50000000000000355 ) ) ;
#32017 = CARTESIAN_POINT ( 'NONE',  ( 16.56230152254411081, 6.928203230275506996, -4.499999998770991105 ) ) ;
#32018 = CARTESIAN_POINT ( 'NONE',  ( -64.45163769728823411, 213.9548777149308592, -2.149950860017830756 ) ) ;
#32019 = CARTESIAN_POINT ( 'NONE',  ( 20.99999999999999645, 6.928203230275506996, -7.256249998770945453 ) ) ;
#32020 = DIRECTION ( 'NONE',  ( 0.000000000000000000, 0.000000000000000000, -1.000000000000000000 ) ) ;
#32021 = CARTESIAN_POINT ( 'NONE',  ( -2.908627838312119351, 106.7226862821014635, -15.53471296425195369 ) ) ;
#32022 = CARTESIAN_POINT ( 'NONE',  ( -4.622313124798576922, 23.63518628210144357, -11.61527771782819762 ) ) ;
#32023 = LINE ( 'NONE', #5682, #14010 ) ;
#32024 = DIRECTION ( 'NONE',  ( 6.123233995736766036E-17, -1.000000000000000000, 0.000000000000000000 ) ) ;
#32025 = CARTESIAN_POINT ( 'NONE',  ( -3.474262827703337830, 124.8351862821014748, -8.843639120294326972 ) ) ;
#32026 = CYLINDRICAL_SURFACE ( 'NONE', #27066, 3.999999999999996447 ) ;
#32027 = EDGE_CURVE ( 'NONE', #8056, #2746, #19280, .T. ) ;
#32028 = CARTESIAN_POINT ( 'NONE',  ( 5.778771075727756162E-15, 196.8218750006145399, 31.45816453501075927 ) ) ;
#32029 = CARTESIAN_POINT ( 'NONE',  ( 26.75643035624999655, 242.7343750006145342, 3.323476615752267715 ) ) ;
#32030 = ORIENTED_EDGE ( 'NONE', *, *, #32495, .T. ) ;
#32031 = CARTESIAN_POINT ( 'NONE',  ( 25.22662187717753568, 0.000000000000000000, 169.9474368419002985 ) ) ;
#32032 = CARTESIAN_POINT ( 'NONE',  ( -9.534712964251941258, 58.42268628210145209, 1.715153634034234154 ) ) ;
#32033 = DIRECTION ( 'NONE',  ( 0.9961946980917462113, 0.000000000000000000, -0.08715574274765178209 ) ) ;
#32034 = DIRECTION ( 'NONE',  ( 1.000000000000000000, 0.000000000000000000, 0.000000000000000000 ) ) ;
#32035 = PLANE ( 'NONE',  #337 ) ;
#32036 = CARTESIAN_POINT ( 'NONE',  ( 27.24356964375000345, 195.5843750006145285, -3.336375036156643733E-15 ) ) ;
#32037 = DIRECTION ( 'NONE',  ( -0.000000000000000000, -0.000000000000000000, -1.000000000000000000 ) ) ;
#32038 = DIRECTION ( 'NONE',  ( -0.000000000000000000, -0.000000000000000000, 1.000000000000000000 ) ) ;
#32039 = CARTESIAN_POINT ( 'NONE',  ( 7.954856959092311719, 47.02731371789855075, -5.529263428287300108 ) ) ;
#32040 = FACE_BOUND ( 'NONE', #31450, .T. ) ;
#32041 = VERTEX_POINT ( 'NONE', #17927 ) ;
#32042 = ORIENTED_EDGE ( 'NONE', *, *, #9197, .T. ) ;
#32043 = CARTESIAN_POINT ( 'NONE',  ( 26.99999999999999645, 239.8937500012290229, 3.464101615137751278 ) ) ;
#32044 = CARTESIAN_POINT ( 'NONE',  ( 12.46528703574811558, 38.40231371789855075, -2.660918448318005947 ) ) ;
#32045 = CARTESIAN_POINT ( 'NONE',  ( 13.44051670066911441, -5.407089921784865361, -9.121874999385520155 ) ) ;
#32046 = CARTESIAN_POINT ( 'NONE',  ( 18.12178482187499640, 4.985214923628404904, -10.22812499938549635 ) ) ;
#32047 = CARTESIAN_POINT ( 'NONE',  ( -4.944772684328424539, 17.41481371789854649, -11.48171059495408031 ) ) ;
#32048 = EDGE_CURVE ( 'NONE', #35189, #31630, #7505, .T. ) ;
#32049 = CARTESIAN_POINT ( 'NONE',  ( 10.56230152254410726, 0.000000000000000000, -1.350000000000045608 ) ) ;
#32050 = EDGE_LOOP ( 'NONE', ( #20648, #35751, #22095, #19264 ) ) ;
#32051 = CARTESIAN_POINT ( 'NONE',  ( 10.31873187879411091, -3.604726614523244610, -2.859374999385534633 ) ) ;
#32052 = ORIENTED_EDGE ( 'NONE', *, *, #21473, .T. ) ;
#32053 = CARTESIAN_POINT ( 'NONE',  ( 13.62178482187499640, 198.7531250006145456, -23.59362340125807123 ) ) ;
#32054 = CARTESIAN_POINT ( 'NONE',  ( 24.98966720158236043, -3.604726614523244610, 167.2390325064633885 ) ) ;
#32055 = EDGE_CURVE ( 'NONE', #5932, #19565, #16836, .T. ) ;
#32056 =( REPRESENTATION_RELATIONSHIP ('NONE','NONE', #4304, #35512 ) REPRESENTATION_RELATIONSHIP_WITH_TRANSFORMATION ( #877 )SHAPE_REPRESENTATION_RELATIONSHIP( ) );
#32057 = CARTESIAN_POINT ( 'NONE',  ( -31.59002896937850124, 204.4285982733020433, 3.350049139982171020 ) ) ;
#32058 = CARTESIAN_POINT ( 'NONE',  ( 15.00000000000000000, 245.5187500012290513, -3.464101615137752610 ) ) ;
#32059 = FACE_BOUND ( 'NONE', #28471, .T. ) ;
#32060 = CARTESIAN_POINT ( 'NONE',  ( -64.24627896937850835, 205.4690446883607535, -1.090244570138286351 ) ) ;
#32061 =( BOUNDED_CURVE ( )  B_SPLINE_CURVE ( 2, ( #28579, #2617, #14193, #31799, #5645, #17415, #23099, #31617, #13640 ),
 .UNSPECIFIED., .F., .F. ) 
 B_SPLINE_CURVE_WITH_KNOTS ( ( 3, 2, 2, 2, 3 ),
 ( 0.01086956521739129711, 0.01449275362318840597, 0.02173913043478260809, 0.02898550724637681195, 0.03260869565217391908 ),
 .UNSPECIFIED. ) 
 CURVE ( )  GEOMETRIC_REPRESENTATION_ITEM ( )  RATIONAL_B_SPLINE_CURVE ( ( 0.9330127018922192983, 0.9330127018922191873, 1.000000000000000000, 0.8660254037844387076, 1.000000000000000000, 0.8660254037844387076, 1.000000000000000000, 0.9330127018922191873, 0.9330127018922192983 ) ) 
 REPRESENTATION_ITEM ( '' )  );
#32062 = CARTESIAN_POINT ( 'NONE',  ( 15.02283181144952628, 7.347880794884122694E-16, 50.52293445648592751 ) ) ;
#32063 = CARTESIAN_POINT ( 'NONE',  ( 31.29935753756119965, -7.209453229046475009, 167.7221953391727709 ) ) ;
#32064 = ORIENTED_EDGE ( 'NONE', *, *, #19616, .T. ) ;
#32065 = CARTESIAN_POINT ( 'NONE',  ( 37.29531868308838938, -3.464101615137579415, 167.4140653638507388 ) ) ;
#32066 = AXIS2_PLACEMENT_3D ( 'NONE', #22995, #14646, #23366 ) ;
#32067 = CARTESIAN_POINT ( 'NONE',  ( 0.1745138560722461762, 22.58981371789854364, 15.50000000000000533 ) ) ;
#32068 = CARTESIAN_POINT ( 'NONE',  ( -61.28497103062156981, 202.6965474657331185, -4.350049139982091084 ) ) ;
#32069 = CARTESIAN_POINT ( 'NONE',  ( -8.152565276336710909, 131.4476862821014436, 5.233372021372435512 ) ) ;
#32070 = CARTESIAN_POINT ( 'NONE',  ( -2.311890736173176641, 42.32268628210145067, -12.53471296425194836 ) ) ;
#32071 = CARTESIAN_POINT ( 'NONE',  ( 19.56230152254412502, 5.196152422706637353, -4.650000000000070521 ) ) ;
#32072 = ORIENTED_EDGE ( 'NONE', *, *, #19573, .F. ) ;
#32073 = CARTESIAN_POINT ( 'NONE',  ( -43.27455436395489841, 205.1570982666397640, 4.673758765035199048 ) ) ;
#32074 = CARTESIAN_POINT ( 'NONE',  ( 15.00000000000000000, 242.3500000000000227, 0.000000000000000000 ) ) ;
#32075 = CARTESIAN_POINT ( 'NONE',  ( 9.500000000000005329, 17.31018628210144428, 0.1745138560725188748 ) ) ;
#32076 = VECTOR ( 'NONE', #20161, 1000.000000000000000 ) ;
#32077 = CARTESIAN_POINT ( 'NONE',  ( -13.62178482187500528, 196.1843750006145228, -23.59362340125807123 ) ) ;
#32078 = DIRECTION ( 'NONE',  ( 0.000000000000000000, 1.000000000000000000, 0.000000000000000000 ) ) ;
#32079 = FACE_OUTER_BOUND ( 'NONE', #1820, .T. ) ;
#32080 = DIRECTION ( 'NONE',  ( 0.000000000000000000, 0.000000000000000000, 1.000000000000000000 ) ) ;
#32081 =( BOUNDED_CURVE ( )  B_SPLINE_CURVE ( 2, ( #8964, #26577, #23560, #31892, #22817, #2704, #17690, #34365, #28856 ),
 .UNSPECIFIED., .F., .F. ) 
 B_SPLINE_CURVE_WITH_KNOTS ( ( 3, 2, 2, 2, 3 ),
 ( 0.2291666666666666574, 0.2361111111111111049, 0.2500000000000000000, 0.2638888888888888951, 0.2708333333333333703 ),
 .UNSPECIFIED. ) 
 CURVE ( )  GEOMETRIC_REPRESENTATION_ITEM ( )  RATIONAL_B_SPLINE_CURVE ( ( 0.9330127018922194093, 0.9330127018922194093, 1.000000000000000000, 0.8660254037844387076, 1.000000000000000000, 0.8660254037844387076, 1.000000000000000000, 0.9330127018922190762, 0.9330127018922194093 ) ) 
 REPRESENTATION_ITEM ( '' )  );
#32082 = CARTESIAN_POINT ( 'NONE',  ( 21.00000000000000000, 244.7968750006145626, -6.646953231504538984 ) ) ;
#32083 = CARTESIAN_POINT ( 'NONE',  ( 9.465287035748106703, 102.8023137178985422, -2.064181346179063237 ) ) ;
#32084 = DIRECTION ( 'NONE',  ( -0.000000000000000000, -1.000000000000000000, -0.000000000000000000 ) ) ;
#32085 = VERTEX_POINT ( 'NONE', #20210 ) ;
#32086 = CARTESIAN_POINT ( 'NONE',  ( -54.75372103062154849, 216.5309553116391612, -1.626142955000564383 ) ) ;
#32087 = CARTESIAN_POINT ( 'NONE',  ( 18.00000000000000000, 246.8312500012290513, -5.196152422706630247 ) ) ;
#32088 = CARTESIAN_POINT ( 'NONE',  ( 10.49813415416005213, 102.2273137178985536, -7.228626920338837358 ) ) ;
#32089 = EDGE_CURVE ( 'NONE', #26752, #32409, #90, .T. ) ;
#32090 = CARTESIAN_POINT ( 'NONE',  ( 16.56230152254411436, 7.209453229046482114, -2.559374999385494842 ) ) ;
#32091 = CARTESIAN_POINT ( 'NONE',  ( 15.24356964375000167, -3.323476615752272600, -2.915624999385482141 ) ) ;
#32092 = CARTESIAN_POINT ( 'NONE',  ( -8.715434833792127023, 69.73981371789855643, 8.962234695871568846 ) ) ;
#32093 = CARTESIAN_POINT ( 'NONE',  ( -13.62178482187500528, 198.8843750006145399, -23.59362340125807123 ) ) ;
#32094 = ORIENTED_EDGE ( 'NONE', *, *, #32992, .T. ) ;
#32095 = CIRCLE ( 'NONE', #25440, 1.500000000000001332 ) ;
#32096 = ORIENTED_EDGE ( 'NONE', *, *, #20765, .F. ) ;
#32097 = CARTESIAN_POINT ( 'NONE',  ( 15.24356964374999990, 3.323476615752268604, -6.028124999385455318 ) ) ;
#32098 = CARTESIAN_POINT ( 'NONE',  ( 10.56230152254339494, 3.464101615137343160, -0.9375000000000115463 ) ) ;
#32099 = CARTESIAN_POINT ( 'NONE',  ( 23.87821517812499650, 245.5468750006145058, -4.985214923628404904 ) ) ;
#32100 = ADVANCED_FACE ( 'NONE', ( #8642 ), #31759, .F. ) ;
#32101 = CARTESIAN_POINT ( 'NONE',  ( -4.622313124798576922, 42.03518628210144215, -11.61527771782819762 ) ) ;
#32102 = CARTESIAN_POINT ( 'NONE',  ( -47.02752896937850124, 213.3500491399821613, 5.571401726697954970 ) ) ;
#32103 = CARTESIAN_POINT ( 'NONE',  ( -35.35044563604517265, 206.6211998817775566, -3.209657149897419348 ) ) ;
#32104 = CARTESIAN_POINT ( 'NONE',  ( 36.75604252494409963, -3.464101615137751278, 161.2501106706323810 ) ) ;
#32105 = CARTESIAN_POINT ( 'NONE',  ( -10.69584247140429412, 108.5523137178985564, -6.932735513424201024 ) ) ;
#32106 = CARTESIAN_POINT ( 'NONE',  ( -61.68080436395489841, 205.4999999999999716, -0.1155267958017894420 ) ) ;
#32107 = CARTESIAN_POINT ( 'NONE',  ( -35.35788769728823411, 218.4690446883607535, 2.393094931466250408 ) ) ;
#32108 = EDGE_CURVE ( 'NONE', #21071, #37055, #30420, .T. ) ;
#32109 = CARTESIAN_POINT ( 'NONE',  ( 26.75643035624999655, -3.323476615752267271, -5.465624999385501503 ) ) ;
#32110 = CARTESIAN_POINT ( 'NONE',  ( 5.770363421894130873, 82.96481371789856496, -14.38691631536193860 ) ) ;
#32111 = CARTESIAN_POINT ( 'NONE',  ( -52.76711230271184405, 218.4690446883607535, -2.393094931466363651 ) ) ;
#32112 = EDGE_LOOP ( 'NONE', ( #18835, #29457, #25572, #1799 ) ) ;
#32113 = CARTESIAN_POINT ( 'NONE',  ( 24.00000000000000000, -5.196152422706629359, -0.6937499987709483396 ) ) ;
#32114 = CARTESIAN_POINT ( 'NONE',  ( -2.660918448318275509, 102.6976862821014720, 12.46528703574805874 ) ) ;
#32115 = CARTESIAN_POINT ( 'NONE',  ( -6.092822981423970496, 47.78518628210144215, 14.25334919248782661 ) ) ;
#32116 = CARTESIAN_POINT ( 'NONE',  ( -12.50000000000000355, 144.4898137178985564, 0.1745138560722786503 ) ) ;
#32117 = FACE_OUTER_BOUND ( 'NONE', #29056, .T. ) ;
#32118 = CIRCLE ( 'NONE', #28491, 5.999999999999998224 ) ;
#32119 = CARTESIAN_POINT ( 'NONE',  ( 0.1745138560725837118, 70.21018628210144641, -15.50000000000000533 ) ) ;
#32120 = CARTESIAN_POINT ( 'NONE',  ( -7.234628195640354420, 194.8049038117966916, 26.99999999999996803 ) ) ;
#32121 = ADVANCED_FACE ( 'NONE', ( #10135 ), #32688, .T. ) ;
#32122 = CARTESIAN_POINT ( 'NONE',  ( 19.68408634441910721, 5.407089921784857367, -7.940624999385553551 ) ) ;
#32123 = CARTESIAN_POINT ( 'NONE',  ( 15.00000000000000000, 0.000000000000000000, -4.049999999999998046 ) ) ;
#32124 = CARTESIAN_POINT ( 'NONE',  ( -44.26413769728823411, 213.1499508600178672, 5.686928522499718142 ) ) ;
#32125 = FACE_OUTER_BOUND ( 'NONE', #33270, .T. ) ;
#32126 = CARTESIAN_POINT ( 'NONE',  ( 10.49813415415989581, 36.57268628210145067, 7.228626920339068285 ) ) ;
#32127 = CARTESIAN_POINT ( 'NONE',  ( -27.00000000000000355, 195.0500000000000114, 0.000000000000000000 ) ) ;
#32128 = CARTESIAN_POINT ( 'NONE',  ( 9.500000000000005329, 8.110186282101443211, 0.1745138560725188748 ) ) ;
#32129 = CARTESIAN_POINT ( 'NONE',  ( 18.12178482187500350, 246.3343750006145285, 4.985214923628407568 ) ) ;
#32130 = ORIENTED_EDGE ( 'NONE', *, *, #21788, .F. ) ;
#32131 = CARTESIAN_POINT ( 'NONE',  ( 26.99999999999999645, 7.347880794884117764E-16, -7.874999999999992895 ) ) ;
#32132 = CARTESIAN_POINT ( 'NONE',  ( 15.00000000000000000, 249.6062500012290570, 0.000000000000000000 ) ) ;
#32133 = FACE_OUTER_BOUND ( 'NONE', #22094, .T. ) ;
#32134 = CARTESIAN_POINT ( 'NONE',  ( 13.44051670066911086, 5.407089921784856479, -5.165624999385554084 ) ) ;
#32135 = CARTESIAN_POINT ( 'NONE',  ( 24.91286120328598841, 0.000000000000000000, 166.3611359287700395 ) ) ;
#32136 = CARTESIAN_POINT ( 'NONE',  ( 21.00000000000000000, 241.3375000000000341, -6.928203230275506996 ) ) ;
#32137 = CARTESIAN_POINT ( 'NONE',  ( -12.83063518929827751, 216.5618201379890309, 4.786185431830589643 ) ) ;
#32138 = CARTESIAN_POINT ( 'NONE',  ( 4.944772684328679446, 61.58518628210145351, -11.48171059495397373 ) ) ;
#32139 = VERTEX_POINT ( 'NONE', #1034 ) ;
#32140 = ORIENTED_EDGE ( 'NONE', *, *, #27204, .F. ) ;
#32141 = DIRECTION ( 'NONE',  ( 0.000000000000000000, 0.000000000000000000, 1.000000000000000000 ) ) ;
#32142 = FACE_OUTER_BOUND ( 'NONE', #4205, .T. ) ;
#32143 = CARTESIAN_POINT ( 'NONE',  ( 15.00000000000000000, 248.2000000000000171, 0.000000000000000000 ) ) ;
#32144 = CARTESIAN_POINT ( 'NONE',  ( 18.12178482187500350, -4.985214923628407568, -5.465624999385465088 ) ) ;
#32145 = CARTESIAN_POINT ( 'NONE',  ( 2.908627838312458636, 27.47731371789854649, -15.53471296425188442 ) ) ;
#32146 = CARTESIAN_POINT ( 'NONE',  ( 22.56230152254410370, 7.347880794884117764E-16, -5.512499998771014376 ) ) ;
#32147 = CARTESIAN_POINT ( 'NONE',  ( 37.14497502684795904, 3.464101615138004409, 165.6956295096424583 ) ) ;
#32148 = VECTOR ( 'NONE', #13001, 1000.000000000000000 ) ;
#32149 = VECTOR ( 'NONE', #3777, 1000.000000000000000 ) ;
#32150 = CARTESIAN_POINT ( 'NONE',  ( -63.85044563604516554, 206.6211998817775566, -3.209657149897419348 ) ) ;
#32151 = FACE_OUTER_BOUND ( 'NONE', #1756, .T. ) ;
#32152 = CARTESIAN_POINT ( 'NONE',  ( 30.58849351077567036, -7.209453229046482114, 159.5969823328619555 ) ) ;
#32153 = CARTESIAN_POINT ( 'NONE',  ( -3.796722387233185003, 17.41481371789854649, -8.710071997420207879 ) ) ;
#32154 = CARTESIAN_POINT ( 'NONE',  ( -62.27455436395490551, 205.1570982666397356, 4.673758765035198159 ) ) ;
#32155 = CARTESIAN_POINT ( 'NONE',  ( -34.36086230271182984, 214.1499508600178387, -7.418979330068641964 ) ) ;
#32156 = CARTESIAN_POINT ( 'NONE',  ( 0.000000000000000000, 0.000000000000000000, 0.000000000000000000 ) ) ;
#32157 = CARTESIAN_POINT ( 'NONE',  ( 20.99999999999995381, 242.5187500012290513, 5.999999999999998224 ) ) ;
#32158 = CARTESIAN_POINT ( 'NONE',  ( -27.24356964374999635, 195.8468750006145171, 15.72908226750539384 ) ) ;
#32159 = CARTESIAN_POINT ( 'NONE',  ( -15.46528703574811736, 125.8023137178985706, 3.257655550456946436 ) ) ;
#32160 = CARTESIAN_POINT ( 'NONE',  ( -55.73586230271182984, 206.8500491399821328, 5.686928522499748340 ) ) ;
#32161 = EDGE_CURVE ( 'NONE', #1340, #34717, #36091, .T. ) ;
#32162 = VERTEX_POINT ( 'NONE', #18117 ) ;
#32163 = EDGE_CURVE ( 'NONE', #6034, #14163, #18498, .T. ) ;
#32164 = CARTESIAN_POINT ( 'NONE',  ( 10.69584247140445221, 53.24768628210144072, -6.932735513423970097 ) ) ;
#32165 = CARTESIAN_POINT ( 'NONE',  ( 37.27244030072370151, 3.464101615137892942, 167.1525642568259968 ) ) ;
#32166 = CARTESIAN_POINT ( 'NONE',  ( 22.38580703878232470, 5.599659159192138524, -8.000000000000000000 ) ) ;
#32167 = CARTESIAN_POINT ( 'NONE',  ( 37.60577953318700395, 3.604726614523243278, 168.1680008707037075 ) ) ;
#32168 = CARTESIAN_POINT ( 'NONE',  ( 26.99999999999999645, 3.464101615137755275, -1.931249998770958820 ) ) ;
#32169 = CARTESIAN_POINT ( 'NONE',  ( 10.31873187879410736, 3.604726614523240613, -8.334374999385541827 ) ) ;
#32170 = CARTESIAN_POINT ( 'NONE',  ( -66.62872103062154849, 203.4690446883607535, 1.626142955000567936 ) ) ;
#32171 = AXIS2_PLACEMENT_3D ( 'NONE', #9397, #660, #34792 ) ;
#32172 = CARTESIAN_POINT ( 'NONE',  ( 16.56230152254411081, -7.209453229046475009, -1.828124999385505989 ) ) ;
#32173 = CARTESIAN_POINT ( 'NONE',  ( 0.1745138560725194299, 61.01018628210145067, -9.500000000000005329 ) ) ;
#32174 = LINE ( 'NONE', #31615, #7994 ) ;
#32175 = DIRECTION ( 'NONE',  ( -0.000000000000000000, -0.000000000000000000, 1.000000000000000000 ) ) ;
#32176 = EDGE_CURVE ( 'NONE', #31726, #33950, #5671, .T. ) ;
#32177 = CARTESIAN_POINT ( 'NONE',  ( 2.660918448318279950, 98.09768628210146346, -12.46528703574805697 ) ) ;
#32178 = CARTESIAN_POINT ( 'NONE',  ( 13.50000000000001421, 199.7000000000000171, 23.38268590217984055 ) ) ;
#32179 = LINE ( 'NONE', #3367, #30507 ) ;
#32180 = ORIENTED_EDGE ( 'NONE', *, *, #13992, .F. ) ;
#32181 = CARTESIAN_POINT ( 'NONE',  ( 29.49486714975617474, 6.148716665048037378, 159.5363409456820136 ) ) ;
#32182 = AXIS2_PLACEMENT_3D ( 'NONE', #31569, #5591, #13962 ) ;
#32183 = PRODUCT_DEFINITION ( 'UNKNOWN', '', #20845, #12282 ) ;
#32184 = CARTESIAN_POINT ( 'NONE',  ( 26.75643035624999655, 3.323476615752271712, -6.628124999385471838 ) ) ;
#32185 = CARTESIAN_POINT ( 'NONE',  ( 28.22824784931821895, 5.196152422706636465, 167.0403907120479232 ) ) ;
#32186 = CARTESIAN_POINT ( 'NONE',  ( 24.91122703310947628, -3.604726614523244610, 166.3424572781808024 ) ) ;
#32187 = CARTESIAN_POINT ( 'NONE',  ( 36.90965452142972225, 3.464101615137759271, 163.0059038247947285 ) ) ;
#32188 = CARTESIAN_POINT ( 'NONE',  ( 20.99999999999999645, 0.000000000000000000, -8.000000000000000000 ) ) ;
#32189 = CARTESIAN_POINT ( 'NONE',  ( 15.00000000000000000, 249.0999999999999943, 0.000000000000000000 ) ) ;
#32190 = CARTESIAN_POINT ( 'NONE',  ( -27.24356964375000345, 195.3031250006145285, 0.000000000000000000 ) ) ;
#32191 = CARTESIAN_POINT ( 'NONE',  ( 7.228626920338837358, 104.5273137178985650, 10.49813415416005036 ) ) ;
#32192 = CARTESIAN_POINT ( 'NONE',  ( -2.660918448318275509, 130.2976862821014379, 12.46528703574805874 ) ) ;
#32194 = ORIENTED_EDGE ( 'NONE', *, *, #22111, .F. ) ;
#32193 = ORIENTED_EDGE ( 'NONE', *, *, #32108, .F. ) ;
#32195 = CARTESIAN_POINT ( 'NONE',  ( 27.24356964375000700, 195.4906250006145001, 15.72908226750537075 ) ) ;
#32196 = CARTESIAN_POINT ( 'NONE',  ( 21.00000000000000000, 242.6593750006145171, 6.646953231504538984 ) ) ;
#32197 = CARTESIAN_POINT ( 'NONE',  ( -8.632099005475794229, 87.85231371789855359, 13.23911966647199812 ) ) ;
#32198 = CARTESIAN_POINT ( 'NONE',  ( 15.24356964374999990, 3.323476615752268604, -4.340624999385463312 ) ) ;
#32199 = CARTESIAN_POINT ( 'NONE',  ( 21.00000000000000000, 248.6218750006145228, 6.646953231504538984 ) ) ;
#32200 = CARTESIAN_POINT ( 'NONE',  ( -9.500000000000005329, 104.7101862821014606, -0.1745138560725176813 ) ) ;
#32201 = AXIS2_PLACEMENT_3D ( 'NONE', #2803, #20631, #8504 ) ;
#32202 = CARTESIAN_POINT ( 'NONE',  ( -1.909035429704832693E-15, 195.5000000012290400, -31.17691453623979214 ) ) ;
#32203 = CARTESIAN_POINT ( 'NONE',  ( 0.1745138560723095977, 68.58981371789855075, 9.500000000000005329 ) ) ;
#32204 = CARTESIAN_POINT ( 'NONE',  ( 10.31873187879411269, -3.604726614523240613, -5.503124999385529570 ) ) ;
#32205 = CARTESIAN_POINT ( 'NONE',  ( 23.87821517812500005, 241.3468750006145171, 4.985214923628404016 ) ) ;
#32206 = CARTESIAN_POINT ( 'NONE',  ( 4.622313124798831829, 55.36481371789855643, -11.61527771782809282 ) ) ;
#32207 = CARTESIAN_POINT ( 'NONE',  ( 24.90629303914081305, -3.464101615138032830, 163.4914132213142750 ) ) ;
#32208 = CARTESIAN_POINT ( 'NONE',  ( 7.228626920339068285, 98.67268628210145209, -10.49813415415989581 ) ) ;
#32209 = CARTESIAN_POINT ( 'NONE',  ( 10.56230152254411259, 3.464101615137752166, -5.324999998771021481 ) ) ;
#32210 = CARTESIAN_POINT ( 'NONE',  ( -67.61830436395490551, 209.8844732041982297, 4.499999999999996447 ) ) ;
#32211 = CARTESIAN_POINT ( 'NONE',  ( 8.715434833791931624, 138.0601862821014549, 8.962234695871760692 ) ) ;
#32212 = CARTESIAN_POINT ( 'NONE',  ( 30.70370250816666058, 6.928203230275514990, 160.9138271987898463 ) ) ;
#32213 = CARTESIAN_POINT ( 'NONE',  ( 15.50000000000000533, 90.91018628210146346, 0.1745138560725827404 ) ) ;
#32214 = CARTESIAN_POINT ( 'NONE',  ( 26.99999999999999645, 7.347880794884117764E-16, -0.6750000000000089262 ) ) ;
#32215 = DIRECTION ( 'NONE',  ( 0.9961946980917462113, 0.000000000000000000, -0.08715574274765118534 ) ) ;
#32216 = CARTESIAN_POINT ( 'NONE',  ( 24.00000000000000000, -5.196152422706629359, -5.643749998770958065 ) ) ;
#32217 = CARTESIAN_POINT ( 'NONE',  ( 5.529263428287477744, 107.8726862821014549, -7.954856959092191815 ) ) ;
#32218 = CARTESIAN_POINT ( 'NONE',  ( 26.99999999999999645, 199.0250000012290172, -15.58845726811990495 ) ) ;
#32219 = CARTESIAN_POINT ( 'NONE',  ( 15.50000000000000533, 8.110186282101443211, 0.1745138560725827404 ) ) ;
#32220 = CARTESIAN_POINT ( 'NONE',  ( 27.24356964375000345, 195.5843750006145285, -3.336375036156643733E-15 ) ) ;
#32221 = CARTESIAN_POINT ( 'NONE',  ( 18.12178482187500350, 241.7218750006145171, 4.985214923628407568 ) ) ;
#32222 = ORIENTED_EDGE ( 'NONE', *, *, #21463, .T. ) ;
#32223 = CARTESIAN_POINT ( 'NONE',  ( 31.18169728485186454, -7.209453229046475009, 166.3773324967489202 ) ) ;
#32224 = CARTESIAN_POINT ( 'NONE',  ( 18.12178482187499640, 4.985214923628404904, -1.565624999385478722 ) ) ;
#32225 = CARTESIAN_POINT ( 'NONE',  ( 26.99999999999999645, 241.7125000000000057, -3.464101615137755275 ) ) ;
#32226 = CARTESIAN_POINT ( 'NONE',  ( 2.999999999999997335, 244.5000000000000000, 5.000000000000000000 ) ) ;
#32227 = DIRECTION ( 'NONE',  ( -0.1155267958017759666, -0.9933043639548629899, 2.756973438308332598E-14 ) ) ;
#32228 = CARTESIAN_POINT ( 'NONE',  ( -4.521054380870901390, 195.0000000000000853, 26.88021455572233620 ) ) ;
#32229 = CARTESIAN_POINT ( 'NONE',  ( 26.97716818855048260, 0.000000000000000000, 49.47706554351410801 ) ) ;
#32230 = CARTESIAN_POINT ( 'NONE',  ( -9.500000000000005329, 34.08981371789853654, 0.1745138560723101806 ) ) ;
#32231 = DIRECTION ( 'NONE',  ( 0.000000000000000000, 1.000000000000000000, -2.710505431213758127E-16 ) ) ;
#32232 = ORIENTED_EDGE ( 'NONE', *, *, #6847, .T. ) ;
#32233 = CARTESIAN_POINT ( 'NONE',  ( 26.75643035624999655, 249.5593750006145228, -3.323476615752271712 ) ) ;
#32234 = CARTESIAN_POINT ( 'NONE',  ( -11.48171059495408208, 51.91481371789855359, 4.944772684328421875 ) ) ;
#32235 = CARTESIAN_POINT ( 'NONE',  ( 18.12178482187500350, -4.985214923628407568, -8.278124999385488181 ) ) ;
#32236 = CARTESIAN_POINT ( 'NONE',  ( -8.962234695871565293, 16.83981371789855430, -8.715434833792128799 ) ) ;
#32237 = CARTESIAN_POINT ( 'NONE',  ( -6.000000000000000888, -20.00000000000000000, -19.99999999999999289 ) ) ;
#32238 = EDGE_LOOP ( 'NONE', ( #6667, #11648, #19467, #2726 ) ) ;
#32239 = CARTESIAN_POINT ( 'NONE',  ( 22.80587116629411781, -3.604726614523238837, -2.709374999385514737 ) ) ;
#32240 = EDGE_LOOP ( 'NONE', ( #6082, #8383, #22874, #288 ) ) ;
#32241 = CARTESIAN_POINT ( 'NONE',  ( 27.24356964375000700, 198.6406250006145058, 15.72908226750537075 ) ) ;
#32242 = CARTESIAN_POINT ( 'NONE',  ( 34.25074851857407765, -5.407089921784861808, 165.6382847571695436 ) ) ;
#32243 = CARTESIAN_POINT ( 'NONE',  ( -35.54836230271183695, 204.3130714775002446, -3.149950860017828091 ) ) ;
#32244 = CARTESIAN_POINT ( 'NONE',  ( 26.75643035624999655, 249.0718750006145115, -7.049594010296217766E-16 ) ) ;
#32245 = DIRECTION ( 'NONE',  ( -0.000000000000000000, -1.000000000000000000, -0.000000000000000000 ) ) ;
#32246 = CARTESIAN_POINT ( 'NONE',  ( -56.92336230271183695, 213.9548777149308023, 2.149950860017852960 ) ) ;
#32247 = CARTESIAN_POINT ( 'NONE',  ( -35.55580436395490551, 216.5000000000000000, 0.1155267958017343610 ) ) ;
#32248 = CARTESIAN_POINT ( 'NONE',  ( 31.37779770603408380, -7.209453229046475009, 168.6187705674553285 ) ) ;
#32249 = ORIENTED_EDGE ( 'NONE', *, *, #23035, .F. ) ;
#32250 = CARTESIAN_POINT ( 'NONE',  ( 26.99999999999999645, 248.0312500012290400, -7.347880794884117764E-16 ) ) ;
#32251 = CARTESIAN_POINT ( 'NONE',  ( -8.927990412390661490, 140.0726862821014151, 13.04141134922759804 ) ) ;
#32252 = CARTESIAN_POINT ( 'NONE',  ( -61.48288769728824121, 201.5309553116392181, -2.393094931466246855 ) ) ;
#32253 = PRODUCT_DEFINITION_SHAPE ( 'NONE', 'NONE',  #7423 ) ;
#32254 = CARTESIAN_POINT ( 'NONE',  ( 2.064181346179272847, 125.6976862821014578, -9.465287035748065847 ) ) ;
#32255 = CARTESIAN_POINT ( 'NONE',  ( 2.311890736173175753, 28.52268628210144641, 12.53471296425194836 ) ) ;
#32256 = CARTESIAN_POINT ( 'NONE',  ( 19.56230152254412502, 5.196152422706637353, -5.550000000000054889 ) ) ;
#32257 = VERTEX_POINT ( 'NONE', #845 ) ;
#32258 = CARTESIAN_POINT ( 'NONE',  ( -40.50372103062156981, 216.5309553116392181, -1.626142955000564383 ) ) ;
#32259 = CARTESIAN_POINT ( 'NONE',  ( 6.092822981423978490, 125.9851862821014521, -14.25334919248782306 ) ) ;
#32260 = PRESENTATION_LAYER_ASSIGNMENT (  '', '', ( #11092 ) ) ;
#32261 = CARTESIAN_POINT ( 'NONE',  ( 8.152565276336714462, 16.44768628210144001, -5.233372021372432847 ) ) ;
#32262 = CARTESIAN_POINT ( 'NONE',  ( 27.24356964375000345, 195.1343750006145399, -3.336375036156643733E-15 ) ) ;
#32263 = CARTESIAN_POINT ( 'NONE',  ( 27.00000000000000355, 195.8375000012290457, -3.306546357697854128E-15 ) ) ;
#32264 = CARTESIAN_POINT ( 'NONE',  ( 21.00000000000000355, 0.000000000000000000, 50.00000000000001421 ) ) ;
#32265 = CARTESIAN_POINT ( 'NONE',  ( 26.99999999999999289, 0.000000000000000000, -8.000000000000000000 ) ) ;
#32266 = CARTESIAN_POINT ( 'NONE',  ( -30.00669563604516910, 209.8844732041982013, -6.500000000000000888 ) ) ;
#32267 = CARTESIAN_POINT ( 'NONE',  ( 15.24356964374999990, 244.9093750006145171, 0.000000000000000000 ) ) ;
#32268 = CARTESIAN_POINT ( 'NONE',  ( 8.843639120294245259, 85.26481371789857633, 3.474262827703527901 ) ) ;
#32269 = FACE_BOUND ( 'NONE', #26853, .T. ) ;
#32270 = ORIENTED_EDGE ( 'NONE', *, *, #31547, .T. ) ;
#32271 = CARTESIAN_POINT ( 'NONE',  ( -58.71205436395488420, 214.6737587650352168, 4.842901733360204908 ) ) ;
#32272 = CARTESIAN_POINT ( 'NONE',  ( 21.00000000000000000, 246.5687500012290343, 6.928203230275506996 ) ) ;
#32273 = CARTESIAN_POINT ( 'NONE',  ( -10.49813415416004858, 97.62731371789857349, 7.228626920338840023 ) ) ;
#32274 = CARTESIAN_POINT ( 'NONE',  ( 10.31873187879410736, -3.604726614523244610, -1.959374999385511407 ) ) ;
#32275 = CARTESIAN_POINT ( 'NONE',  ( 36.86223210287109708, 7.646167579472015790E-16, 159.6692148526084907 ) ) ;
#32276 = CARTESIAN_POINT ( 'NONE',  ( 15.24356964375000167, -3.323476615752272600, -3.365624999385478322 ) ) ;
#32277 = CARTESIAN_POINT ( 'NONE',  ( 6.932735513424201024, 64.85231371789855359, -10.69584247140429412 ) ) ;
#32278 = CARTESIAN_POINT ( 'NONE',  ( -13.62178482187500528, 198.4343750006145228, -23.59362340125807123 ) ) ;
#32279 = ORIENTED_EDGE ( 'NONE', *, *, #746, .F. ) ;
#32280 = VECTOR ( 'NONE', #5882, 1000.000000000000000 ) ;
#32281 = ORIENTED_EDGE ( 'NONE', *, *, #26319, .T. ) ;
#32282 = CARTESIAN_POINT ( 'NONE',  ( 23.87821517812500005, -4.985214923628404016, -4.940624999385468286 ) ) ;
#32283 = DIRECTION ( 'NONE',  ( 1.000000000000000000, 0.000000000000000000, 0.000000000000000000 ) ) ;
#32284 = CARTESIAN_POINT ( 'NONE',  ( 18.12178482187499640, 247.4218750006145342, -4.985214923628404904 ) ) ;
#32285 = CARTESIAN_POINT ( 'NONE',  ( -7.228626920339069173, 38.87268628210144072, 10.49813415415989581 ) ) ;
#32286 =( BOUNDED_CURVE ( )  B_SPLINE_CURVE ( 2, ( #20660, #26143, #25770, #17441, #8899, #32207, #29358 ),
 .UNSPECIFIED., .F., .F. ) 
 B_SPLINE_CURVE_WITH_KNOTS ( ( 3, 2, 2, 3 ),
 ( 0.5869565217391293777, 0.5942028985507235017, 0.6014492753623178478, 0.6086956521739120829 ),
 .UNSPECIFIED. ) 
 CURVE ( )  GEOMETRIC_REPRESENTATION_ITEM ( )  RATIONAL_B_SPLINE_CURVE ( ( 1.000000000000020428, 0.8660254037844181685, 1.000000000000000000, 0.8660254037844387076, 1.000000000000000000, 0.8660254037844571373, 0.9999999999999815703 ) ) 
 REPRESENTATION_ITEM ( '' )  );
#32287 = EDGE_CURVE ( 'NONE', #6657, #11819, #10288, .T. ) ;
#32288 = CARTESIAN_POINT ( 'NONE',  ( -55.53794563604516554, 205.3262412349648116, 4.842901733360249317 ) ) ;
#32289 =( NAMED_UNIT ( * ) SI_UNIT ( $, .STERADIAN. ) SOLID_ANGLE_UNIT ( ) );
#32290 = CARTESIAN_POINT ( 'NONE',  ( -32.18377896937850124, 208.9097554298617183, 4.530955311639234040 ) ) ;
#32291 =( NAMED_UNIT ( * ) SI_UNIT ( $, .STERADIAN. ) SOLID_ANGLE_UNIT ( ) );
#32292 =( GEOMETRIC_REPRESENTATION_CONTEXT ( 3 ) GLOBAL_UNCERTAINTY_ASSIGNED_CONTEXT ( ( #6598 ) ) GLOBAL_UNIT_ASSIGNED_CONTEXT ( ( #26556, #12153, #6478 ) ) REPRESENTATION_CONTEXT ( 'NONE', 'WORKASPACE' ) );
#32293 = CARTESIAN_POINT ( 'NONE',  ( 27.89814547376861142, -5.196152422706632912, 163.2673032942497571 ) ) ;
#32294 = CARTESIAN_POINT ( 'NONE',  ( -11.48171059495408208, 79.51481371789856212, 4.944772684328421875 ) ) ;
#32295 = CARTESIAN_POINT ( 'NONE',  ( -55.94122103062156981, 208.9097554298617752, -4.530955311639240257 ) ) ;
#32296 = AXIS2_PLACEMENT_3D ( 'NONE', #9586, #12427, #24368 ) ;
#32297 = CARTESIAN_POINT ( 'NONE',  ( -66.23288769728823411, 203.5309553116391612, -1.857196546604028775 ) ) ;
#32298 = CARTESIAN_POINT ( 'NONE',  ( 18.12178482187500350, -4.985214923628407568, -6.928124999385470772 ) ) ;
#32299 = CARTESIAN_POINT ( 'NONE',  ( 27.00000000000023448, 3.464101615137617163, -2.437499999999998224 ) ) ;
#32300 = CARTESIAN_POINT ( 'NONE',  ( -11.08355503943118592, 81.23981371789855643, -10.83675517735179383 ) ) ;
#32301 = CARTESIAN_POINT ( 'NONE',  ( -59.89211230271182274, 201.5309553116392181, 2.393094931466368980 ) ) ;
#32302 = VERTEX_POINT ( 'NONE', #27570 ) ;
#32303 = CARTESIAN_POINT ( 'NONE',  ( 11.48171059495397728, 82.28518628210146346, 4.944772684328674117 ) ) ;
#32304 = CARTESIAN_POINT ( 'NONE',  ( 10.83675517735155225, 46.06018628210144072, 11.08355503943142573 ) ) ;
#32305 = DIRECTION ( 'NONE',  ( 1.000000000000000000, 0.000000000000000000, 0.000000000000000000 ) ) ;
#32306 =( BOUNDED_CURVE ( )  B_SPLINE_CURVE ( 2, ( #2870, #23919, #17483, #29015, #21086, #20700, #34900, #15197, #3060, #11592, #18050, #6087, #14630, #32624, #29591, #9511, #6284, #14442, #32244, #17860, #8944, #6662, #29403, #15005, #23729, #20518, #23350, #26555, #26180, #17671, #29207, #26367, #3248, #584, #20891, #217, #32434, #6477, #11782, #18236, #26744, #25998, #27, #23168, #34710, #8756, #20329, #31870, #24845, #24659, #27691, #32811, #24480, #21461, #36026, #4192, #27318, #24108, #13104, #1530, #30548, #7605, #4377, #35652, #12728, #21274, #1720, #30354, #15955, #33569, #36210, #9881, #33002, #7053, #18621, #30163, #12542, #15767, #10253, #1345, #21829, #9697, #10069, #15574, #33383, #6852, #12917, #27508, #18810, #29971, #13289, #18428, #21641, #33194, #24296, #7422, #18992, #27130, #4001, #29780, #4565, #3810, #16141, #35839, #36396, #1156, #7236, #10442, #22016, #15388, #26936, #966, #8350, #25221, #34490, #5309, #7792, #33936, #19923, #30912, #19182, #33753, #19370, #37321, #16700, #13671, #31460, #4931, #27874, #34306, #22386, #16513, #11371, #5483, #28605, #22572, #30729, #25403, #36953, #36771, #22944, #10999, #34118, #28422, #10815, #2095, #13855, #28060, #7978, #19551, #5121, #31100, #4753, #28249, #16326, #25586, #8168, #19742, #17067, #2278, #1905, #31280, #16886, #25027, #25769, #2463, #14036, #2643, #14219, #37141, #10625, #13475, #36585, #11184, #22757, #22204, #3018, #28978, #3204, #20286, #14589, #23876, #26699, #20474, #32013, #31644, #26324, #6430, #2829, #26141, #8531, #35340, #31827, #28792, #12301, #5861, #18004, #6044, #29161, #23125, #23682, #23310, #14780, #11553, #3587, #3395, #29548, #34669, #360, #173, #11925, #17630, #23493, #14401, #29355, #17819, #9278, #35042, #5672, #730, #20658, #8715, #15149, #9089, #32205, #20097, #14964, #11741, #34856, #8897, #6241, #26512, #25958, #542, #12108, #35228, #20850, #17439, #32390, #17253, #26895, #925, #24250, #35985, #24436, #35608, #7377, #29733, #35794, #30120, #18379, #18766, #10021, #32769, #3767, #1677, #4332, #4151, #1299, #9837, #21414, #9652, #12495, #6804, #30502, #27650, #15912, #7196, #24619 ),
 .UNSPECIFIED., .F., .F. ) 
 B_SPLINE_CURVE_WITH_KNOTS ( ( 3, 2, 2, 2, 2, 2, 2, 2, 2, 2, 2, 2, 2, 2, 2, 2, 2, 2, 2, 2, 2, 2, 2, 2, 2, 2, 2, 2, 2, 2, 2, 2, 2, 2, 2, 2, 2, 2, 2, 2, 2, 2, 2, 2, 2, 2, 2, 2, 2, 2, 2, 2, 2, 2, 2, 2, 2, 2, 2, 2, 2, 2, 2, 2, 2, 2, 2, 2, 2, 2, 2, 2, 2, 2, 2, 2, 2, 2, 2, 2, 2, 2, 2, 2, 2, 2, 2, 2, 2, 2, 2, 2, 2, 2, 2, 2, 2, 2, 2, 2, 2, 2, 2, 2, 2, 2, 2, 2, 2, 2, 2, 2, 2, 2, 2, 2, 2, 2, 2, 2, 2, 2, 2, 2, 2, 2, 2, 2, 2, 2, 2, 2, 2, 2, 3 ),
 ( 0.000000000000000000, 0.007246376811594202987, 0.01449275362318840597, 0.02173913043478260809, 0.02898550724637681195, 0.03623188405797101580, 0.04347826086956521618, 0.05072463768115942351, 0.05797101449275362389, 0.06521739130434782428, 0.07246376811594203160, 0.07971014492753622505, 0.08695652173913043237, 0.09420289855072463969, 0.1014492753623188470, 0.1086956521739130405, 0.1159420289855072478, 0.1231884057971014551, 0.1304347826086956486, 0.1376811594202898559, 0.1449275362318840632, 0.1521739130434782705, 0.1594202898550724501, 0.1666666666666666574, 0.1739130434782608647, 0.1811594202898550721, 0.1884057971014492794, 0.1956521739130434867, 0.2028985507246376940, 0.2101449275362318736, 0.2173913043478260809, 0.2246376811594202882, 0.2318840579710144956, 0.2391304347826087029, 0.2463768115942029102, 0.2536231884057971175, 0.2608695652173912971, 0.2681159420289855322, 0.2753623188405797118, 0.2826086956521738913, 0.2898550724637681264, 0.2971014492753623615, 0.3043478260869565410, 0.3115942028985507206, 0.3188405797101449002, 0.3260869565217391353, 0.3333333333333333148, 0.3405797101449275499, 0.3478260869565217295, 0.3550724637681159646, 0.3623188405797101441, 0.3695652173913043237, 0.3768115942028985588, 0.3840579710144927383, 0.3913043478260869734, 0.3985507246376811530, 0.4057971014492753881, 0.4130434782608695676, 0.4202898550724637472, 0.4275362318840579823, 0.4347826086956521618, 0.4420289855072463969, 0.4492753623188405765, 0.4565217391304347561, 0.4637681159420289911, 0.4710144927536231707, 0.4782608695652174058, 0.4855072463768115854, 0.4927536231884058204, 0.5000000000000000000, 0.5072463768115942351, 0.5144927536231883591, 0.5217391304347825942, 0.5289855072463768293, 0.5362318840579710644, 0.5434782608695651884, 0.5507246376811594235, 0.5579710144927536586, 0.5652173913043477826, 0.5724637681159420177, 0.5797101449275362528, 0.5869565217391304879, 0.5942028985507247230, 0.6014492753623188470, 0.6086956521739130821, 0.6159420289855072062, 0.6231884057971014412, 0.6304347826086956763, 0.6376811594202898004, 0.6449275362318840354, 0.6521739130434782705, 0.6594202898550725056, 0.6666666666666666297, 0.6739130434782608647, 0.6811594202898550998, 0.6884057971014493349, 0.6956521739130434590, 0.7028985507246376940, 0.7101449275362319291, 0.7173913043478260532, 0.7246376811594202882, 0.7318840579710145233, 0.7391304347826086474, 0.7463768115942028825, 0.7536231884057971175, 0.7608695652173913526, 0.7681159420289854767, 0.7753623188405797118, 0.7826086956521739468, 0.7898550724637680709, 0.7971014492753623060, 0.8043478260869565410, 0.8115942028985507761, 0.8188405797101449002, 0.8260869565217391353, 0.8333333333333333703, 0.8405797101449274944, 0.8478260869565217295, 0.8550724637681159646, 0.8623188405797101996, 0.8695652173913043237, 0.8768115942028985588, 0.8840579710144927938, 0.8913043478260869179, 0.8985507246376811530, 0.9057971014492753881, 0.9130434782608695121, 0.9202898550724637472, 0.9275362318840579823, 0.9347826086956522174, 0.9420289855072463414, 0.9492753623188405765, 0.9565217391304348116, 0.9637681159420289356, 0.9662082966761270653 ),
 .UNSPECIFIED. ) 
 CURVE ( )  GEOMETRIC_REPRESENTATION_ITEM ( )  RATIONAL_B_SPLINE_CURVE ( ( 1.000000000000000000, 0.8660254037844387076, 1.000000000000000000, 0.8660254037844387076, 1.000000000000000000, 0.8660254037844387076, 1.000000000000000000, 0.8660254037844387076, 1.000000000000000000, 0.8660254037844387076, 1.000000000000000000, 0.8660254037844387076, 1.000000000000000000, 0.8660254037844387076, 1.000000000000000000, 0.8660254037844387076, 1.000000000000000000, 0.8660254037844387076, 1.000000000000000000, 0.8660254037844387076, 1.000000000000000000, 0.8660254037844387076, 1.000000000000000000, 0.8660254037844387076, 1.000000000000000000, 0.8660254037844387076, 1.000000000000000000, 0.8660254037844387076, 1.000000000000000000, 0.8660254037844387076, 1.000000000000000000, 0.8660254037844387076, 1.000000000000000000, 0.8660254037844387076, 1.000000000000000000, 0.8660254037844387076, 1.000000000000000000, 0.8660254037844387076, 1.000000000000000000, 0.8660254037844387076, 1.000000000000000000, 0.8660254037844387076, 1.000000000000000000, 0.8660254037844387076, 1.000000000000000000, 0.8660254037844387076, 1.000000000000000000, 0.8660254037844387076, 1.000000000000000000, 0.8660254037844387076, 1.000000000000000000, 0.8660254037844387076, 1.000000000000000000, 0.8660254037844387076, 1.000000000000000000, 0.8660254037844387076, 1.000000000000000000, 0.8660254037844387076, 1.000000000000000000, 0.8660254037844387076, 1.000000000000000000, 0.8660254037844387076, 1.000000000000000000, 0.8660254037844387076, 1.000000000000000000, 0.8660254037844387076, 1.000000000000000000, 0.8660254037844387076, 1.000000000000000000, 0.8660254037844387076, 1.000000000000000000, 0.8660254037844387076, 1.000000000000000000, 0.8660254037844387076, 1.000000000000000000, 0.8660254037844387076, 1.000000000000000000, 0.8660254037844387076, 1.000000000000000000, 0.8660254037844387076, 1.000000000000000000, 0.8660254037844387076, 1.000000000000000000, 0.8660254037844387076, 1.000000000000000000, 0.8660254037844387076, 1.000000000000000000, 0.8660254037844387076, 1.000000000000000000, 0.8660254037844387076, 1.000000000000000000, 0.8660254037844387076, 1.000000000000000000, 0.8660254037844387076, 1.000000000000000000, 0.8660254037844387076, 1.000000000000000000, 0.8660254037844387076, 1.000000000000000000, 0.8660254037844387076, 1.000000000000000000, 0.8660254037844387076, 1.000000000000000000, 0.8660254037844387076, 1.000000000000000000, 0.8660254037844387076, 1.000000000000000000, 0.8660254037844387076, 1.000000000000000000, 0.8660254037844387076, 1.000000000000000000, 0.8660254037844387076, 1.000000000000000000, 0.8660254037844387076, 1.000000000000000000, 0.8660254037844387076, 1.000000000000000000, 0.8660254037844387076, 1.000000000000000000, 0.8660254037844387076, 1.000000000000000000, 0.8660254037844387076, 1.000000000000000000, 0.8660254037844387076, 1.000000000000000000, 0.8660254037844387076, 1.000000000000000000, 0.8660254037844387076, 1.000000000000000000, 0.8660254037844387076, 1.000000000000000000, 0.8660254037844387076, 1.000000000000000000, 0.8660254037844387076, 1.000000000000000000, 0.8660254037844387076, 1.000000000000000000, 0.8660254037844387076, 1.000000000000000000, 0.8660254037844387076, 1.000000000000000000, 0.8660254037844387076, 1.000000000000000000, 0.8660254037844387076, 1.000000000000000000, 0.8660254037844387076, 1.000000000000000000, 0.8660254037844387076, 1.000000000000000000, 0.8660254037844387076, 1.000000000000000000, 0.8660254037844387076, 1.000000000000000000, 0.8660254037844387076, 1.000000000000000000, 0.8660254037844387076, 1.000000000000000000, 0.8660254037844387076, 1.000000000000000000, 0.8660254037844387076, 1.000000000000000000, 0.8660254037844387076, 1.000000000000000000, 0.8660254037844387076, 1.000000000000000000, 0.8660254037844387076, 1.000000000000000000, 0.8660254037844387076, 1.000000000000000000, 0.8660254037844387076, 1.000000000000000000, 0.8660254037844387076, 1.000000000000000000, 0.8660254037844387076, 1.000000000000000000, 0.8660254037844387076, 1.000000000000000000, 0.8660254037844387076, 1.000000000000000000, 0.8660254037844387076, 1.000000000000000000, 0.8660254037844387076, 1.000000000000000000, 0.8660254037844387076, 1.000000000000000000, 0.8660254037844387076, 1.000000000000000000, 0.8660254037844387076, 1.000000000000000000, 0.8660254037844387076, 1.000000000000000000, 0.8660254037844387076, 1.000000000000000000, 0.8660254037844387076, 1.000000000000000000, 0.8660254037844387076, 1.000000000000000000, 0.8660254037844387076, 1.000000000000000000, 0.8660254037844387076, 1.000000000000000000, 0.8660254037844387076, 1.000000000000000000, 0.8660254037844387076, 1.000000000000000000, 0.8660254037844387076, 1.000000000000000000, 0.8660254037844387076, 1.000000000000000000, 0.8660254037844387076, 1.000000000000000000, 0.8660254037844387076, 1.000000000000000000, 0.8660254037844387076, 1.000000000000000000, 0.8660254037844387076, 1.000000000000000000, 0.8660254037844387076, 1.000000000000000000, 0.8660254037844387076, 1.000000000000000000, 0.8660254037844387076, 1.000000000000000000, 0.8660254037844387076, 1.000000000000000000, 0.8660254037844387076, 1.000000000000000000, 0.8660254037844387076, 1.000000000000000000, 0.8660254037844387076, 1.000000000000000000, 0.8660254037844387076, 1.000000000000000000, 0.8660254037844387076, 1.000000000000000000, 0.8660254037844387076, 1.000000000000000000, 0.8660254037844387076, 1.000000000000000000, 0.8660254037844387076, 1.000000000000000000, 0.8660254037844387076, 1.000000000000000000, 0.8660254037844387076, 1.000000000000000000, 0.8660254037844387076, 1.000000000000000000, 0.8660254037844387076, 1.000000000000000000, 0.8660254037844387076, 1.000000000000000000, 0.8660254037844387076, 1.000000000000000000, 0.8660254037844387076, 1.000000000000000000, 0.8660254037844387076, 1.000000000000000000, 0.8660254037844387076, 1.000000000000000000, 0.8660254037844387076, 1.000000000000000000, 0.8660254037844387076, 1.000000000000000000, 0.8660254037844387076, 1.000000000000000000, 0.8660254037844387076, 1.000000000000000000, 0.9548847324609573972, 0.9401541411607521326 ) ) 
 REPRESENTATION_ITEM ( '' )  );
#32307 = CARTESIAN_POINT ( 'NONE',  ( 33.79318086914889818, 5.407089921784862696, 160.4082625921878673 ) ) ;
#32308 = CARTESIAN_POINT ( 'NONE',  ( 15.53471296425195369, 53.82268628210144357, -2.908627838312120684 ) ) ;
#32309 = EDGE_CURVE ( 'NONE', #483, #30424, #20698, .T. ) ;
#32310 = CARTESIAN_POINT ( 'NONE',  ( 10.31873187879411269, 3.604726614523236616, -9.178124999385520510 ) ) ;
#32311 = CARTESIAN_POINT ( 'NONE',  ( 0.000000000000000000, 210.0000000000000284, 0.000000000000000000 ) ) ;
#32312 = CARTESIAN_POINT ( 'NONE',  ( -53.17038769728823411, 208.1428034533959703, 6.469044688360770401 ) ) ;
#32313 = CARTESIAN_POINT ( 'NONE',  ( 13.18934786828137362, 5.048416078761468917, -9.999999999999994671 ) ) ;
#32314 = CARTESIAN_POINT ( 'NONE',  ( 4.944772684328679446, 33.98518628210143788, -11.48171059495397373 ) ) ;
#32315 = CARTESIAN_POINT ( 'NONE',  ( 15.00000000000000000, 0.000000000000000000, -3.149999999999986144 ) ) ;
#32316 = CARTESIAN_POINT ( 'NONE',  ( -9.500000000000005329, 144.4898137178985280, 0.1745138560723101806 ) ) ;
#32317 = CARTESIAN_POINT ( 'NONE',  ( 15.24356964374999990, 246.2593750006145399, 0.000000000000000000 ) ) ;
#32318 = ORIENTED_EDGE ( 'NONE', *, *, #12017, .T. ) ;
#32319 = CARTESIAN_POINT ( 'NONE',  ( 15.00000000000000000, 3.464101615137752166, -5.887500000000005507 ) ) ;
#32320 = DIRECTION ( 'NONE',  ( -1.000000000000000000, 0.000000000000000000, 1.558072081575740353E-16 ) ) ;
#32321 = CARTESIAN_POINT ( 'NONE',  ( 13.56230152254411436, -5.196152422706632912, -3.412499998771051146 ) ) ;
#32322 = CARTESIAN_POINT ( 'NONE',  ( 19.68408634441910721, -5.407089921784855591, -4.040624999385538985 ) ) ;
#32323 = AXIS2_PLACEMENT_3D ( 'NONE', #36486, #33467, #10530 ) ;
#32324 = CARTESIAN_POINT ( 'NONE',  ( 25.03052145599531997, 0.000000000000000000, 167.7059987711938902 ) ) ;
#32325 = CARTESIAN_POINT ( 'NONE',  ( 15.00000000000000000, 240.5500000000000114, 0.000000000000000000 ) ) ;
#32326 = CARTESIAN_POINT ( 'NONE',  ( 26.99999999999999645, 199.8125000000000000, -15.58845726811990495 ) ) ;
#32327 = VECTOR ( 'NONE', #21887, 1000.000000000000000 ) ;
#32328 = CARTESIAN_POINT ( 'NONE',  ( -6.932735513423968321, 50.94768628210144357, -10.69584247140445221 ) ) ;
#32329 = VERTEX_POINT ( 'NONE', #32498 ) ;
#32330 = ORIENTED_EDGE ( 'NONE', *, *, #26378, .F. ) ;
#32331 = CARTESIAN_POINT ( 'NONE',  ( -6.000000000000000888, -30.00000000000000000, -19.99999999999999289 ) ) ;
#32332 = DIRECTION ( 'NONE',  ( 0.000000000000000000, -1.000000000000000000, 0.000000000000000000 ) ) ;
#32333 = CARTESIAN_POINT ( 'NONE',  ( 24.00000000000000000, 242.9499999999999886, 5.196152422706629359 ) ) ;
#32334 = CARTESIAN_POINT ( 'NONE',  ( 23.87821517812500005, -4.985214923628404016, -6.740624999385463667 ) ) ;
#32335 = CARTESIAN_POINT ( 'NONE',  ( 10.69584247140445221, 99.24768628210146915, -6.932735513423970097 ) ) ;
#32336 = CARTESIAN_POINT ( 'NONE',  ( 14.25334919248795451, 28.91481371789854649, -6.092822981423661410 ) ) ;
#32337 = CYLINDRICAL_SURFACE ( 'NONE', #4872, 5.999999999999998224 ) ;
#32338 = CARTESIAN_POINT ( 'NONE',  ( 23.87821517812500005, 241.0093750006145399, 4.985214923628404016 ) ) ;
#32339 = CARTESIAN_POINT ( 'NONE',  ( -31.99330436395490196, 210.1155267958017703, -4.499999999999996447 ) ) ;
#32340 = DIRECTION ( 'NONE',  ( -0.000000000000000000, -1.000000000000000000, -0.000000000000000000 ) ) ;
#32341 = CARTESIAN_POINT ( 'NONE',  ( 24.40136593803570975, -3.604726614523244610, 160.5147182943441067 ) ) ;
#32342 = CARTESIAN_POINT ( 'NONE',  ( 5.529263428287300108, 12.52731371789855963, 7.954856959092309943 ) ) ;
#32343 = ADVANCED_FACE ( 'NONE', ( #6544 ), #3971, .F. ) ;
#32344 = CARTESIAN_POINT ( 'NONE',  ( -63.26413769728824121, 213.1499508600178672, 5.686928522499718142 ) ) ;
#32345 = CARTESIAN_POINT ( 'NONE',  ( -32.77752896937849414, 214.3500491399821897, 7.303452534266821949 ) ) ;
#32346 = CARTESIAN_POINT ( 'NONE',  ( 0.000000000000000000, 250.0000000000000000, 0.000000000000000000 ) ) ;
#32347 = CARTESIAN_POINT ( 'NONE',  ( 26.75643035624999655, -3.323476615752267271, -0.5156249993854836733 ) ) ;
#32348 = CARTESIAN_POINT ( 'NONE',  ( -27.24356964375000345, 196.2593750006145399, 0.000000000000000000 ) ) ;
#32349 = CARTESIAN_POINT ( 'NONE',  ( -10.83675517735179028, 134.1398137178985621, 11.08355503943118947 ) ) ;
#32350 = CARTESIAN_POINT ( 'NONE',  ( -60.09002896937850124, 204.4285982733020433, 3.350049139982171020 ) ) ;
#32351 =( BOUNDED_CURVE ( )  B_SPLINE_CURVE ( 2, ( #5139, #28814, #14423, #8738, #19942, #28998, #17090, #16720, #25424 ),
 .UNSPECIFIED., .F., .F. ) 
 B_SPLINE_CURVE_WITH_KNOTS ( ( 3, 2, 2, 2, 3 ),
 ( 0.6847826086956522174, 0.6884057971014492239, 0.6956521739130434590, 0.7028985507246376940, 0.7065217391304348116 ),
 .UNSPECIFIED. ) 
 CURVE ( )  GEOMETRIC_REPRESENTATION_ITEM ( )  RATIONAL_B_SPLINE_CURVE ( ( 0.9330127018922192983, 0.9330127018922202975, 1.000000000000000000, 0.8660254037844387076, 1.000000000000000000, 0.8660254037844387076, 1.000000000000000000, 0.9330127018922194093, 0.9330127018922194093 ) ) 
 REPRESENTATION_ITEM ( '' )  );
#32352 = ORIENTED_EDGE ( 'NONE', *, *, #6458, .T. ) ;
#32353 = CARTESIAN_POINT ( 'NONE',  ( -6.932735513423968321, 41.74768628210144783, -10.69584247140445221 ) ) ;
#32354 = CARTESIAN_POINT ( 'NONE',  ( -29.00000000000002487, 222.9518338469886203, -12.50000000000000000 ) ) ;
#32355 = CARTESIAN_POINT ( 'NONE',  ( 19.80074372294634344, 5.630122097104456991, -7.999999999999998224 ) ) ;
#32356 = CARTESIAN_POINT ( 'NONE',  ( 37.40641077165175687, 7.646167579472024665E-16, 165.8892054988188534 ) ) ;
#32357 = CARTESIAN_POINT ( 'NONE',  ( 18.00000000000000000, 5.196152422706630247, -3.168749998770953091 ) ) ;
#32358 =( LENGTH_UNIT ( ) NAMED_UNIT ( * ) SI_UNIT ( .MILLI., .METRE. ) );
#32359 = CARTESIAN_POINT ( 'NONE',  ( 10.31873187879411091, 0.000000000000000000, -2.390624999385526639 ) ) ;
#32360 = CARTESIAN_POINT ( 'NONE',  ( -9.465287035748065847, 58.99768628210144783, -2.064181346179273735 ) ) ;
#32361 = DIRECTION ( 'NONE',  ( -0.000000000000000000, -1.000000000000000000, -0.000000000000000000 ) ) ;
#32362 = CARTESIAN_POINT ( 'NONE',  ( 26.99999999999999645, 245.7249999999999943, -7.347880794884117764E-16 ) ) ;
#32363 = CARTESIAN_POINT ( 'NONE',  ( -12.53471296425194836, 95.22268628210146346, 2.311890736173176641 ) ) ;
#32364 = CARTESIAN_POINT ( 'NONE',  ( 13.49999999999999645, 199.5125000012290286, -23.38268590217984766 ) ) ;
#32365 = FACE_OUTER_BOUND ( 'NONE', #34383, .T. ) ;
#32366 = ORIENTED_EDGE ( 'NONE', *, *, #790, .F. ) ;
#32367 = CARTESIAN_POINT ( 'NONE',  ( 24.48144027668511669, 0.000000000000000000, 161.4299721732159014 ) ) ;
#32368 = CARTESIAN_POINT ( 'NONE',  ( 26.75643035624999655, 3.323476615752271712, -9.778124999385472194 ) ) ;
#32369 = CARTESIAN_POINT ( 'NONE',  ( 19.56230152254412502, -5.196152422706635576, -6.600000000000050271 ) ) ;
#32370 = CARTESIAN_POINT ( 'NONE',  ( 37.40314243129871841, -3.604726614523238837, 165.8518481976404360 ) ) ;
#32371 = PRODUCT_DEFINITION_CONTEXT ( 'detailed design', #25034, 'design' ) ;
#32372 = CARTESIAN_POINT ( 'NONE',  ( 24.93570810221054757, -3.464101615137761048, 163.8276289306958802 ) ) ;
#32373 = CARTESIAN_POINT ( 'NONE',  ( 37.10248660225891371, 7.347880794884125653E-16, 165.2099845943227479 ) ) ;
#32374 = CARTESIAN_POINT ( 'NONE',  ( 24.00000000000000000, 248.7999999999999829, 5.196152422706629359 ) ) ;
#32375 = CARTESIAN_POINT ( 'NONE',  ( 5.778771075727756162E-15, 197.2156250006145513, 31.45816453501076637 ) ) ;
#32376 = ADVANCED_FACE ( 'NONE', ( #26826 ), #10330, .T. ) ;
#32377 = CARTESIAN_POINT ( 'NONE',  ( -2.660918448318004614, 100.5023137178985593, -12.46528703574811558 ) ) ;
#32378 = CARTESIAN_POINT ( 'NONE',  ( -4.622313124798576922, 97.23518628210145209, -11.61527771782819762 ) ) ;
#32380 = ORIENTED_EDGE ( 'NONE', *, *, #10179, .F. ) ;
#32379 = VERTEX_POINT ( 'NONE', #32698 ) ;
#32381 = CARTESIAN_POINT ( 'NONE',  ( 5.778771075727756162E-15, 195.8656250006145285, 31.45816453501075927 ) ) ;
#32382 = CARTESIAN_POINT ( 'NONE',  ( -15.46528703574811736, 79.80231371789852801, 3.257655550456946436 ) ) ;
#32383 = CARTESIAN_POINT ( 'NONE',  ( 15.24356964374999990, 0.000000000000000000, -3.853124999385476812 ) ) ;
#32384 = CARTESIAN_POINT ( 'NONE',  ( 18.12178482187499640, 246.6343750006145115, -4.985214923628404904 ) ) ;
#32385 = CARTESIAN_POINT ( 'NONE',  ( -5.233372021372430183, 106.1476862821014322, -8.152565276336710909 ) ) ;
#32386 = CARTESIAN_POINT ( 'NONE',  ( 27.00000000000000355, 197.1875000012290400, -3.306546357697854128E-15 ) ) ;
#32387 = EDGE_CURVE ( 'NONE', #11777, #10703, #856, .T. ) ;
#32388 = CARTESIAN_POINT ( 'NONE',  ( 6.594114490232462877, 74.33981371789855075, -6.840914352311949109 ) ) ;
#32389 = CARTESIAN_POINT ( 'NONE',  ( 13.44051670066911619, -5.407089921784859143, -4.565624999385536675 ) ) ;
#32390 = CARTESIAN_POINT ( 'NONE',  ( 18.12178482187500350, 240.8218750006145399, 4.985214923628407568 ) ) ;
#32391 = CARTESIAN_POINT ( 'NONE',  ( -12.53471296425189152, 52.77731371789855075, -2.311890736173453753 ) ) ;
#32392 = CARTESIAN_POINT ( 'NONE',  ( 36.86716609684025059, 7.347880794884125653E-16, 162.5202589094750181 ) ) ;
#32393 = CARTESIAN_POINT ( 'NONE',  ( -7.228626920339069173, 103.2726862821014606, 10.49813415415989581 ) ) ;
#32394 = CARTESIAN_POINT ( 'NONE',  ( 10.56230152254410903, 3.464101615137752166, -7.124999998771004428 ) ) ;
#32395 = EDGE_CURVE ( 'NONE', #20367, #2209, #7856, .T. ) ;
#32396 = CARTESIAN_POINT ( 'NONE',  ( -32.78497103062156981, 204.4285982733020148, -3.350049139982115509 ) ) ;
#32397 = CARTESIAN_POINT ( 'NONE',  ( 26.99999999999999645, 7.347880794884117764E-16, -5.624999999999991118 ) ) ;
#32398 = CARTESIAN_POINT ( 'NONE',  ( 24.72002912245681117, -3.604726614523240613, 164.1570551592420486 ) ) ;
#32399 = CARTESIAN_POINT ( 'NONE',  ( 14.38691631536207538, 81.13518628210145778, -5.770363421893813793 ) ) ;
#32400 = CARTESIAN_POINT ( 'NONE',  ( 13.44051670066910908, 5.407089921784862696, -4.321874999385522109 ) ) ;
#32401 = CARTESIAN_POINT ( 'NONE',  ( 2.660918448318279950, 6.097686282101443922, -12.46528703574805874 ) ) ;
#32402 = CARTESIAN_POINT ( 'NONE',  ( 16.56230152254411081, 6.928203230275506996, -7.199999998770998388 ) ) ;
#32403 = CARTESIAN_POINT ( 'NONE',  ( 13.49999999999999645, 198.5000000000000000, -23.38268590217984766 ) ) ;
#32404 = CARTESIAN_POINT ( 'NONE',  ( -5.529263428287477744, 121.6726862821014521, 7.954856959092191815 ) ) ;
#32405 = DIRECTION ( 'NONE',  ( 0.000000000000000000, 0.000000000000000000, -1.000000000000000000 ) ) ;
#32406 = CARTESIAN_POINT ( 'NONE',  ( -14.38691631536207183, 12.13518628210144712, 5.770363421893814682 ) ) ;
#32407 = CARTESIAN_POINT ( 'NONE',  ( -1.926257025242585782E-15, 195.6968750006145683, -31.45816453501075927 ) ) ;
#32408 = CARTESIAN_POINT ( 'NONE',  ( 23.87821517812499650, 242.3968750006145285, -4.985214923628404904 ) ) ;
#32409 = VERTEX_POINT ( 'NONE', #29856 ) ;
#32410 = CARTESIAN_POINT ( 'NONE',  ( 25.10896162446820412, 0.000000000000000000, 168.6025739994764479 ) ) ;
#32411 = CARTESIAN_POINT ( 'NONE',  ( 26.75643035624999655, 7.049594010296217766E-16, -1.715624999385462202 ) ) ;
#32412 = CARTESIAN_POINT ( 'NONE',  ( 13.62178482187501416, 199.1093750006145342, 23.59362340125806767 ) ) ;
#32413 = CARTESIAN_POINT ( 'NONE',  ( 26.99999999999999645, 7.347880794884117764E-16, -3.824999999999994849 ) ) ;
#32414 = CARTESIAN_POINT ( 'NONE',  ( 16.56230152254410726, 0.000000000000000000, -10.00000000000000000 ) ) ;
#32415 = CARTESIAN_POINT ( 'NONE',  ( 34.06814574304114984, -5.196152422706635576, 164.9484496060674985 ) ) ;
#32416 = CARTESIAN_POINT ( 'NONE',  ( 21.00000000000000355, 0.000000000000000000, 50.00000000000001421 ) ) ;
#32417 = CARTESIAN_POINT ( 'NONE',  ( 9.500000000000005329, 11.08981371789854897, -0.1745138560723090149 ) ) ;
#32418 = CARTESIAN_POINT ( 'NONE',  ( 27.24356964375000345, 198.7343750006145626, -3.336375036156643733E-15 ) ) ;
#32419 = ORIENTED_EDGE ( 'NONE', *, *, #23148, .F. ) ;
#32420 = CARTESIAN_POINT ( 'NONE',  ( 23.87821517812500005, 247.1968750006145115, 4.985214923628404016 ) ) ;
#32421 = CARTESIAN_POINT ( 'NONE',  ( -4.622313124798826500, 50.76481371789855501, 11.61527771782809637 ) ) ;
#32422 = CARTESIAN_POINT ( 'NONE',  ( 15.24356964374999990, 0.000000000000000000, -1.940624999385465177 ) ) ;
#32423 = CARTESIAN_POINT ( 'NONE',  ( 15.53471296425188797, 130.9773137178985394, 2.908627838312457747 ) ) ;
#32424 = EDGE_CURVE ( 'NONE', #18565, #19287, #13177, .T. ) ;
#32425 = CARTESIAN_POINT ( 'NONE',  ( 18.00000000000000000, 5.196152422706630247, -6.318749998770966769 ) ) ;
#32426 = CARTESIAN_POINT ( 'NONE',  ( 28.39820154767614468, -5.196152422706638241, 168.9829703733268218 ) ) ;
#32427 = VERTEX_POINT ( 'NONE', #24732 ) ;
#32428 = CARTESIAN_POINT ( 'NONE',  ( 19.68408634441911076, 5.407089921784862696, -3.496874999385557459 ) ) ;
#32429 = CARTESIAN_POINT ( 'NONE',  ( -27.24356964374999635, 199.3906250006145342, 15.72908226750539384 ) ) ;
#32430 = CARTESIAN_POINT ( 'NONE',  ( 24.79356678040014117, -3.604726614523244610, 164.9975944357569517 ) ) ;
#32431 = EDGE_CURVE ( 'NONE', #13040, #4369, #18697, .T. ) ;
#32432 = VECTOR ( 'NONE', #18403, 1000.000000000000000 ) ;
#32433 = CARTESIAN_POINT ( 'NONE',  ( -64.24627896937850835, 201.4690446883607251, -2.162041339862721845 ) ) ;
#32434 = CARTESIAN_POINT ( 'NONE',  ( 15.24356964374999990, 248.3968750006145285, 0.000000000000000000 ) ) ;
#32435 = DIRECTION ( 'NONE',  ( 0.9961946980917462113, 0.000000000000000000, -0.08715574274765118534 ) ) ;
#32436 = CARTESIAN_POINT ( 'NONE',  ( -62.86086230271182984, 212.1499508600178387, -3.954877714930852495 ) ) ;
#32437 = CARTESIAN_POINT ( 'NONE',  ( -34.56622103062155560, 211.6261429550005744, 6.530955311639227823 ) ) ;
#32438 = CARTESIAN_POINT ( 'NONE',  ( 28.14696362483655889, -5.407089921784859143, 167.5086318987019069 ) ) ;
#32439 = VERTEX_POINT ( 'NONE', #36282 ) ;
#32440 = CARTESIAN_POINT ( 'NONE',  ( -28.36931066777353294, 204.7133184642976005, 6.026954303579515226 ) ) ;
#32441 = CARTESIAN_POINT ( 'NONE',  ( 15.46528703574811736, 10.80231371789855466, -3.257655550456947768 ) ) ;
#32442 = CARTESIAN_POINT ( 'NONE',  ( -56.53497103062156270, 202.6965474657331185, -4.350049139982091084 ) ) ;
#32443 = CARTESIAN_POINT ( 'NONE',  ( 2.064181346179272847, 134.8976862821014606, -9.465287035748065847 ) ) ;
#32444 = CARTESIAN_POINT ( 'NONE',  ( 19.39230484541324628, 246.3638461906613486, -5.999999999999989342 ) ) ;
#32445 = CARTESIAN_POINT ( 'NONE',  ( 0.1745138560725515708, 24.21018628210144641, -12.50000000000000355 ) ) ;
#32446 = CARTESIAN_POINT ( 'NONE',  ( 13.56230152254411792, -5.196152422706638241, -6.675000000000069988 ) ) ;
#32447 = EDGE_LOOP ( 'NONE', ( #1918, #16715, #19375, #16332 ) ) ;
#32448 = LINE ( 'NONE', #15407, #26994 ) ;
#32449 = CARTESIAN_POINT ( 'NONE',  ( -3.257655550457281723, 130.2976862821014379, 15.46528703574804986 ) ) ;
#32450 = CARTESIAN_POINT ( 'NONE',  ( 1.120210788295102201E-13, 195.3875000000000455, -27.00000000000000711 ) ) ;
#32451 = CARTESIAN_POINT ( 'NONE',  ( -6.594114490232312775, 4.660186282101435928, -6.840914352312096547 ) ) ;
#32452 = CARTESIAN_POINT ( 'NONE',  ( -13.62178482187498396, 199.4281250006145569, 23.59362340125808188 ) ) ;
#32453 = DIRECTION ( 'NONE',  ( 0.000000000000000000, 0.000000000000000000, -1.000000000000000000 ) ) ;
#32454 = CARTESIAN_POINT ( 'NONE',  ( 17.75238460531252471, -6.096976528379499882, -10.00000000000000000 ) ) ;
#32455 = FACE_OUTER_BOUND ( 'NONE', #17779, .T. ) ;
#32456 = CARTESIAN_POINT ( 'NONE',  ( 24.85399959338462139, 0.000000000000000000, 162.8936964012349051 ) ) ;
#32457 = AXIS2_PLACEMENT_3D ( 'NONE', #33870, #10375, #27625 ) ;
#32458 = CARTESIAN_POINT ( 'NONE',  ( 6.594114490232462877, 83.53981371789856780, -6.840914352311949109 ) ) ;
#32459 = DIRECTION ( 'NONE',  ( 0.1219804832088915297, 0.9925324990730154395, 0.000000000000000000 ) ) ;
#32460 = ORIENTED_EDGE ( 'NONE', *, *, #3812, .T. ) ;
#32461 = CARTESIAN_POINT ( 'NONE',  ( 26.99999999999999645, 246.1937500012290343, 3.464101615137751278 ) ) ;
#32462 = CARTESIAN_POINT ( 'NONE',  ( -10.69584247140429412, 90.15231371789853654, -6.932735513424201024 ) ) ;
#32463 = CARTESIAN_POINT ( 'NONE',  ( 16.56230152254411436, -7.209453229046482114, -2.784374999385508698 ) ) ;
#32464 = CARTESIAN_POINT ( 'NONE',  ( 18.00000000000000000, 246.7750000000000057, -5.196152422706630247 ) ) ;
#32465 = CARTESIAN_POINT ( 'NONE',  ( 21.00000000000000000, -6.646953231504538984, -5.540624999385494576 ) ) ;
#32466 = CARTESIAN_POINT ( 'NONE',  ( 0.1745138560722779009, 59.38981371789856212, 12.50000000000000355 ) ) ;
#32467 = CARTESIAN_POINT ( 'NONE',  ( 27.24356964375000700, 197.7968750006145342, 15.72908226750537075 ) ) ;
#32468 = ORIENTED_EDGE ( 'NONE', *, *, #33739, .F. ) ;
#32469 = ORIENTED_EDGE ( 'NONE', *, *, #2301, .F. ) ;
#32470 = CARTESIAN_POINT ( 'NONE',  ( 15.24356964374999990, 3.323476615752268604, -5.128124999385462957 ) ) ;
#32471 = CARTESIAN_POINT ( 'NONE',  ( 26.75643035624999655, 246.3718750006145228, -7.049594010296217766E-16 ) ) ;
#32472 = CARTESIAN_POINT ( 'NONE',  ( 0.1745138560725515708, 42.61018628210144499, -12.50000000000000355 ) ) ;
#32473 = CARTESIAN_POINT ( 'NONE',  ( -42.67336230271183695, 215.6869285224997270, 3.149950860017831200 ) ) ;
#32474 = CARTESIAN_POINT ( 'NONE',  ( -64.44419563604516554, 203.5000000000000000, 0.1155267958017914542 ) ) ;
#32475 = PRODUCT_CONTEXT ( 'NONE', #21674, 'mechanical' ) ;
#32476 = CARTESIAN_POINT ( 'NONE',  ( 36.84101937412305716, 3.464101615137755275, 162.2214005012718587 ) ) ;
#32477 = CARTESIAN_POINT ( 'NONE',  ( -2.311890736173448424, 87.27731371789856496, 12.53471296425189330 ) ) ;
#32478 = CARTESIAN_POINT ( 'NONE',  ( -56.33705436395490551, 206.7903428501026042, -3.378800118222489157 ) ) ;
#32479 = CARTESIAN_POINT ( 'NONE',  ( -32.78497103062156981, 202.6965474657331185, -4.350049139982091084 ) ) ;
#32480 = CARTESIAN_POINT ( 'NONE',  ( 15.24356964374999990, 3.323476615752268604, -7.940624999385462068 ) ) ;
#32481 = CARTESIAN_POINT ( 'NONE',  ( 19.56230152254412147, 5.196152422706637353, -7.350000000000022737 ) ) ;
#32482 = CARTESIAN_POINT ( 'NONE',  ( 10.83675517735179206, 65.13981371789854791, -11.08355503943118769 ) ) ;
#32483 = CARTESIAN_POINT ( 'NONE',  ( -57.91294563604517265, 216.1378603801729241, -6.307003348498026796 ) ) ;
#32484 = CARTESIAN_POINT ( 'NONE',  ( 22.56230152254412147, 7.347880794884125653E-16, -9.225000000000010303 ) ) ;
#32485 = CARTESIAN_POINT ( 'NONE',  ( 12.50000000000000355, 90.91018628210146346, 0.1745138560725507937 ) ) ;
#32486 = CARTESIAN_POINT ( 'NONE',  ( -13.23911966647218463, 39.44768628210144357, 8.632099005475506459 ) ) ;
#32487 = FACE_OUTER_BOUND ( 'NONE', #28278, .T. ) ;
#32488 = CARTESIAN_POINT ( 'NONE',  ( 24.35560917309319251, 3.604726614523240613, 159.9917160778459220 ) ) ;
#32489 = CARTESIAN_POINT ( 'NONE',  ( 14.25334919248782661, 54.68518628210145494, 6.092822981423971385 ) ) ;
#32490 = VECTOR ( 'NONE', #28893, 1000.000000000000000 ) ;
#32491 = DIRECTION ( 'NONE',  ( 0.000000000000000000, 0.000000000000000000, 1.000000000000000000 ) ) ;
#32492 = CARTESIAN_POINT ( 'NONE',  ( 22.80587116629410360, -3.604726614523235284, -8.953124999385540406 ) ) ;
#32493 = CARTESIAN_POINT ( 'NONE',  ( 15.00000000000000000, 0.000000000000000000, -2.193749998770949894 ) ) ;
#32494 = CARTESIAN_POINT ( 'NONE',  ( -39.51413769728823411, 213.1499508600178672, 5.686928522499718142 ) ) ;
#32495 = EDGE_CURVE ( 'NONE', #29192, #25759, #18879, .T. ) ;
#32496 = CARTESIAN_POINT ( 'NONE',  ( 37.33780710767756972, 7.347880794884125653E-16, 167.8997102791704492 ) ) ;
#32497 = CARTESIAN_POINT ( 'NONE',  ( 2.660918448318279950, 24.49768628210144783, -12.46528703574805697 ) ) ;
#32498 = CARTESIAN_POINT ( 'NONE',  ( -3.253724281355068545E-15, 197.6374999999999602, -27.00000000000000355 ) ) ;
#32499 = CARTESIAN_POINT ( 'NONE',  ( 3.796722387233379514, 15.58518628210145351, -8.710071997420127943 ) ) ;
#32500 = CARTESIAN_POINT ( 'NONE',  ( 26.75643035624999655, 247.3468750006145171, 3.323476615752267271 ) ) ;
#32501 = VERTEX_POINT ( 'NONE', #21901 ) ;
#32502 = CARTESIAN_POINT ( 'NONE',  ( 15.00000000000000178, -3.464101615137757051, -6.262500000000007283 ) ) ;
#32503 = CARTESIAN_POINT ( 'NONE',  ( -47.00000000000000711, 252.0000000000000000, -5.000000000000000000 ) ) ;
#32504 = CARTESIAN_POINT ( 'NONE',  ( 13.50000000000001421, 197.4500000000000171, 23.38268590217984055 ) ) ;
#32505 = CARTESIAN_POINT ( 'NONE',  ( 10.31873187879411091, -3.604726614523240613, -3.253124999385518912 ) ) ;
#32506 = CARTESIAN_POINT ( 'NONE',  ( 31.24052741120653209, 7.209453229046475009, 167.0497639179608313 ) ) ;
#32507 =( BOUNDED_CURVE ( )  B_SPLINE_CURVE ( 2, ( #935, #29941, #32403, #15163, #24262, #23695, #29367, #29746, #3968 ),
 .UNSPECIFIED., .F., .T. ) 
 B_SPLINE_CURVE_WITH_KNOTS ( ( 3, 2, 2, 2, 3 ),
 ( 0.2708333333333333703, 0.2777777777777777901, 0.2916666666666666852, 0.3055555555555555802, 0.3125000000000000000 ),
 .UNSPECIFIED. ) 
 CURVE ( )  GEOMETRIC_REPRESENTATION_ITEM ( )  RATIONAL_B_SPLINE_CURVE ( ( 0.9330127018922194093, 0.9330127018922196314, 1.000000000000000000, 0.8660254037844387076, 1.000000000000000000, 0.8660254037844387076, 1.000000000000000000, 0.9330127018922194093, 0.9330127018922194093 ) ) 
 REPRESENTATION_ITEM ( '' )  );
#32508 = CARTESIAN_POINT ( 'NONE',  ( 26.99999999999999645, 240.7749999999999773, -7.347880794884117764E-16 ) ) ;
#32509 = DIRECTION ( 'NONE',  ( -0.000000000000000000, -1.000000000000000000, -0.000000000000000000 ) ) ;
#32510 = CARTESIAN_POINT ( 'NONE',  ( 11.61527771782819940, 53.53518628210144925, -4.622313124798573369 ) ) ;
#32511 = ORIENTED_EDGE ( 'NONE', *, *, #2301, .T. ) ;
#32512 = VERTEX_POINT ( 'NONE', #35541 ) ;
#32513 = CARTESIAN_POINT ( 'NONE',  ( 13.50000000000001421, 196.6625000012290343, 23.38268590217984055 ) ) ;
#32514 = CARTESIAN_POINT ( 'NONE',  ( 16.56230152254411436, -6.928203230275506996, -2.024999998770999454 ) ) ;
#32515 = CARTESIAN_POINT ( 'NONE',  ( 20.99999999999999645, -6.928203230275506996, -3.431249998770965703 ) ) ;
#32516 = CARTESIAN_POINT ( 'NONE',  ( 21.00000000000000000, 249.0437500012290570, -5.999999999999998224 ) ) ;
#32517 = CARTESIAN_POINT ( 'NONE',  ( 26.75643035624999655, 3.323476615752271712, -5.278124999385452654 ) ) ;
#32518 = CARTESIAN_POINT ( 'NONE',  ( 4.944772684328679446, 89.18518628210145494, -11.48171059495397373 ) ) ;
#32519 = CARTESIAN_POINT ( 'NONE',  ( -14.25334919248795096, 24.31481371789855217, 6.092822981423662299 ) ) ;
#32520 = FACE_OUTER_BOUND ( 'NONE', #10289, .T. ) ;
#32521 = ADVANCED_FACE ( 'NONE', ( #27202 ), #3704, .F. ) ;
#32522 = LINE ( 'NONE', #29682, #19641 ) ;
#32523 = CARTESIAN_POINT ( 'NONE',  ( -68.00669563604516554, 209.8844732041982297, -4.499999999999996447 ) ) ;
#32524 = AXIS2_PLACEMENT_3D ( 'NONE', #18898, #12152, #3627 ) ;
#32525 = CARTESIAN_POINT ( 'NONE',  ( 21.00000000000000000, 245.6125000000000114, 5.999999999999998224 ) ) ;
#32526 = CARTESIAN_POINT ( 'NONE',  ( 30.66693367924855096, -7.209453229046482114, 160.4935575611445415 ) ) ;
#32527 = CARTESIAN_POINT ( 'NONE',  ( -9.534712964251895073, 6.777313717898553413, -1.715153634034446428 ) ) ;
#32528 = CARTESIAN_POINT ( 'NONE',  ( -58.31622103062155560, 211.6261429550005744, 6.530955311639227823 ) ) ;
#32529 = CARTESIAN_POINT ( 'NONE',  ( -35.15252896937850124, 205.6499508600178103, -7.303452534266820173 ) ) ;
#32530 = ADVANCED_FACE ( 'NONE', ( #21160 ), #21536, .F. ) ;
#32531 =( BOUNDED_CURVE ( )  B_SPLINE_CURVE ( 2, ( #27918, #4795, #16373, #1949, #13519, #21689, #10670 ),
 .UNSPECIFIED., .F., .F. ) 
 B_SPLINE_CURVE_WITH_KNOTS ( ( 3, 2, 2, 3 ),
 ( 0.6521739130434789367, 0.6594202898550732828, 0.6666666666666675178, 0.6739130434782618639 ),
 .UNSPECIFIED. ) 
 CURVE ( )  GEOMETRIC_REPRESENTATION_ITEM ( )  RATIONAL_B_SPLINE_CURVE ( ( 0.9999999999999876765, 0.8660254037844510311, 1.000000000000000000, 0.8660254037844387076, 1.000000000000000000, 0.8660254037844202779, 1.000000000000018430 ) ) 
 REPRESENTATION_ITEM ( '' )  );
#32532 = APPLICATION_PROTOCOL_DEFINITION ( 'draft international standard', 'automotive_design', 1998, #11249 ) ;
#32533 = DIRECTION ( 'NONE',  ( 0.000000000000000000, 0.000000000000000000, 1.000000000000000000 ) ) ;
#32534 = CARTESIAN_POINT ( 'NONE',  ( 27.24356964375000345, 198.2281250006145399, -3.336375036156643733E-15 ) ) ;
#32535 = CARTESIAN_POINT ( 'NONE',  ( -6.092822981423666739, 118.6148137178985706, -14.25334919248795096 ) ) ;
#32536 = CARTESIAN_POINT ( 'NONE',  ( -59.89211230271182984, 203.5309553116391612, 1.857196546604092280 ) ) ;
#32537 = VERTEX_POINT ( 'NONE', #4450 ) ;
#32538 = CARTESIAN_POINT ( 'NONE',  ( 8.962234695871762469, 43.76018628210144357, -8.715434833791931624 ) ) ;
#32539 = CARTESIAN_POINT ( 'NONE',  ( 10.56230152254410903, 7.347880794884117764E-16, -10.00000000000000000 ) ) ;
#32540 = CARTESIAN_POINT ( 'NONE',  ( 28.22050128277989245, -5.407089921784865361, 168.3491711752168385 ) ) ;
#32541 = CARTESIAN_POINT ( 'NONE',  ( -13.23911966647218463, 94.64768628210147483, 8.632099005475506459 ) ) ;
#32542 = CARTESIAN_POINT ( 'NONE',  ( -62.86830436395490551, 209.8844732041982581, 6.500000000000000888 ) ) ;
#32543 = CARTESIAN_POINT ( 'NONE',  ( 10.31873187879411091, 3.604726614523236616, -1.528124999385498173 ) ) ;
#32544 = CARTESIAN_POINT ( 'NONE',  ( 9.465287035748067623, 63.59768628210142793, 2.064181346179272847 ) ) ;
#32545 = CARTESIAN_POINT ( 'NONE',  ( 20.99999999999999645, 185.0294372515228645, -5.999999999999999112 ) ) ;
#32546 = CARTESIAN_POINT ( 'NONE',  ( 24.00000000000000000, 244.7500000000000000, 5.196152422706629359 ) ) ;
#32547 = CARTESIAN_POINT ( 'NONE',  ( -8.715434833791929847, 78.26018628210144357, -8.962234695871762469 ) ) ;
#32548 = CARTESIAN_POINT ( 'NONE',  ( 27.00000000000001421, 199.4000000012290457, 15.58845726811988897 ) ) ;
#32549 = CARTESIAN_POINT ( 'NONE',  ( -26.99999999999999645, 195.2000000012290286, 15.58845726811991561 ) ) ;
#32550 = ORIENTED_EDGE ( 'NONE', *, *, #17498, .T. ) ;
#32551 = CARTESIAN_POINT ( 'NONE',  ( 30.59339602130522096, -7.209453229046475009, 159.6530182846296384 ) ) ;
#32552 = CARTESIAN_POINT ( 'NONE',  ( 23.87821517812499650, 4.985214923628404904, -9.740624999385467220 ) ) ;
#32553 = AXIS2_PLACEMENT_3D ( 'NONE', #8446, #31197, #2932 ) ;
#32555 = ADVANCED_FACE ( 'NONE', ( #21717 ), #33082, .T. ) ;
#32554 = CARTESIAN_POINT ( 'NONE',  ( 1.069080835302379631E-14, 198.4250000012290229, 27.00000000000000000 ) ) ;
#32556 = CARTESIAN_POINT ( 'NONE',  ( 31.07874456373120609, 7.209453229046482114, 165.2005775096280615 ) ) ;
#32557 = CARTESIAN_POINT ( 'NONE',  ( 24.89648801797410727, -3.464101615137761048, 163.3793413165546440 ) ) ;
#32558 = CARTESIAN_POINT ( 'NONE',  ( 3.306546357697853733E-15, 210.0000000000000284, 27.00000000000000000 ) ) ;
#32559 = CARTESIAN_POINT ( 'NONE',  ( 15.00000000000000000, 248.6500000000000057, 0.000000000000000000 ) ) ;
#32560 = CARTESIAN_POINT ( 'NONE',  ( -27.24356964375000345, 197.0656250006145171, -15.72908226750537786 ) ) ;
#32561 = CARTESIAN_POINT ( 'NONE',  ( -4.944772684328424539, 109.4148137178985536, -11.48171059495408031 ) ) ;
#32562 = CARTESIAN_POINT ( 'NONE',  ( -4.944772684328673229, 102.9851862821014663, 11.48171059495397728 ) ) ;
#32563 = VECTOR ( 'NONE', #32078, 1000.000000000000000 ) ;
#32564 = VERTEX_POINT ( 'NONE', #15464 ) ;
#32565 = CARTESIAN_POINT ( 'NONE',  ( -13.62178482187500528, 195.2281250006145399, -23.59362340125807123 ) ) ;
#32566 = DIRECTION ( 'NONE',  ( 0.000000000000000000, 0.000000000000000000, 1.000000000000000000 ) ) ;
#32567 = EDGE_CURVE ( 'NONE', #25042, #13953, #23132, .T. ) ;
#32568 = CARTESIAN_POINT ( 'NONE',  ( 11.08355503943118769, 67.43981371789855928, 10.83675517735179028 ) ) ;
#32569 = CARTESIAN_POINT ( 'NONE',  ( 21.00000000000000000, -6.646953231504538984, -5.090624999385466865 ) ) ;
#32570 = CARTESIAN_POINT ( 'NONE',  ( 21.00000000000000000, 247.4968750006145513, -6.646953231504538984 ) ) ;
#32571 = CARTESIAN_POINT ( 'NONE',  ( 5.233372021372432847, 101.5476862821014663, 8.152565276336710909 ) ) ;
#32572 =( BOUNDED_CURVE ( )  B_SPLINE_CURVE ( 3, ( #7115, #4069, #15641, #30227 ),
 .UNSPECIFIED., .F., .F. ) 
 B_SPLINE_CURVE_WITH_KNOTS ( ( 4, 4 ),
 ( 1.570796326794938302, 3.141592653589793116 ),
 .UNSPECIFIED. ) 
 CURVE ( )  GEOMETRIC_REPRESENTATION_ITEM ( )  RATIONAL_B_SPLINE_CURVE ( ( 1.000000000000000000, 0.8047378541243747074, 0.8047378541243747074, 1.000000000000000000 ) ) 
 REPRESENTATION_ITEM ( '' )  );
#32573 = EDGE_CURVE ( 'NONE', #4816, #27974, #24351, .T. ) ;
#32574 = CARTESIAN_POINT ( 'NONE',  ( 9.500000000000005329, 57.08981371789855075, -0.1745138560723090149 ) ) ;
#32575 = CARTESIAN_POINT ( 'NONE',  ( 13.44051670066911797, -5.407089921784859143, -6.365624999385560479 ) ) ;
#32576 = CARTESIAN_POINT ( 'NONE',  ( 5.529263428287300108, 104.5273137178985650, 7.954856959092309943 ) ) ;
#32577 = CARTESIAN_POINT ( 'NONE',  ( -27.24356964374999990, 199.8218750006145399, -15.72908226750537786 ) ) ;
#32578 = CARTESIAN_POINT ( 'NONE',  ( 4.944772684328420986, 49.61481371789855643, 11.48171059495408208 ) ) ;
#32579 = CARTESIAN_POINT ( 'NONE',  ( 34.19561101691670757, -5.196152422706629359, 166.4053843532510371 ) ) ;
#32580 = CARTESIAN_POINT ( 'NONE',  ( 2.660918448318279950, 98.09768628210146346, -12.46528703574805697 ) ) ;
#32581 = CARTESIAN_POINT ( 'NONE',  ( 19.56230152254410726, 5.196152422706631135, -6.337499998771006560 ) ) ;
#32582 = EDGE_CURVE ( 'NONE', #4196, #28188, #14169, .T. ) ;
#32583 = CARTESIAN_POINT ( 'NONE',  ( -66.62872103062156270, 205.4690446883607535, 1.090244570138264368 ) ) ;
#32584 = CARTESIAN_POINT ( 'NONE',  ( -10.49813415415989581, 133.1726862821014663, -7.228626920339068285 ) ) ;
#32585 = CARTESIAN_POINT ( 'NONE',  ( 37.25116460488249004, -3.604726614523235284, 164.1147336928429468 ) ) ;
#32586 = AXIS2_PLACEMENT_3D ( 'NONE', #5467, #11355, #6028 ) ;
#32587 = CARTESIAN_POINT ( 'NONE',  ( -15.50000000000000533, 86.31018628210145494, -0.1745138560725808530 ) ) ;
#32588 = CARTESIAN_POINT ( 'NONE',  ( 22.80587116629411781, -3.604726614523238837, -3.609374999385538185 ) ) ;
#32589 = CARTESIAN_POINT ( 'NONE',  ( 22.60769515458673240, 248.3325961894322518, 6.000000000000000000 ) ) ;
#32590 = CARTESIAN_POINT ( 'NONE',  ( 24.00000000000000000, -5.196152422706629359, -4.799999999999998934 ) ) ;
#32591 = CYLINDRICAL_SURFACE ( 'NONE', #29662, 6.000000000000001776 ) ;
#32592 = CARTESIAN_POINT ( 'NONE',  ( -8.843639120294326972, 122.5351862821014493, 3.474262827703335166 ) ) ;
#32593 = CYLINDRICAL_SURFACE ( 'NONE', #23737, 5.999999999999999112 ) ;
#32594 = CARTESIAN_POINT ( 'NONE',  ( -10.83675517735155047, 4.660186282101435928, -11.08355503943142750 ) ) ;
#32595 = CARTESIAN_POINT ( 'NONE',  ( 13.62178482187499640, 195.2093750006145569, -23.59362340125807123 ) ) ;
#32596 = CARTESIAN_POINT ( 'NONE',  ( 21.00000000000000000, 241.7593750006145115, 6.646953231504538984 ) ) ;
#32597 = ORIENTED_EDGE ( 'NONE', *, *, #10840, .T. ) ;
#32598 = CARTESIAN_POINT ( 'NONE',  ( 34.41253136604939300, -5.407089921784855591, 167.4874711655023418 ) ) ;
#32599 = CARTESIAN_POINT ( 'NONE',  ( 21.00000000000000000, 6.646953231504538984, -2.953124999385479565 ) ) ;
#32600 = ADVANCED_FACE ( 'NONE', ( #36469 ), #11263, .T. ) ;
#32601 = CARTESIAN_POINT ( 'NONE',  ( -27.24356964375000345, 199.8593750006145342, 0.000000000000000000 ) ) ;
#32602 = DIRECTION ( 'NONE',  ( 0.1736605105622160139, 0.000000000000000000, 0.9848055783103945027 ) ) ;
#32603 = DIRECTION ( 'NONE',  ( 0.1219804832088915297, 0.9925324990730154395, 0.000000000000000000 ) ) ;
#32604 = CARTESIAN_POINT ( 'NONE',  ( 27.00000000000001421, 199.4000000012290457, 15.58845726811988897 ) ) ;
#32605 = LINE ( 'NONE', #386, #24253 ) ;
#32606 = CARTESIAN_POINT ( 'NONE',  ( -8.710071997420207879, 24.31481371789855217, 3.796722387233182339 ) ) ;
#32607 = CARTESIAN_POINT ( 'NONE',  ( 27.24356964375000700, 198.2468750006145513, 15.72908226750537075 ) ) ;
#32608 = CIRCLE ( 'NONE', #34421, 17.99999999999998934 ) ;
#32610 = ORIENTED_EDGE ( 'NONE', *, *, #27777, .T. ) ;
#32609 = EDGE_LOOP ( 'NONE', ( #14378, #16032, #4906, #17280 ) ) ;
#32611 = CARTESIAN_POINT ( 'NONE',  ( 15.24356964375000167, 247.0843750006145285, 3.323476615752272600 ) ) ;
#32612 = CARTESIAN_POINT ( 'NONE',  ( 8.715434833792128799, 28.33981371789855075, -8.962234695871567070 ) ) ;
#32613 = CARTESIAN_POINT ( 'NONE',  ( 21.00000000000000000, 6.646953231504538984, -1.153124999385464200 ) ) ;
#32614 = CARTESIAN_POINT ( 'NONE',  ( -15.46528703574811736, 135.0023137178985166, 3.257655550456946436 ) ) ;
#32615 = CARTESIAN_POINT ( 'NONE',  ( 24.00000000000000000, -5.196152422706629359, -6.993749998770947940 ) ) ;
#32616 = DIRECTION ( 'NONE',  ( 0.000000000000000000, -0.000000000000000000, -1.000000000000000000 ) ) ;
#32617 = EDGE_LOOP ( 'NONE', ( #29344, #5474, #24162, #17270 ) ) ;
#32618 = CARTESIAN_POINT ( 'NONE',  ( 13.44051670066910908, 5.407089921784862696, -6.571874999385523886 ) ) ;
#32619 = EDGE_CURVE ( 'NONE', #35077, #8427, #31350, .T. ) ;
#32620 = ORIENTED_EDGE ( 'NONE', *, *, #18763, .T. ) ;
#32621 = CARTESIAN_POINT ( 'NONE',  ( -27.24356964374999990, 197.5156250006145626, -15.72908226750537786 ) ) ;
#32622 = CARTESIAN_POINT ( 'NONE',  ( 37.29201885929546023, 3.604726614523243278, 164.5816999575734201 ) ) ;
#32623 = CARTESIAN_POINT ( 'NONE',  ( -30.99627896937850124, 203.4690446883607535, -1.626142955000504209 ) ) ;
#32624 = CARTESIAN_POINT ( 'NONE',  ( 15.24356964374999990, 249.2593750006145115, -3.323476615752268604 ) ) ;
#32625 =( LENGTH_UNIT ( ) NAMED_UNIT ( * ) SI_UNIT ( .MILLI., .METRE. ) );
#32626 = CARTESIAN_POINT ( 'NONE',  ( 1.069080835302379631E-14, 199.3250000012290286, 27.00000000000000000 ) ) ;
#32627 = CARTESIAN_POINT ( 'NONE',  ( -41.68377896937850124, 208.9097554298617183, 4.530955311639234040 ) ) ;
#32628 = CARTESIAN_POINT ( 'NONE',  ( 0.000000000000000000, 202.0000000000000000, 0.000000000000000000 ) ) ;
#32629 = CARTESIAN_POINT ( 'NONE',  ( 28.06852345636367119, -5.407089921784859143, 166.6120566704193493 ) ) ;
#32630 = ORIENTED_EDGE ( 'NONE', *, *, #19158, .T. ) ;
#32631 = CARTESIAN_POINT ( 'NONE',  ( -28.09635861911301546, 206.4454563690075588, 7.185930831749626435 ) ) ;
#32632 = CARTESIAN_POINT ( 'NONE',  ( 14.38691631536194393, 11.66481371789854293, 5.770363421894124656 ) ) ;
#32633 = CARTESIAN_POINT ( 'NONE',  ( -45.84747103062156981, 214.3500491399821044, -7.303452534266878793 ) ) ;
#32634 = CARTESIAN_POINT ( 'NONE',  ( 0.1745138560725194299, 125.4101862821014635, -9.500000000000005329 ) ) ;
#32635 = EDGE_CURVE ( 'NONE', #11078, #3622, #19067, .T. ) ;
#32636 = CARTESIAN_POINT ( 'NONE',  ( 11.61527771782819940, 35.13518628210143646, -4.622313124798573369 ) ) ;
#32637 = CARTESIAN_POINT ( 'NONE',  ( 16.56230152254411436, -6.928203230275514990, -7.087500000000036771 ) ) ;
#32638 = ORIENTED_EDGE ( 'NONE', *, *, #5005, .T. ) ;
#32639 = CARTESIAN_POINT ( 'NONE',  ( -34.76413769728823411, 213.1499508600178672, 5.686928522499718142 ) ) ;
#32640 = CARTESIAN_POINT ( 'NONE',  ( -14.25334919248782306, 123.6851862821014549, -6.092822981423979378 ) ) ;
#32641 = DIRECTION ( 'NONE',  ( 0.08715574274765150453, 0.000000000000000000, 0.9961946980917461003 ) ) ;
#32642 = CARTESIAN_POINT ( 'NONE',  ( 6.840914352311949109, 141.0398137178985678, 6.594114490232462877 ) ) ;
#32643 = CARTESIAN_POINT ( 'NONE',  ( -27.24356964375000345, 197.5531250006145285, 0.000000000000000000 ) ) ;
#32644 = PLANE ( 'NONE',  #26239 ) ;
#32645 = CARTESIAN_POINT ( 'NONE',  ( 3.306546357697854128E-15, 200.0000000000000000, 27.00000000000000355 ) ) ;
#32646 = EDGE_CURVE ( 'NONE', #21615, #15372, #12942, .T. ) ;
#32647 = CARTESIAN_POINT ( 'NONE',  ( 20.99999999999998579, 248.5374999999999659, -5.999999999999997335 ) ) ;
#32648 = CARTESIAN_POINT ( 'NONE',  ( 0.000000000000000000, 210.0000000000000284, -27.00000000000000000 ) ) ;
#32649 = CARTESIAN_POINT ( 'NONE',  ( 8.152565276336593669, 67.15231371789852233, 5.233372021372610483 ) ) ;
#32650 = CYLINDRICAL_SURFACE ( 'NONE', #7583, 27.00000000000000000 ) ;
#32651 = ORIENTED_EDGE ( 'NONE', *, *, #21739, .F. ) ;
#32652 = CARTESIAN_POINT ( 'NONE',  ( 24.00000000000000000, 243.0062500012290627, 5.196152422706629359 ) ) ;
#32653 = CARTESIAN_POINT ( 'NONE',  ( 11.48171059495408208, 84.11481371789855643, -4.944772684328420986 ) ) ;
#32654 = CARTESIAN_POINT ( 'NONE',  ( 13.44051670066910908, 5.407089921784862696, -4.771874999385556038 ) ) ;
#32655 = CARTESIAN_POINT ( 'NONE',  ( -13.16328360146172116, 143.0000000000000284, 4.685063460632339805 ) ) ;
#32656 = CARTESIAN_POINT ( 'NONE',  ( 26.75643035624999655, 7.049594010296217766E-16, -3.628124999385473615 ) ) ;
#32657 = CARTESIAN_POINT ( 'NONE',  ( 4.944772684328420986, 49.61481371789855643, 11.48171059495408208 ) ) ;
#32658 = CARTESIAN_POINT ( 'NONE',  ( 5.778771075727756162E-15, 197.2718750006145569, 31.45816453501075927 ) ) ;
#32659 = ORIENTED_EDGE ( 'NONE', *, *, #15166, .F. ) ;
#32660 = ORIENTED_EDGE ( 'NONE', *, *, #16912, .F. ) ;
#32661 = CARTESIAN_POINT ( 'NONE',  ( 20.99999999999999645, 6.646953231504538984, -4.303124999385466332 ) ) ;
#32662 = CARTESIAN_POINT ( 'NONE',  ( 15.24356964374999990, 243.8593750006145342, -3.323476615752268604 ) ) ;
#32663 = CARTESIAN_POINT ( 'NONE',  ( -10.69584247140444866, 48.64768628210144641, 6.932735513423972762 ) ) ;
#32664 = CARTESIAN_POINT ( 'NONE',  ( -32.38169563604517265, 210.1155267958017703, 6.500000000000000888 ) ) ;
#32665 = CARTESIAN_POINT ( 'NONE',  ( 22.80587116629411071, 3.604726614523238837, -1.228124999385522331 ) ) ;
#32666 = CARTESIAN_POINT ( 'NONE',  ( -62.46502896937850124, 215.5714017266979567, -3.350049139982168800 ) ) ;
#32667 = FACE_OUTER_BOUND ( 'NONE', #16274, .T. ) ;
#32668 = CARTESIAN_POINT ( 'NONE',  ( -6.932735513424201912, 87.85231371789855359, 10.69584247140429412 ) ) ;
#32669 = CARTESIAN_POINT ( 'NONE',  ( -46.63913769728824121, 207.8500491399821613, -3.954877714930864485 ) ) ;
#32670 = CARTESIAN_POINT ( 'NONE',  ( -32.19122103062156270, 207.8379586601371329, -8.530955311639223382 ) ) ;
#32671 = CARTESIAN_POINT ( 'NONE',  ( 18.12178482187500350, -4.985214923628407568, -6.478124999385492799 ) ) ;
#32672 = CARTESIAN_POINT ( 'NONE',  ( 22.56230152254411792, 7.347880794884125653E-16, -7.425000000000042455 ) ) ;
#32673 = CARTESIAN_POINT ( 'NONE',  ( 8.927990412390371944, 58.52731371789855785, 13.04141134922778811 ) ) ;
#32674 = CARTESIAN_POINT ( 'NONE',  ( -56.32961230271183695, 212.3930949314663792, 8.469044688360751749 ) ) ;
#32675 = AXIS2_PLACEMENT_3D ( 'NONE', #8590, #5548, #25834 ) ;
#32676 = CARTESIAN_POINT ( 'NONE',  ( 26.99999999999999645, 240.7749999999999773, -7.347880794884117764E-16 ) ) ;
#32677 = CARTESIAN_POINT ( 'NONE',  ( 10.49813415415989581, 91.77268628210144641, 7.228626920339068285 ) ) ;
#32678 = CARTESIAN_POINT ( 'NONE',  ( 15.53471296425195369, 35.42268628210144499, -2.908627838312120684 ) ) ;
#32679 = CARTESIAN_POINT ( 'NONE',  ( 19.56230152254412147, -5.196152422706635576, -0.3000000000000779821 ) ) ;
#32680 = CARTESIAN_POINT ( 'NONE',  ( 30.60810355289388696, 7.209453229046482114, 159.8211261399325736 ) ) ;
#32681 = CARTESIAN_POINT ( 'NONE',  ( 0.1745138560725837118, 51.81018628210144783, -15.50000000000000533 ) ) ;
#32682 = CARTESIAN_POINT ( 'NONE',  ( 13.62178482187499640, 197.8531250006145399, -23.59362340125807123 ) ) ;
#32683 = CARTESIAN_POINT ( 'NONE',  ( -47.00000000000000711, 244.5000000000000000, -0.4999999999999978351 ) ) ;
#32684 = DIRECTION ( 'NONE',  ( 0.000000000000000000, 0.000000000000000000, 1.000000000000000000 ) ) ;
#32685 = CARTESIAN_POINT ( 'NONE',  ( -39.31622103062156270, 211.6261429550005744, 6.530955311639227823 ) ) ;
#32686 = CARTESIAN_POINT ( 'NONE',  ( 2.999999999999997335, 244.5000000000000000, 0.000000000000000000 ) ) ;
#32687 = CARTESIAN_POINT ( 'NONE',  ( -12.46528703574805697, 12.99768628210143362, -2.660918448318280838 ) ) ;
#32688 = CYLINDRICAL_SURFACE ( 'NONE', #1431, 8.000000000000000000 ) ;
#32689 = CARTESIAN_POINT ( 'NONE',  ( 3.474262827703532341, 128.9648137178985792, -8.843639120294245259 ) ) ;
#32690 = CARTESIAN_POINT ( 'NONE',  ( 15.24356964374999990, 247.6093750006145342, 0.000000000000000000 ) ) ;
#32691 = VECTOR ( 'NONE', #3778, 1000.000000000000000 ) ;
#32692 = VERTEX_POINT ( 'NONE', #4636 ) ;
#32693 = CARTESIAN_POINT ( 'NONE',  ( 18.00000000000000000, 5.196152422706630247, -5.925000000000013145 ) ) ;
#32694 = CARTESIAN_POINT ( 'NONE',  ( 18.00000000000000355, 245.1812500012290457, 5.196152422706632912 ) ) ;
#32695 = CARTESIAN_POINT ( 'NONE',  ( 26.99999999999999645, 7.347880794884117764E-16, -6.918749998770956644 ) ) ;
#32696 = CARTESIAN_POINT ( 'NONE',  ( 10.31873187879411091, 3.604726614523236616, -6.478124999385515004 ) ) ;
#32697 = CARTESIAN_POINT ( 'NONE',  ( 37.33614145406145468, 3.604726614523238837, 165.0860235234823392 ) ) ;
#32698 = CARTESIAN_POINT ( 'NONE',  ( 1.069080835302379631E-14, 195.2750000012290457, 27.00000000000000000 ) ) ;
#32699 = CARTESIAN_POINT ( 'NONE',  ( 0.000000000000000000, 200.0000000000000000, -27.00000000000000355 ) ) ;
#32700 = EDGE_CURVE ( 'NONE', #26583, #29410, #20821, .T. ) ;
#32701 = CARTESIAN_POINT ( 'NONE',  ( -12.53471296425194659, 58.42268628210145209, 2.311890736173176641 ) ) ;
#32702 = ORIENTED_EDGE ( 'NONE', *, *, #33040, .T. ) ;
#32703 = ORIENTED_EDGE ( 'NONE', *, *, #14005, .T. ) ;
#32704 = CARTESIAN_POINT ( 'NONE',  ( 20.99999999999999645, 185.0294372515228645, 0.000000000000000000 ) ) ;
#32705 = CARTESIAN_POINT ( 'NONE',  ( 19.56230152254412502, -5.196152422706635576, -3.900000000000070077 ) ) ;
#32706 = CARTESIAN_POINT ( 'NONE',  ( 26.99999999999999645, 246.6625000000000227, -3.464101615137755275 ) ) ;
#32707 = CARTESIAN_POINT ( 'NONE',  ( -79.74198084750223359, 216.3821266856691636, 5.000000000000000000 ) ) ;
#32708 = CARTESIAN_POINT ( 'NONE',  ( 15.24356964374999990, 3.323476615752268604, -9.178124999385456562 ) ) ;
#32709 = VECTOR ( 'NONE', #3791, 1000.000000000000000 ) ;
#32710 = CARTESIAN_POINT ( 'NONE',  ( -4.944772684328673229, 93.78518628210144925, 11.48171059495397728 ) ) ;
#32711 = CARTESIAN_POINT ( 'NONE',  ( -6.092822981423666739, 26.61481371789854933, -14.25334919248795096 ) ) ;
#32712 = CARTESIAN_POINT ( 'NONE',  ( 13.56230152254411614, -5.196152422706638241, -5.775000000000085620 ) ) ;
#32713 = CARTESIAN_POINT ( 'NONE',  ( 21.00000000000000000, 243.8687500012290172, 5.999999999999998224 ) ) ;
#32714 = CARTESIAN_POINT ( 'NONE',  ( -64.24627896937850835, 205.4690446883607535, -1.090244570138286351 ) ) ;
#32715 = CARTESIAN_POINT ( 'NONE',  ( 20.99999999999997513, 245.3875000000000455, -5.999999999999999112 ) ) ;
#32716 = CARTESIAN_POINT ( 'NONE',  ( 31.22336862440664618, 6.928203230275506996, 166.8536380873862015 ) ) ;
#32717 = CARTESIAN_POINT ( 'NONE',  ( -12.46528703574811558, 135.0023137178985735, 2.660918448318003726 ) ) ;
#32718 = CARTESIAN_POINT ( 'NONE',  ( -45.05580436395489841, 216.5000000000000000, 0.1155267958017343610 ) ) ;
#32719 = EDGE_CURVE ( 'NONE', #5744, #8565, #11074, .T. ) ;
#32720 = CARTESIAN_POINT ( 'NONE',  ( -68.21205436395490551, 216.1378603801730094, 6.307003348497944195 ) ) ;
#32721 = APPLICATION_PROTOCOL_DEFINITION ( 'draft international standard', 'automotive_design', 1998, #34708 ) ;
#32722 = VECTOR ( 'NONE', #25974, 1000.000000000000000 ) ;
#32723 = DIRECTION ( 'NONE',  ( -0.08715574274766001162, -2.055968571607451078E-14, -0.9961946980917453232 ) ) ;
#32724 = CARTESIAN_POINT ( 'NONE',  ( -13.62178482187500528, 198.3781250006145171, -23.59362340125807123 ) ) ;
#32725 = CARTESIAN_POINT ( 'NONE',  ( -11.08355503943118592, 108.8398137178985507, -10.83675517735179383 ) ) ;
#32726 = CARTESIAN_POINT ( 'NONE',  ( -62.86086230271182984, 213.1499508600178387, -5.686928522499747451 ) ) ;
#32727 = VERTEX_POINT ( 'NONE', #16215 ) ;
#32728 = CARTESIAN_POINT ( 'NONE',  ( -2.311890736173176641, 23.92268628210143788, -12.53471296425194836 ) ) ;
#32729 = CARTESIAN_POINT ( 'NONE',  ( 19.39230484541324984, 244.7486538117967143, 5.999999999999991118 ) ) ;
#32730 = DIRECTION ( 'NONE',  ( -1.000000000000000000, -0.000000000000000000, -0.000000000000000000 ) ) ;
#32731 = CARTESIAN_POINT ( 'NONE',  ( 25.10732745429168489, -3.604726614523244610, 168.5838953488872676 ) ) ;
#32732 = CARTESIAN_POINT ( 'NONE',  ( 13.23911966647218996, 99.24768628210145494, -8.632099005475504683 ) ) ;
#32733 = PRESENTATION_STYLE_ASSIGNMENT (( #11341 ) ) ;
#32734 = CARTESIAN_POINT ( 'NONE',  ( 13.44051670066911086, 5.407089921784856479, -5.165624999385554084 ) ) ;
#32735 =( BOUNDED_CURVE ( )  B_SPLINE_CURVE ( 2, ( #3252, #20895, #14826, #588, #12157, #23543, #26371 ),
 .UNSPECIFIED., .F., .F. ) 
 B_SPLINE_CURVE_WITH_KNOTS ( ( 3, 2, 2, 3 ),
 ( 0.4130434782608686795, 0.4202898550724629700, 0.4275362318840572606, 0.4347826086956515512 ),
 .UNSPECIFIED. ) 
 CURVE ( )  GEOMETRIC_REPRESENTATION_ITEM ( )  RATIONAL_B_SPLINE_CURVE ( ( 1.000000000000016431, 0.8660254037844222763, 1.000000000000000000, 0.8660254037844387076, 1.000000000000000000, 0.8660254037844500319, 0.9999999999999886757 ) ) 
 REPRESENTATION_ITEM ( '' )  );
#32736 = CARTESIAN_POINT ( 'NONE',  ( 3.474262827703335166, 65.03518628210144925, 8.843639120294326972 ) ) ;
#32737 = CARTESIAN_POINT ( 'NONE',  ( 18.00000000000000000, 240.5312500012290400, -5.196152422706630247 ) ) ;
#32738 = CARTESIAN_POINT ( 'NONE',  ( -43.27455436395490551, 203.6929966515020283, 6.137860380172978303 ) ) ;
#32739 = FACE_BOUND ( 'NONE', #22607, .T. ) ;
#32740 = CARTESIAN_POINT ( 'NONE',  ( 7.228626920339068285, 80.27268628210146062, -10.49813415415989581 ) ) ;
#32741 = CARTESIAN_POINT ( 'NONE',  ( 19.56230152254412502, 5.196152422706637353, -5.100000000000049383 ) ) ;
#32742 = DIRECTION ( 'NONE',  ( 1.000000000000000000, 0.000000000000000000, -0.000000000000000000 ) ) ;
#32744 = VERTEX_POINT ( 'NONE', #7866 ) ;
#32743 = CARTESIAN_POINT ( 'NONE',  ( 3.474262827703335166, 46.63518628210144357, 8.843639120294326972 ) ) ;
#32745 = CARTESIAN_POINT ( 'NONE',  ( 26.99999999999999645, 7.347880794884117764E-16, -1.068749998770962550 ) ) ;
#32746 = CARTESIAN_POINT ( 'NONE',  ( 15.00000000000000000, 3.464101615137752166, -0.9375000000000204281 ) ) ;
#32747 = CARTESIAN_POINT ( 'NONE',  ( 16.56230152254411081, -6.928203230275514990, -6.637500000000041034 ) ) ;
#32748 = CARTESIAN_POINT ( 'NONE',  ( 24.86547026816695904, 3.604726614523240613, 165.8194550616826461 ) ) ;
#32749 = CARTESIAN_POINT ( 'NONE',  ( 36.94233792496010693, -3.464101615137755275, 163.3794768365791583 ) ) ;
#32750 = CARTESIAN_POINT ( 'NONE',  ( 26.99999999999999645, 247.0374999999999943, 3.464101615137751278 ) ) ;
#32751 = CARTESIAN_POINT ( 'NONE',  ( 5.778771075727756162E-15, 196.3156250006145171, 31.45816453501076637 ) ) ;
#32752 = CARTESIAN_POINT ( 'NONE',  ( -4.944772684328424539, 100.2148137178985650, -11.48171059495408031 ) ) ;
#32753 = CARTESIAN_POINT ( 'NONE',  ( -8.962234695871760692, 103.5601862821014549, 8.715434833791933400 ) ) ;
#32754 = ORIENTED_EDGE ( 'NONE', *, *, #5020, .F. ) ;
#32755 = AXIS2_PLACEMENT_3D ( 'NONE', #23878, #18382, #29932 ) ;
#32756 = EDGE_LOOP ( 'NONE', ( #5700, #31957, #52, #8935 ) ) ;
#32757 = CARTESIAN_POINT ( 'NONE',  ( -13.50000000000000533, 199.5875000012290457, -23.38268590217984411 ) ) ;
#32758 = CARTESIAN_POINT ( 'NONE',  ( 18.12178482187500350, 239.9218750006145058, 4.985214923628407568 ) ) ;
#32759 = CARTESIAN_POINT ( 'NONE',  ( 15.50000000000000533, 84.68981371789855928, -0.1745138560722452326 ) ) ;
#32760 = CARTESIAN_POINT ( 'NONE',  ( 21.00000000000000000, -6.646953231504538984, -5.540624999385494576 ) ) ;
#32761 = CARTESIAN_POINT ( 'NONE',  ( 23.87821517812499650, 245.6593750006145171, -4.985214923628404904 ) ) ;
#32762 =( BOUNDED_CURVE ( )  B_SPLINE_CURVE ( 2, ( #37091, #16654, #16839, #22716, #28379, #27828, #7559 ),
 .UNSPECIFIED., .F., .F. ) 
 B_SPLINE_CURVE_WITH_KNOTS ( ( 3, 2, 2, 3 ),
 ( 0.6956521739130446802, 0.7028985507246381381, 0.7101449275362315960, 0.7173913043478249429 ),
 .UNSPECIFIED. ) 
 CURVE ( )  GEOMETRIC_REPRESENTATION_ITEM ( )  RATIONAL_B_SPLINE_CURVE ( ( 0.9999999999999774625, 0.8660254037844612451, 1.000000000000000000, 0.8660254037844387076, 1.000000000000000000, 0.8660254037844592467, 0.9999999999999794609 ) ) 
 REPRESENTATION_ITEM ( '' )  );
#32763 = CARTESIAN_POINT ( 'NONE',  ( -8.152565276336710909, 103.8476862821014493, 5.233372021372435512 ) ) ;
#32764 = CARTESIAN_POINT ( 'NONE',  ( 20.99999999999999289, 243.1937500012290343, -5.999999999999997335 ) ) ;
#32765 = CARTESIAN_POINT ( 'NONE',  ( -8.152565276336593669, 62.55231371789854222, -5.233372021372610483 ) ) ;
#32766 = CARTESIAN_POINT ( 'NONE',  ( 22.80587116629410360, 3.604726614523238837, -4.828124999385519978 ) ) ;
#32767 = EDGE_CURVE ( 'NONE', #17657, #32139, #11724, .T. ) ;
#32768 = CARTESIAN_POINT ( 'NONE',  ( -2.064181346179062349, 118.9023137178985650, -9.465287035748106703 ) ) ;
#32769 = CARTESIAN_POINT ( 'NONE',  ( 15.24356964374999990, 240.2593750006144830, -3.323476615752268604 ) ) ;
#32770 = CARTESIAN_POINT ( 'NONE',  ( 8.715434833792128799, 28.33981371789855075, -8.962234695871567070 ) ) ;
#32771 = DIRECTION ( 'NONE',  ( 0.000000000000000000, -0.000000000000000000, -1.000000000000000000 ) ) ;
#32772 = CARTESIAN_POINT ( 'NONE',  ( -12.46528703574805697, 86.59768628210144925, -2.660918448318280838 ) ) ;
#32773 = CARTESIAN_POINT ( 'NONE',  ( 22.56230152254410370, 7.347880794884117764E-16, -5.512499998771014376 ) ) ;
#32774 = CARTESIAN_POINT ( 'NONE',  ( 15.00000000000000000, 0.000000000000000000, -0.3937499987709536242 ) ) ;
#32775 = CARTESIAN_POINT ( 'NONE',  ( 34.05955060792140188, -5.407089921784855591, 163.4528826382307614 ) ) ;
#32776 = CARTESIAN_POINT ( 'NONE',  ( 10.83675517735155225, 82.86018628210146630, 11.08355503943142573 ) ) ;
#32777 = CARTESIAN_POINT ( 'NONE',  ( 22.80587116629412137, 7.646167579472024665E-16, -3.571874999385521221 ) ) ;
#32778 = CARTESIAN_POINT ( 'NONE',  ( 16.56230152254411081, 6.928203230275506996, -3.149999998770972365 ) ) ;
#32779 = PLANE ( 'NONE',  #18862 ) ;
#32780 = CARTESIAN_POINT ( 'NONE',  ( 25.36386068845838082, 0.000000000000000000, 168.7214353850716293 ) ) ;
#32781 = CARTESIAN_POINT ( 'NONE',  ( 8.843639120294328748, 117.9351862821014407, -3.474262827703334722 ) ) ;
#32782 = CARTESIAN_POINT ( 'NONE',  ( 18.00000000000000000, 5.196152422706630247, -2.268749998770941190 ) ) ;
#32783 = CARTESIAN_POINT ( 'NONE',  ( 10.69584247140445221, 126.8476862821014635, -6.932735513423970097 ) ) ;
#32784 = APPLICATION_CONTEXT ( 'automotive_design' ) ;
#32785 = CARTESIAN_POINT ( 'NONE',  ( 5.778771075727756162E-15, 195.4718750006145456, 31.45816453501075927 ) ) ;
#32786 = CARTESIAN_POINT ( 'NONE',  ( 23.87821517812499650, 240.1468750006145285, -4.985214923628404904 ) ) ;
#32787 = ORIENTED_EDGE ( 'NONE', *, *, #17824, .T. ) ;
#32788 = CARTESIAN_POINT ( 'NONE',  ( 37.53224187524366329, 3.604726614523238837, 167.3274615941888044 ) ) ;
#32789 = CARTESIAN_POINT ( 'NONE',  ( 26.75643035624999655, 7.049594010296217766E-16, -2.165624999385467930 ) ) ;
#32790 = ADVANCED_FACE ( 'NONE', ( #30798 ), #34960, .T. ) ;
#32791 = CARTESIAN_POINT ( 'NONE',  ( 26.99999999999999645, 242.6125000000000114, -3.464101615137755275 ) ) ;
#32792 = CARTESIAN_POINT ( 'NONE',  ( 20.99999999999999645, 185.0294372515228645, 5.999999999999999112 ) ) ;
#32793 = DIRECTION ( 'NONE',  ( 1.000000000000000000, 0.000000000000000000, 0.000000000000000000 ) ) ;
#32794 = CARTESIAN_POINT ( 'NONE',  ( 13.44051670066911086, 5.407089921784856479, -0.2156249993855441360 ) ) ;
#32795 = CARTESIAN_POINT ( 'NONE',  ( 9.534712964251900402, 20.57731371789854435, 1.715153634034445540 ) ) ;
#32796 = CARTESIAN_POINT ( 'NONE',  ( -27.24356964375000345, 198.0218750006145569, -15.72908226750537786 ) ) ;
#32798 = ORIENTED_EDGE ( 'NONE', *, *, #34596, .T. ) ;
#32797 = VERTEX_POINT ( 'NONE', #28693 ) ;
#32799 = CARTESIAN_POINT ( 'NONE',  ( 26.75643035624999655, 247.3093750006144944, -3.323476615752271712 ) ) ;
#32800 = CARTESIAN_POINT ( 'NONE',  ( -0.1745138560722763466, 17.98981371789853867, -12.50000000000000355 ) ) ;
#32801 = CARTESIAN_POINT ( 'NONE',  ( 18.12178482187499640, 4.985214923628404904, -2.465624999385462868 ) ) ;
#32802 = CARTESIAN_POINT ( 'NONE',  ( 13.23911966647199812, 131.5523137178985564, 8.632099005475788900 ) ) ;
#32803 = CARTESIAN_POINT ( 'NONE',  ( 21.00000000000000000, -6.928203230275506996, -8.381249998770950782 ) ) ;
#32804 = CARTESIAN_POINT ( 'NONE',  ( 10.49999999999999645, 244.5000000000000000, 5.000000000000000000 ) ) ;
#32805 = VERTEX_POINT ( 'NONE', #10709 ) ;
#32806 = CARTESIAN_POINT ( 'NONE',  ( 16.56230152254411436, -7.209453229046482114, -6.384374999385507010 ) ) ;
#32807 = CARTESIAN_POINT ( 'NONE',  ( 13.62178482187499640, 195.6031250006145115, -23.59362340125807123 ) ) ;
#32808 = CARTESIAN_POINT ( 'NONE',  ( 7.228626920339068285, 135.4726862821014493, -10.49813415415989581 ) ) ;
#32809 = CARTESIAN_POINT ( 'NONE',  ( 27.82830044041545747, -5.407089921784865361, 163.8662950338039650 ) ) ;
#32810 = CARTESIAN_POINT ( 'NONE',  ( -60.09002896937850124, 202.6965474657332038, 4.350049139982197666 ) ) ;
#32811 = CARTESIAN_POINT ( 'NONE',  ( 20.99999999999999645, 247.8343750006144717, -6.646953231504538984 ) ) ;
#32812 = LINE ( 'NONE', #23921, #6724 ) ;
#32813 = CARTESIAN_POINT ( 'NONE',  ( -48.41294563604517265, 213.2096571498974527, -3.378800118222469617 ) ) ;
#32814 = CARTESIAN_POINT ( 'NONE',  ( 10.69584247140445221, 136.0476862821014379, -6.932735513423970097 ) ) ;
#32815 = CARTESIAN_POINT ( 'NONE',  ( 31.24052741120653209, 7.209453229046475009, 167.0497639179608313 ) ) ;
#32816 = ORIENTED_EDGE ( 'NONE', *, *, #10261, .T. ) ;
#32817 = CARTESIAN_POINT ( 'NONE',  ( 20.99999999999998579, 248.1437500012290229, -5.999999999999997335 ) ) ;
#32818 = CARTESIAN_POINT ( 'NONE',  ( -15.50000000000000533, 132.3101862821014549, -0.1745138560725808530 ) ) ;
#32819 = CARTESIAN_POINT ( 'NONE',  ( -44.65997103062156981, 217.3034525342668815, 4.350049139982096413 ) ) ;
#32820 = CARTESIAN_POINT ( 'NONE',  ( -0.1745138560725182642, 120.8101862821014691, 9.500000000000005329 ) ) ;
#32821 = CARTESIAN_POINT ( 'NONE',  ( 0.000000000000000000, 143.0000000000000000, 0.000000000000000000 ) ) ;
#32822 = CARTESIAN_POINT ( 'NONE',  ( 11.48171059495397728, 36.28518628210144925, 4.944772684328674117 ) ) ;
#32823 = CARTESIAN_POINT ( 'NONE',  ( 16.56230152254411436, 6.928203230275514990, -7.762500000000014388 ) ) ;
#32824 = UNCERTAINTY_MEASURE_WITH_UNIT (LENGTH_MEASURE( 1.000000000000000082E-05 ), #13710, 'distance_accuracy_value', 'NONE');
#32825 = ORIENTED_EDGE ( 'NONE', *, *, #19589, .T. ) ;
#32826 = CARTESIAN_POINT ( 'NONE',  ( -34.17038769728823411, 208.1428034533959703, 6.469044688360771289 ) ) ;
#32827 = CARTESIAN_POINT ( 'NONE',  ( 8.632099005475504683, 119.9476862821014294, 13.23911966647218996 ) ) ;
#32828 = CARTESIAN_POINT ( 'NONE',  ( -47.00000000000000711, 237.0000000000000000, 5.000000000000000000 ) ) ;
#32829 = CARTESIAN_POINT ( 'NONE',  ( -2.064181346179062349, 137.3023137178985564, -9.465287035748106703 ) ) ;
#32830 = CARTESIAN_POINT ( 'NONE',  ( 27.24356964375000345, 198.2281250006145399, -3.336375036156643733E-15 ) ) ;
#32831 = CARTESIAN_POINT ( 'NONE',  ( 16.56230152254410726, 0.000000000000000000, 10.00000000000000000 ) ) ;
#32832 = CARTESIAN_POINT ( 'NONE',  ( -26.99999999999998934, 195.5374999999999943, 15.58845726811991561 ) ) ;
#32833 = CARTESIAN_POINT ( 'NONE',  ( 15.26155779561005232, -6.106572496351636126, -10.00000000000000000 ) ) ;
#32834 = CARTESIAN_POINT ( 'NONE',  ( 15.07120214184183737, -0.2399139898622077993, -8.000000000000019540 ) ) ;
#32835 = CARTESIAN_POINT ( 'NONE',  ( 24.77229108455811257, 3.464101615137419543, 161.9597638717738732 ) ) ;
#32836 = CARTESIAN_POINT ( 'NONE',  ( 5.529263428287300108, 76.92731371789854222, 7.954856959092309943 ) ) ;
#32837 = FACE_OUTER_BOUND ( 'NONE', #36687, .T. ) ;
#32838 = EDGE_LOOP ( 'NONE', ( #37347, #23336, #15045, #17751 ) ) ;
#32839 = CARTESIAN_POINT ( 'NONE',  ( 21.00000000000000000, 242.9687500012290684, 6.928203230275506996 ) ) ;
#32840 = CARTESIAN_POINT ( 'NONE',  ( -11.48171059495408208, 88.71481371789855075, 4.944772684328421875 ) ) ;
#32841 = CARTESIAN_POINT ( 'NONE',  ( 22.80587116629411781, -3.604726614523238837, -3.609374999385538185 ) ) ;
#32842 = LINE ( 'NONE', #10102, #20955 ) ;
#32843 = CARTESIAN_POINT ( 'NONE',  ( 18.12178482187500350, -4.985214923628407568, -4.678124999385496530 ) ) ;
#32844 = CARTESIAN_POINT ( 'NONE',  ( 12.53471296425189330, 38.97731371789855359, 2.311890736173451977 ) ) ;
#32845 = ORIENTED_EDGE ( 'NONE', *, *, #5020, .T. ) ;
#32846 = CARTESIAN_POINT ( 'NONE',  ( 26.75643035624999655, -3.323476615752267271, -6.703124999385464911 ) ) ;
#32847 = CARTESIAN_POINT ( 'NONE',  ( 23.87821517812499650, 244.1968750006145115, -4.985214923628404904 ) ) ;
#32848 = CARTESIAN_POINT ( 'NONE',  ( -2.660918448318275509, 19.89768628210143575, 12.46528703574805874 ) ) ;
#32849 = VECTOR ( 'NONE', #33740, 1000.000000000000000 ) ;
#32850 = CARTESIAN_POINT ( 'NONE',  ( -35.54836230271183695, 204.3130714775002446, -3.149950860017828091 ) ) ;
#32851 = CARTESIAN_POINT ( 'NONE',  ( -61.27752896937850124, 213.3500491399821613, 5.571401726697954970 ) ) ;
#32852 = FILL_AREA_STYLE ('',( #35507 ) ) ;
#32853 = CARTESIAN_POINT ( 'NONE',  ( 33.68574992184294103, -5.196152422706629359, 160.5776453694143129 ) ) ;
#32854 = CARTESIAN_POINT ( 'NONE',  ( -12.46528703574811558, 89.00231371789855928, 2.660918448318003726 ) ) ;
#32855 = EDGE_CURVE ( 'NONE', #31903, #14365, #16600, .T. ) ;
#32856 = CARTESIAN_POINT ( 'NONE',  ( -43.27455436395490551, 206.6211998817774997, 3.209657149897401585 ) ) ;
#32858 = ADVANCED_FACE ( 'NONE', ( #14304 ), #21923, .F. ) ;
#32857 = CARTESIAN_POINT ( 'NONE',  ( -68.01413769728823411, 213.1499508600178672, 5.686928522499718142 ) ) ;
#32859 =( BOUNDED_CURVE ( )  B_SPLINE_CURVE ( 2, ( #6560, #27026, #12054, #23626, #32143, #18135, #18517, #18322, #29489 ),
 .UNSPECIFIED., .F., .F. ) 
 B_SPLINE_CURVE_WITH_KNOTS ( ( 3, 2, 2, 2, 3 ),
 ( 0.1630434782608695676, 0.1666666666666666574, 0.1739130434782608647, 0.1811594202898550721, 0.1847826086956521618 ),
 .UNSPECIFIED. ) 
 CURVE ( )  GEOMETRIC_REPRESENTATION_ITEM ( )  RATIONAL_B_SPLINE_CURVE ( ( 0.9330127018922194093, 0.9330127018922196314, 1.000000000000000000, 0.8660254037844387076, 1.000000000000000000, 0.8660254037844387076, 1.000000000000000000, 0.9330127018922196314, 0.9330127018922194093 ) ) 
 REPRESENTATION_ITEM ( '' )  );
#32860 =( GEOMETRIC_REPRESENTATION_CONTEXT ( 3 ) GLOBAL_UNCERTAINTY_ASSIGNED_CONTEXT ( ( #26571 ) ) GLOBAL_UNIT_ASSIGNED_CONTEXT ( ( #37252, #36700, #28172 ) ) REPRESENTATION_CONTEXT ( 'NONE', 'WORKASPACE' ) );
#32861 = CARTESIAN_POINT ( 'NONE',  ( 26.75643035624999655, 3.323476615752271268, -7.640624999385485339 ) ) ;
#32862 = CARTESIAN_POINT ( 'NONE',  ( 16.56230152254411792, 6.928203230275514990, -7.312500000000050626 ) ) ;
#32863 = CARTESIAN_POINT ( 'NONE',  ( -15.53471296425188442, 52.77731371789855785, -2.908627838312459080 ) ) ;
#32864 = CARTESIAN_POINT ( 'NONE',  ( -42.07961230271182984, 212.3930949314663792, 8.469044688360751749 ) ) ;
#32865 =( GEOMETRIC_REPRESENTATION_CONTEXT ( 3 ) GLOBAL_UNCERTAINTY_ASSIGNED_CONTEXT ( ( #15782 ) ) GLOBAL_UNIT_ASSIGNED_CONTEXT ( ( #10665, #25070, #10853 ) ) REPRESENTATION_CONTEXT ( 'NONE', 'WORKASPACE' ) );
#32866 = CARTESIAN_POINT ( 'NONE',  ( -10.69584247140444866, 94.64768628210146062, 6.932735513423972762 ) ) ;
#32867 = CARTESIAN_POINT ( 'NONE',  ( -15.46528703574804986, 31.39768628210144286, -3.257655550457287497 ) ) ;
#32869 = EDGE_CURVE ( 'NONE', #3429, #36284, #29651, .T. ) ;
#32868 = DIRECTION ( 'NONE',  ( 0.08715574274765150453, 0.000000000000000000, 0.9961946980917461003 ) ) ;
#32870 = CARTESIAN_POINT ( 'NONE',  ( 20.99999999999999645, 185.0294372515228645, 0.000000000000000000 ) ) ;
#32871 = EDGE_LOOP ( 'NONE', ( #17333, #22589 ) ) ;
#32872 = CARTESIAN_POINT ( 'NONE',  ( 3.257655550457285720, 42.89768628210143220, -15.46528703574804986 ) ) ;
#32873 = CARTESIAN_POINT ( 'NONE',  ( 27.24356964374999279, 197.3656250006145285, -15.72908226750539207 ) ) ;
#32874 = CARTESIAN_POINT ( 'NONE',  ( -77.00000000000002842, 210.0000000000000000, 2.500000000000001332 ) ) ;
#32875 = CARTESIAN_POINT ( 'NONE',  ( 22.56230152254392252, -3.464101615137877843, -2.512500000000024158 ) ) ;
#32876 = CARTESIAN_POINT ( 'NONE',  ( -35.55580436395490551, 216.5000000000000000, 0.1155267958017343610 ) ) ;
#32877 = CARTESIAN_POINT ( 'NONE',  ( -78.53013030854349097, 228.3413836382483169, 5.000000000000000000 ) ) ;
#32878 = CARTESIAN_POINT ( 'NONE',  ( 2.311890736173175753, 19.32268628210144712, 12.53471296425194836 ) ) ;
#32879 = DIRECTION ( 'NONE',  ( 0.000000000000000000, -1.000000000000000000, 0.000000000000000000 ) ) ;
#32880 = CARTESIAN_POINT ( 'NONE',  ( 7.954856959092311719, 139.0273137178985507, -5.529263428287300108 ) ) ;
#32881 = CARTESIAN_POINT ( 'NONE',  ( 20.99999999999999645, 244.1218750006145228, 6.646953231504538984 ) ) ;
#32882 = ORIENTED_EDGE ( 'NONE', *, *, #34481, .T. ) ;
#32883 = CARTESIAN_POINT ( 'NONE',  ( 18.00000000000000355, -5.196152422706632912, -7.124999999999992895 ) ) ;
#32884 = LINE ( 'NONE', #12795, #30530 ) ;
#32885 = CARTESIAN_POINT ( 'NONE',  ( 11.61527771782809637, 131.2648137178985621, 4.622313124798827388 ) ) ;
#32886 = CARTESIAN_POINT ( 'NONE',  ( 16.56230152254411081, 7.209453229046475009, -5.653124999385517491 ) ) ;
#32887 = CARTESIAN_POINT ( 'NONE',  ( 24.79846929092969887, -3.604726614523240613, 165.0536303875245778 ) ) ;
#32888 = CARTESIAN_POINT ( 'NONE',  ( 15.00000000000000000, 0.000000000000000000, -1.799999999999996048 ) ) ;
#32889 = CARTESIAN_POINT ( 'NONE',  ( -27.00000000000000355, 199.0625000000000000, -15.58845726811989429 ) ) ;
#32890 = CARTESIAN_POINT ( 'NONE',  ( -0.1745138560725500443, 56.41018628210145636, 12.50000000000000355 ) ) ;
#32891 = VERTEX_POINT ( 'NONE', #12249 ) ;
#32892 = ORIENTED_EDGE ( 'NONE', *, *, #31372, .T. ) ;
#32893 = CYLINDRICAL_SURFACE ( 'NONE', #6114, 5.999999999999994671 ) ;
#32894 = CARTESIAN_POINT ( 'NONE',  ( 18.12178482187499640, 4.985214923628404904, -0.6656249993854668201 ) ) ;
#32895 = CARTESIAN_POINT ( 'NONE',  ( 22.60769515458673595, 249.4736538117967370, -6.000000000000001776 ) ) ;
#32896 = DIRECTION ( 'NONE',  ( -0.000000000000000000, -1.000000000000000000, -0.000000000000000000 ) ) ;
#32897 = CARTESIAN_POINT ( 'NONE',  ( 23.87821517812499650, 4.985214923628404904, -8.390624999385476457 ) ) ;
#32898 = CARTESIAN_POINT ( 'NONE',  ( -2.660918448318275509, 75.09768628210143504, 12.46528703574805874 ) ) ;
#32899 = CARTESIAN_POINT ( 'NONE',  ( 8.632099005475788900, 18.85231371789855359, -13.23911966647199812 ) ) ;
#32900 = CARTESIAN_POINT ( 'NONE',  ( 24.78536444607796341, 0.000000000000000000, 162.1091930777120069 ) ) ;
#32901 = CARTESIAN_POINT ( 'NONE',  ( 10.42677199038629787, 213.9649605036052833, 4.520320870633288912 ) ) ;
#32902 = CARTESIAN_POINT ( 'NONE',  ( -61.87127896937851546, 214.5309553116392749, 1.090244570138288127 ) ) ;
#32903 = CARTESIAN_POINT ( 'NONE',  ( -79.65000000000001990, 210.0000000000000000, 5.000000000000000000 ) ) ;
#32904 = CARTESIAN_POINT ( 'NONE',  ( 37.23322021648748859, 3.464101615137755275, 166.7042766426846754 ) ) ;
#32905 = CARTESIAN_POINT ( 'NONE',  ( -4.944772684328424539, 137.0148137178985621, -11.48171059495408031 ) ) ;
#32906 = CARTESIAN_POINT ( 'NONE',  ( -44.26413769728823411, 213.1499508600178672, 5.686928522499718142 ) ) ;
#32907 = CARTESIAN_POINT ( 'NONE',  ( -31.39211230271183339, 201.5309553116392181, 2.393094931466368980 ) ) ;
#32908 = PRODUCT_CONTEXT ( 'NONE', #3496, 'mechanical' ) ;
#32909 = CARTESIAN_POINT ( 'NONE',  ( 36.75277418448325761, 3.464101615138157619, 161.2127533682296416 ) ) ;
#32910 = CARTESIAN_POINT ( 'NONE',  ( -13.62178482187498396, 198.0781250006145342, 23.59362340125808188 ) ) ;
#32911 = CARTESIAN_POINT ( 'NONE',  ( 0.1745138560722461762, 114.5898137178985650, 15.50000000000000533 ) ) ;
#32912 = CARTESIAN_POINT ( 'NONE',  ( -45.24627896937850835, 203.4690446883607535, -1.626142955000504209 ) ) ;
#32913 = ORIENTED_EDGE ( 'NONE', *, *, #33185, .F. ) ;
#32914 = CARTESIAN_POINT ( 'NONE',  ( -11.61527771782819940, 30.53518628210144570, 4.622313124798574258 ) ) ;
#32915 = CARTESIAN_POINT ( 'NONE',  ( 19.39230484541326049, 244.5638461906613657, -5.999999999999997335 ) ) ;
#32916 = CARTESIAN_POINT ( 'NONE',  ( 26.97716818855048260, 0.000000000000000000, 49.47706554351410801 ) ) ;
#32917 = CARTESIAN_POINT ( 'NONE',  ( 34.25074851857407765, -5.407089921784861808, 165.6382847571695436 ) ) ;
#32918 = PRESENTATION_LAYER_ASSIGNMENT (  '', '', ( #37159 ) ) ;
#32919 = CARTESIAN_POINT ( 'NONE',  ( 6.092822981423978490, 107.5851862821014748, -14.25334919248782306 ) ) ;
#32920 = CARTESIAN_POINT ( 'NONE',  ( -12.46528703574811558, 43.00231371789854506, 2.660918448318003726 ) ) ;
#32921 = CARTESIAN_POINT ( 'NONE',  ( -60.29538769728823411, 211.8571965466040012, -6.469044688360769513 ) ) ;
#32922 = CARTESIAN_POINT ( 'NONE',  ( 16.56230152254411436, -7.209453229046475009, -4.978124999385539873 ) ) ;
#32923 = CARTESIAN_POINT ( 'NONE',  ( 7.954856959092191815, 45.77268628210144641, 5.529263428287477744 ) ) ;
#32924 = CARTESIAN_POINT ( 'NONE',  ( 24.99999999999999289, 0.000000000000000000, 49.65004534589634488 ) ) ;
#32925 = CARTESIAN_POINT ( 'NONE',  ( -35.55580436395489130, 218.5000000000000000, 0.1155267958017064944 ) ) ;
#32926 = AXIS2_PLACEMENT_3D ( 'NONE', #18508, #10144, #33448 ) ;
#32927 = CYLINDRICAL_SURFACE ( 'NONE', #167, 6.000000000000001776 ) ;
#32928 = CARTESIAN_POINT ( 'NONE',  ( -7.228626920339069173, 75.67268628210146630, 10.49813415415989581 ) ) ;
#32929 = CARTESIAN_POINT ( 'NONE',  ( 10.56230152254516952, -3.464101615138373003, -8.512500000000034817 ) ) ;
#32930 = CARTESIAN_POINT ( 'NONE',  ( 27.00000000000001421, 199.2874999999999943, 15.58845726811988897 ) ) ;
#32932 = CARTESIAN_POINT ( 'NONE',  ( 10.56230152254395094, 3.464101615137665124, -1.837500000000042100 ) ) ;
#32931 = CARTESIAN_POINT ( 'NONE',  ( -3.474262827703337830, 51.23518628210143788, -8.843639120294326972 ) ) ;
#32933 = CYLINDRICAL_SURFACE ( 'NONE', #1587, 7.500000000000000000 ) ;
#32934 = CARTESIAN_POINT ( 'NONE',  ( 23.87821517812500005, -4.985214923628404016, -9.890624999385478233 ) ) ;
#32935 = CARTESIAN_POINT ( 'NONE',  ( 34.06772145880400160, 5.407089921784862696, 163.5462758911768617 ) ) ;
#32936 = CARTESIAN_POINT ( 'NONE',  ( 24.81151116879513907, 3.464101615137757051, 162.4080514859151663 ) ) ;
#32937 = CARTESIAN_POINT ( 'NONE',  ( 21.00000000000000000, 246.9624999999999773, 6.928203230275506996 ) ) ;
#32938 = CARTESIAN_POINT ( 'NONE',  ( -27.24356964374999279, 197.1406250006145342, 15.72908226750539384 ) ) ;
#32939 = CARTESIAN_POINT ( 'NONE',  ( 8.962234695871567070, 95.03981371789856780, 8.715434833792127023 ) ) ;
#32940 = CARTESIAN_POINT ( 'NONE',  ( 8.715434833791931624, 101.2601862821014578, 8.962234695871760692 ) ) ;
#32941 = ORIENTED_EDGE ( 'NONE', *, *, #33716, .F. ) ;
#32942 = VERTEX_POINT ( 'NONE', #3341 ) ;
#32943 = CARTESIAN_POINT ( 'NONE',  ( -13.62178482187498396, 196.2781250006145228, 23.59362340125808188 ) ) ;
#32944 = CYLINDRICAL_SURFACE ( 'NONE', #2317, 5.999999999999999112 ) ;
#32945 = CARTESIAN_POINT ( 'NONE',  ( 3.257655550456945548, 77.50231371789855928, 15.46528703574811736 ) ) ;
#32946 = CARTESIAN_POINT ( 'NONE',  ( 23.87821517812500005, -4.985214923628404016, -5.953124999385495109 ) ) ;
#32947 = CARTESIAN_POINT ( 'NONE',  ( 15.24356964375000167, 245.3968750006145285, 3.323476615752272600 ) ) ;
#32948 = CARTESIAN_POINT ( 'NONE',  ( -8.710071997420127943, 96.08518628210146062, -3.796722387233380402 ) ) ;
#32949 = VECTOR ( 'NONE', #34968, 1000.000000000000000 ) ;
#32950 = PRODUCT_DEFINITION_FORMATION_WITH_SPECIFIED_SOURCE ( 'ANY', '', #11977, .NOT_KNOWN. ) ;
#32951 = CARTESIAN_POINT ( 'NONE',  ( 22.60769515458672885, 242.9888461906614054, 5.999999999999997335 ) ) ;
#32952 = CARTESIAN_POINT ( 'NONE',  ( 9.500000000000005329, 66.28981371789855359, -0.1745138560723090149 ) ) ;
#32953 = VECTOR ( 'NONE', #23845, 1000.000000000000000 ) ;
#32954 = CARTESIAN_POINT ( 'NONE',  ( 10.31873187879410736, 3.604726614523236616, -8.728124999385526550 ) ) ;
#32955 = CARTESIAN_POINT ( 'NONE',  ( -9.465287035748106703, 116.6023137178985394, 2.064181346179061460 ) ) ;
#32956 = DIRECTION ( 'NONE',  ( 0.000000000000000000, 1.000000000000000000, 0.000000000000000000 ) ) ;
#32957 = CARTESIAN_POINT ( 'NONE',  ( 7.228626920338837358, 21.72731371789854649, 10.49813415416005036 ) ) ;
#32958 = CARTESIAN_POINT ( 'NONE',  ( 15.00000000000000000, 0.000000000000000000, -3.149999999999986144 ) ) ;
#32959 =( BOUNDED_CURVE ( )  B_SPLINE_CURVE ( 2, ( #12829, #18156, #29697, #3731, #21378, #16248, #2383 ),
 .UNSPECIFIED., .F., .F. ) 
 B_SPLINE_CURVE_WITH_KNOTS ( ( 3, 2, 2, 3 ),
 ( 0.02173913043478212584, 0.02898550724637647541, 0.03623188405797082151, 0.04347826086956516761 ),
 .UNSPECIFIED. ) 
 CURVE ( )  GEOMETRIC_REPRESENTATION_ITEM ( )  RATIONAL_B_SPLINE_CURVE ( ( 1.000000000000008882, 0.8660254037844299368, 1.000000000000000000, 0.8660254037844387076, 1.000000000000000000, 0.8660254037844395958, 0.9999999999999991118 ) ) 
 REPRESENTATION_ITEM ( '' )  );
#32960 = CARTESIAN_POINT ( 'NONE',  ( 4.622313124798573369, 83.43518628210145494, 11.61527771782819940 ) ) ;
#32961 = CARTESIAN_POINT ( 'NONE',  ( 19.56230152254411081, -5.196152422706629359, -6.487499998771045995 ) ) ;
#32962 = DIRECTION ( 'NONE',  ( 0.000000000000000000, 1.000000000000000000, 0.000000000000000000 ) ) ;
#32963 = CARTESIAN_POINT ( 'NONE',  ( 30.92676673731498482, 7.209453229046475009, 163.4634630048305439 ) ) ;
#32964 = CARTESIAN_POINT ( 'NONE',  ( 16.56230152254411436, 7.209453229046482114, -3.009374999385522553 ) ) ;
#32965 = FILL_AREA_STYLE ('',( #3966 ) ) ;
#32966 = CARTESIAN_POINT ( 'NONE',  ( 10.56230152254411081, 0.000000000000000000, -2.587499998771031429 ) ) ;
#32967 = CARTESIAN_POINT ( 'NONE',  ( 28.35898146343970083, -5.196152422706638241, 168.5346827591855288 ) ) ;
#32968 = CARTESIAN_POINT ( 'NONE',  ( 5.529263428287477744, 98.67268628210146630, -7.954856959092191815 ) ) ;
#32969 = CARTESIAN_POINT ( 'NONE',  ( 3.306546357697853733E-15, 210.0000000000000284, 27.00000000000000000 ) ) ;
#32970 = CARTESIAN_POINT ( 'NONE',  ( -11.48171059495397373, 132.8851862821014720, -4.944772684328680334 ) ) ;
#32971 = DIRECTION ( 'NONE',  ( 1.000000000000000000, 0.000000000000000000, 0.000000000000000000 ) ) ;
#32972 = CARTESIAN_POINT ( 'NONE',  ( 18.12178482187499640, 239.7718750006145001, -4.985214923628404904 ) ) ;
#32973 = ORIENTED_EDGE ( 'NONE', *, *, #11274, .T. ) ;
#32974 = CARTESIAN_POINT ( 'NONE',  ( 37.41458162253433528, 3.604726614523238837, 165.9825987517649253 ) ) ;
#32975 = CARTESIAN_POINT ( 'NONE',  ( 15.24356964375000167, -3.323476615752272600, -3.253124999385455407 ) ) ;
#32976 = CARTESIAN_POINT ( 'NONE',  ( 13.62178482187501416, 199.5593750006145513, 23.59362340125806767 ) ) ;
#32977 = CARTESIAN_POINT ( 'NONE',  ( 21.91998644642377769, -5.891742046770922059, -8.000000000000003553 ) ) ;
#32978 = FACE_OUTER_BOUND ( 'NONE', #6418, .T. ) ;
#32979 = CARTESIAN_POINT ( 'NONE',  ( 25.09258843915658588, -3.464101615137914703, 165.6207793872610523 ) ) ;
#32980 = CARTESIAN_POINT ( 'NONE',  ( 15.24356964374999990, 243.9718750006145456, -3.323476615752268604 ) ) ;
#32981 = EDGE_CURVE ( 'NONE', #32041, #33635, #32522, .T. ) ;
#32982 = CARTESIAN_POINT ( 'NONE',  ( 10.31873187879411091, -3.604726614523240613, -0.5531249993855127389 ) ) ;
#32983 = CARTESIAN_POINT ( 'NONE',  ( -5.233372021372612259, 14.25231371789853618, 8.152565276336593669 ) ) ;
#32984 = CARTESIAN_POINT ( 'NONE',  ( -1.926257025242585782E-15, 196.1468750006145569, -31.45816453501076637 ) ) ;
#32986 = ORIENTED_EDGE ( 'NONE', *, *, #2222, .T. ) ;
#32985 = VERTEX_POINT ( 'NONE', #37455 ) ;
#32987 = CARTESIAN_POINT ( 'NONE',  ( 18.12178482187500350, 246.6718750006145342, 4.985214923628407568 ) ) ;
#32988 = CARTESIAN_POINT ( 'NONE',  ( -11.48171059495408208, 24.31481371789855217, 4.944772684328421875 ) ) ;
#32989 = CARTESIAN_POINT ( 'NONE',  ( 15.24356964375000167, -3.323476615752272600, -1.903124999385467753 ) ) ;
#32990 = CARTESIAN_POINT ( 'NONE',  ( -2.908627838312453306, 133.2773137178985507, 15.53471296425188797 ) ) ;
#32991 = CARTESIAN_POINT ( 'NONE',  ( 18.00000000000000000, 5.196152422706630247, -9.918749998770959309 ) ) ;
#32992 = EDGE_CURVE ( 'NONE', #529, #23005, #33534, .T. ) ;
#32993 = CARTESIAN_POINT ( 'NONE',  ( 10.56230152254500965, 3.464101615138273971, -8.024999998771040310 ) ) ;
#32994 = ORIENTED_EDGE ( 'NONE', *, *, #8210, .F. ) ;
#32995 = CARTESIAN_POINT ( 'NONE',  ( 19.68408634441911431, -5.407089921784861808, -6.346874999385549110 ) ) ;
#32996 = ORIENTED_EDGE ( 'NONE', *, *, #28836, .T. ) ;
#32997 = CARTESIAN_POINT ( 'NONE',  ( -27.24356964375000345, 197.5531250006145285, 0.000000000000000000 ) ) ;
#32998 = CARTESIAN_POINT ( 'NONE',  ( -11.48171059495397373, 132.8851862821014720, -4.944772684328680334 ) ) ;
#32999 = CARTESIAN_POINT ( 'NONE',  ( 34.02850137456756130, 5.407089921784862696, 163.0979882770355971 ) ) ;
#33000 = EDGE_CURVE ( 'NONE', #28137, #27706, #37382, .T. ) ;
#33001 = CARTESIAN_POINT ( 'NONE',  ( -50.39211230271182984, 201.5309553116392181, 2.393094931466368980 ) ) ;
#33002 = CARTESIAN_POINT ( 'NONE',  ( 15.24356964374999990, 247.0468750006145058, 0.000000000000000000 ) ) ;
#33003 = EDGE_CURVE ( 'NONE', #7808, #28808, #26996, .T. ) ;
#33004 = CARTESIAN_POINT ( 'NONE',  ( 21.00000000000000355, 0.000000000000000000, 50.00000000000001421 ) ) ;
#33005 = CARTESIAN_POINT ( 'NONE',  ( -43.66294563604516554, 213.2096571498974527, -3.378800118222469617 ) ) ;
#33006 = CARTESIAN_POINT ( 'NONE',  ( 22.56230152254410370, 7.347880794884117764E-16, -8.662499998771028942 ) ) ;
#33007 = CARTESIAN_POINT ( 'NONE',  ( 25.06647319987872535, 3.604726614523236616, 168.1169290841567090 ) ) ;
#33008 = ORIENTED_EDGE ( 'NONE', *, *, #30740, .T. ) ;
#33009 = VECTOR ( 'NONE', #14376, 1000.000000000000000 ) ;
#33010 = CYLINDRICAL_SURFACE ( 'NONE', #20372, 7.500000000000000000 ) ;
#33011 = CARTESIAN_POINT ( 'NONE',  ( -11.08355503943118592, 7.639813717898540801, -10.83675517735179383 ) ) ;
#33012 = CARTESIAN_POINT ( 'NONE',  ( -43.67038769728823411, 207.6069050685337913, 8.469044688360781947 ) ) ;
#33013 = CARTESIAN_POINT ( 'NONE',  ( 9.534712964251941258, 109.0226862821014606, -1.715153634034235708 ) ) ;
#33014 = CARTESIAN_POINT ( 'NONE',  ( 15.00000000000000000, 241.4499999999999886, 0.000000000000000000 ) ) ;
#33015 = CARTESIAN_POINT ( 'NONE',  ( -2.660918448318275509, 38.29768628210145920, 12.46528703574805874 ) ) ;
#33016 = CARTESIAN_POINT ( 'NONE',  ( 22.56230152254411792, 7.347880794884125653E-16, -7.875000000000048850 ) ) ;
#33017 = ORIENTED_EDGE ( 'NONE', *, *, #36583, .T. ) ;
#33018 =( NAMED_UNIT ( * ) SI_UNIT ( $, .STERADIAN. ) SOLID_ANGLE_UNIT ( ) );
#33019 = CARTESIAN_POINT ( 'NONE',  ( 15.53471296425195369, 118.2226862821014493, -2.908627838312120684 ) ) ;
#33020 =( BOUNDED_CURVE ( )  B_SPLINE_CURVE ( 2, ( #26337, #29369, #11939, #32218, #19606, #23697, #25274, #23508, #3408 ),
 .UNSPECIFIED., .F., .F. ) 
 B_SPLINE_CURVE_WITH_KNOTS ( ( 3, 2, 2, 2, 3 ),
 ( 0.1041666666666666713, 0.1111111111111111049, 0.1250000000000000000, 0.1388888888888888951, 0.1458333333333333426 ),
 .UNSPECIFIED. ) 
 CURVE ( )  GEOMETRIC_REPRESENTATION_ITEM ( )  RATIONAL_B_SPLINE_CURVE ( ( 0.9330127018922194093, 0.9330127018922194093, 1.000000000000000000, 0.8660254037844387076, 1.000000000000000000, 0.8660254037844387076, 1.000000000000000000, 0.9330127018922194093, 0.9330127018922194093 ) ) 
 REPRESENTATION_ITEM ( '' )  );
#33021 = CARTESIAN_POINT ( 'NONE',  ( 16.56230152254410726, -6.928203230275506996, -6.074999998771025034 ) ) ;
#33022 = CARTESIAN_POINT ( 'NONE',  ( -2.064181346179269738, 10.69768628210143646, 9.465287035748067623 ) ) ;
#33023 = CARTESIAN_POINT ( 'NONE',  ( -27.24356964374999635, 198.9406250006145171, 15.72908226750539384 ) ) ;
#33024 = CARTESIAN_POINT ( 'NONE',  ( 24.00000000000000000, -5.196152422706629359, -2.099999999999990763 ) ) ;
#33025 = CARTESIAN_POINT ( 'NONE',  ( -1.909035429704832693E-15, 195.3874999999999886, -31.17691453623979214 ) ) ;
#33026 = CARTESIAN_POINT ( 'NONE',  ( 13.56230152254410548, 5.196152422706630247, -1.312499998771005094 ) ) ;
#33027 = CARTESIAN_POINT ( 'NONE',  ( 31.43172532185920076, 7.209453229046482114, 169.2351660368995852 ) ) ;
#33028 = CARTESIAN_POINT ( 'NONE',  ( 2.999999999999997335, 244.5000000000000000, 1.000000000000000000 ) ) ;
#33029 = CARTESIAN_POINT ( 'NONE',  ( -6.840914352311947333, 81.23981371789855643, -6.594114490232462877 ) ) ;
#33030 = ORIENTED_EDGE ( 'NONE', *, *, #30732, .F. ) ;
#33031 = AXIS2_PLACEMENT_3D ( 'NONE', #14707, #23245, #14154 ) ;
#33032 = CARTESIAN_POINT ( 'NONE',  ( 15.00000000000000000, 242.8187500012290627, -3.464101615137752166 ) ) ;
#33033 = CARTESIAN_POINT ( 'NONE',  ( -10.69584247140429412, 71.75231371789855928, -6.932735513424201024 ) ) ;
#33034 = ADVANCED_FACE ( 'NONE', ( #10344 ), #30879, .T. ) ;
#33035 = CARTESIAN_POINT ( 'NONE',  ( 10.31873187879410736, -3.604726614523244610, -3.309374999385498395 ) ) ;
#33036 = DIRECTION ( 'NONE',  ( 0.08715574274765150453, 0.000000000000000000, 0.9961946980917461003 ) ) ;
#33037 = CARTESIAN_POINT ( 'NONE',  ( 18.12178482187500350, -4.985214923628407568, -5.128124999385475391 ) ) ;
#33038 = CARTESIAN_POINT ( 'NONE',  ( -12.53471296425189152, 52.77731371789855075, -2.311890736173453753 ) ) ;
#33039 = AXIS2_PLACEMENT_3D ( 'NONE', #23708, #9859, #12702 ) ;
#33040 = EDGE_CURVE ( 'NONE', #4722, #32744, #17712, .T. ) ;
#33041 = ORIENTED_EDGE ( 'NONE', *, *, #23582, .T. ) ;
#33042 = CYLINDRICAL_SURFACE ( 'NONE', #1980, 27.00000000000000000 ) ;
#33043 = CARTESIAN_POINT ( 'NONE',  ( 23.87821517812500005, 244.9468750006145115, 4.985214923628404016 ) ) ;
#33044 = CARTESIAN_POINT ( 'NONE',  ( -2.311890736173176641, 14.72268628210143859, -12.53471296425194836 ) ) ;
#33045 = EDGE_CURVE ( 'NONE', #21562, #30233, #28885, .T. ) ;
#33046 = CARTESIAN_POINT ( 'NONE',  ( -42.87127896937850124, 216.5309553116392181, 1.626142955000506429 ) ) ;
#33047 = CARTESIAN_POINT ( 'NONE',  ( -52.76711230271183695, 216.4690446883607535, -1.857196546604089393 ) ) ;
#33048 = ADVANCED_FACE ( 'NONE', ( #3482 ), #11459, .T. ) ;
#33049 = CARTESIAN_POINT ( 'NONE',  ( 0.000000000000000000, 200.0000000000000000, 0.000000000000000000 ) ) ;
#33050 = CARTESIAN_POINT ( 'NONE',  ( -8.715434833792127023, 78.93981371789855928, 8.962234695871568846 ) ) ;
#33051 = CARTESIAN_POINT ( 'NONE',  ( -44.46205436395490551, 213.2096571498974242, 3.378800118222489601 ) ) ;
#33052 = CARTESIAN_POINT ( 'NONE',  ( -63.06622103062156981, 211.6261429550005744, 6.530955311639227823 ) ) ;
#33053 = CARTESIAN_POINT ( 'NONE',  ( 20.99999999999999645, 6.646953231504538984, -6.215624999385504168 ) ) ;
#33054 = CARTESIAN_POINT ( 'NONE',  ( 21.00000000000000355, 0.000000000000000000, 50.00000000000001421 ) ) ;
#33055 = CARTESIAN_POINT ( 'NONE',  ( -11.08355503943118592, 53.63981371789855501, -10.83675517735179383 ) ) ;
#33056 = CARTESIAN_POINT ( 'NONE',  ( -41.28794563604517265, 203.8621396198271043, 6.307003348498029460 ) ) ;
#33058 = MANIFOLD_SOLID_BREP ( 'Boss-Extrude3', #1710 ) ;
#33057 = LINE ( 'NONE', #19234, #36503 ) ;
#33059 = CARTESIAN_POINT ( 'NONE',  ( 12.46528703574805874, 81.99768628210146915, 2.660918448318279950 ) ) ;
#33060 = CARTESIAN_POINT ( 'NONE',  ( -0.1745138560725817967, 19.61018628210144144, 15.50000000000000533 ) ) ;
#33061 = AXIS2_PLACEMENT_3D ( 'NONE', #9998, #24778, #4680 ) ;
#33062 = CARTESIAN_POINT ( 'NONE',  ( 16.56230152254411436, 6.928203230275514990, -0.1125000000000229705 ) ) ;
#33063 = DIRECTION ( 'NONE',  ( 0.9961946980917462113, 0.000000000000000000, -0.08715574274765118534 ) ) ;
#33064 = VERTEX_POINT ( 'NONE', #1716 ) ;
#33065 = CARTESIAN_POINT ( 'NONE',  ( -14.25334919248782306, 40.88518628210145067, -6.092822981423979378 ) ) ;
#33066 = CARTESIAN_POINT ( 'NONE',  ( -13.62178482187498396, 197.1781250006145569, 23.59362340125808188 ) ) ;
#33067 = CYLINDRICAL_SURFACE ( 'NONE', #11397, 4.899999999999999467 ) ;
#33068 =( BOUNDED_CURVE ( )  B_SPLINE_CURVE ( 2, ( #36918, #27659, #1684, #10410, #5089, #28214, #13259, #4715, #36550 ),
 .UNSPECIFIED., .F., .F. ) 
 B_SPLINE_CURVE_WITH_KNOTS ( ( 3, 2, 2, 2, 3 ),
 ( 0.7291666666666667407, 0.7361111111111111605, 0.7500000000000000000, 0.7638888888888888395, 0.7708333333333333703 ),
 .UNSPECIFIED. ) 
 CURVE ( )  GEOMETRIC_REPRESENTATION_ITEM ( )  RATIONAL_B_SPLINE_CURVE ( ( 0.9330127018922192983, 0.9330127018922198534, 1.000000000000000000, 0.8660254037844387076, 1.000000000000000000, 0.8660254037844387076, 1.000000000000000000, 0.9330127018922187432, 0.9330127018922192983 ) ) 
 REPRESENTATION_ITEM ( '' )  );
#33069 = DIRECTION ( 'NONE',  ( 1.000000000000000000, 0.000000000000000000, 0.000000000000000000 ) ) ;
#33070 = CARTESIAN_POINT ( 'NONE',  ( -36.94122103062157692, 208.3738570449993404, -6.530955311639226935 ) ) ;
#33071 = FACE_OUTER_BOUND ( 'NONE', #31178, .T. ) ;
#33072 = CARTESIAN_POINT ( 'NONE',  ( -4.944772684328673229, 29.38518628210144712, 11.48171059495397728 ) ) ;
#33073 = CARTESIAN_POINT ( 'NONE',  ( 26.75643035624999655, 249.1468750006145285, 3.323476615752267715 ) ) ;
#33074 = CARTESIAN_POINT ( 'NONE',  ( 2.064181346179061460, 132.7023137178985337, 9.465287035748106703 ) ) ;
#33075 = CARTESIAN_POINT ( 'NONE',  ( 26.75643035624999655, 244.1968750006145683, 3.323476615752267271 ) ) ;
#33076 = ORIENTED_EDGE ( 'NONE', *, *, #25380, .T. ) ;
#33077 = FACE_BOUND ( 'NONE', #20552, .T. ) ;
#33078 = EDGE_CURVE ( 'NONE', #1071, #14163, #17219, .T. ) ;
#33079 = CARTESIAN_POINT ( 'NONE',  ( 2.311890736173452421, 137.8773137178985735, -12.53471296425189152 ) ) ;
#33080 = CARTESIAN_POINT ( 'NONE',  ( 16.56230152254411081, -7.209453229046475009, -6.328124999385527083 ) ) ;
#33081 = CARTESIAN_POINT ( 'NONE',  ( 27.93778984224218931, 5.407089921784856479, 165.1177646232817153 ) ) ;
#33082 = CYLINDRICAL_SURFACE ( 'NONE', #9903, 4.000000000000003553 ) ;
#33083 = CARTESIAN_POINT ( 'NONE',  ( -26.99999999999998934, 198.2374999999999829, 15.58845726811991561 ) ) ;
#33084 = ORIENTED_EDGE ( 'NONE', *, *, #8768, .F. ) ;
#33085 = CARTESIAN_POINT ( 'NONE',  ( -2.311890736173176641, 51.52268628210145351, -12.53471296425194659 ) ) ;
#33086 = ORIENTED_EDGE ( 'NONE', *, *, #36247, .T. ) ;
#33087 = VERTEX_POINT ( 'NONE', #21826 ) ;
#33088 = CARTESIAN_POINT ( 'NONE',  ( -7.234628195640263826, 195.8575961894323711, -27.00000000000003553 ) ) ;
#33089 = CARTESIAN_POINT ( 'NONE',  ( 15.24356964374999990, 0.000000000000000000, -1.490624999385459226 ) ) ;
#33090 = LINE ( 'NONE', #18707, #17815 ) ;
#33091 = CARTESIAN_POINT ( 'NONE',  ( 21.00000000000000000, -6.646953231504538984, -8.128124999385477167 ) ) ;
#33092 = CARTESIAN_POINT ( 'NONE',  ( 8.962234695871762469, 71.36018628210145209, -8.715434833791931624 ) ) ;
#33093 = CARTESIAN_POINT ( 'NONE',  ( -0.1745138560725817967, 139.2101862821014890, 15.50000000000000533 ) ) ;
#33094 = CARTESIAN_POINT ( 'NONE',  ( 22.56230152254337185, -3.464101615138180268, -3.749999998771029297 ) ) ;
#33095 = CARTESIAN_POINT ( 'NONE',  ( 22.56230152254410370, 7.347880794884117764E-16, -5.062499998771007981 ) ) ;
#33096 =( BOUNDED_CURVE ( )  B_SPLINE_CURVE ( 2, ( #4461, #2172, #33459, #35922, #30808, #4644, #24926 ),
 .UNSPECIFIED., .F., .F. ) 
 B_SPLINE_CURVE_WITH_KNOTS ( ( 3, 2, 2, 3 ),
 ( 0.4347826086956526059, 0.4420289855072469520, 0.4492753623188412426, 0.4565217391304355332 ),
 .UNSPECIFIED. ) 
 CURVE ( )  GEOMETRIC_REPRESENTATION_ITEM ( )  RATIONAL_B_SPLINE_CURVE ( ( 0.9999999999999917843, 0.8660254037844469233, 1.000000000000000000, 0.8660254037844387076, 1.000000000000000000, 0.8660254037844243857, 1.000000000000014433 ) ) 
 REPRESENTATION_ITEM ( '' )  );
#33097 = CARTESIAN_POINT ( 'NONE',  ( -49.00669563604517265, 209.8844732041982297, -4.499999999999996447 ) ) ;
#33098 = DIRECTION ( 'NONE',  ( -0.000000000000000000, -1.000000000000000000, -0.000000000000000000 ) ) ;
#33099 = CARTESIAN_POINT ( 'NONE',  ( 28.25112623189659544, -5.196152422706632912, 167.3018918215213660 ) ) ;
#33100 = CARTESIAN_POINT ( 'NONE',  ( -8.715434833792127023, 134.1398137178985621, 8.962234695871568846 ) ) ;
#33101 = CARTESIAN_POINT ( 'NONE',  ( -50.79538769728821990, 211.8571965466039444, -6.469044688360768625 ) ) ;
#33102 = CARTESIAN_POINT ( 'NONE',  ( -53.96205436395491262, 216.1378603801730094, 6.307003348497944195 ) ) ;
#33103 = CARTESIAN_POINT ( 'NONE',  ( 26.75643035624999655, 7.049594010296217766E-16, -0.4781249993854874702 ) ) ;
#33104 = CARTESIAN_POINT ( 'NONE',  ( -27.24356964374999635, 197.5906250006145228, 15.72908226750539384 ) ) ;
#33105 = CARTESIAN_POINT ( 'NONE',  ( 8.927990412390371944, 113.7273137178985678, 13.04141134922778811 ) ) ;
#33106 = CARTESIAN_POINT ( 'NONE',  ( -50.19419563604517265, 203.5000000000000000, 0.1155267958017914542 ) ) ;
#33107 = EDGE_LOOP ( 'NONE', ( #30106, #1363, #19715, #30359 ) ) ;
#33108 = CARTESIAN_POINT ( 'NONE',  ( 12.53471296425194836, 26.22268628210144925, -2.311890736173178418 ) ) ;
#33109 = CARTESIAN_POINT ( 'NONE',  ( 26.97716818855048260, 0.000000000000000000, 49.47706554351410801 ) ) ;
#33110 = CARTESIAN_POINT ( 'NONE',  ( 3.306546357697853733E-15, 210.0000000000000284, 27.00000000000000000 ) ) ;
#33111 = CARTESIAN_POINT ( 'NONE',  ( 24.90795869275643426, 0.000000000000000000, 166.3050999770023850 ) ) ;
#33112 = CARTESIAN_POINT ( 'NONE',  ( 2.908627838312118019, 102.1226862821014549, 15.53471296425195369 ) ) ;
#33113 = CARTESIAN_POINT ( 'NONE',  ( -58.90997103062156270, 215.5714017266979852, 3.350049139982118618 ) ) ;
#33114 = CARTESIAN_POINT ( 'NONE',  ( 13.44051670066911264, 5.407089921784856479, -3.815624999385564209 ) ) ;
#33115 = CARTESIAN_POINT ( 'NONE',  ( 9.534712964251941258, 35.42268628210144499, -1.715153634034235708 ) ) ;
#33116 = EDGE_CURVE ( 'NONE', #14550, #33325, #35349, .T. ) ;
#33117 = DIRECTION ( 'NONE',  ( 0.000000000000000000, 1.000000000000000000, -3.273063162220408568E-16 ) ) ;
#33118 = CARTESIAN_POINT ( 'NONE',  ( -35.75372103062156981, 218.5309553116391896, -2.162041339862839084 ) ) ;
#33119 = FACE_OUTER_BOUND ( 'NONE', #22374, .T. ) ;
#33120 = CARTESIAN_POINT ( 'NONE',  ( 11.48171059495397728, 82.28518628210146346, 4.944772684328674117 ) ) ;
#33121 = DIRECTION ( 'NONE',  ( 0.000000000000000000, 0.000000000000000000, 1.000000000000000000 ) ) ;
#33122 = CARTESIAN_POINT ( 'NONE',  ( 13.56230152254411436, -5.196152422706632912, -7.912499998771055587 ) ) ;
#33124 = CARTESIAN_POINT ( 'NONE',  ( 26.99999999999999645, 7.347880794884117764E-16, -5.624999999999991118 ) ) ;
#33123 = CARTESIAN_POINT ( 'NONE',  ( 5.529263428287477744, 43.47268628210144215, -7.954856959092191815 ) ) ;
#33125 = DIRECTION ( 'NONE',  ( 1.000000000000000000, 0.000000000000000000, 0.000000000000000000 ) ) ;
#33127 = ADVANCED_FACE ( 'NONE', ( #36769 ), #19178, .F. ) ;
#33126 = ORIENTED_EDGE ( 'NONE', *, *, #10754, .T. ) ;
#33128 = CARTESIAN_POINT ( 'NONE',  ( 15.24356964375000167, -3.323476615752272600, -9.103124999385496352 ) ) ;
#33129 = DIRECTION ( 'NONE',  ( -0.000000000000000000, 1.000000000000000000, -0.000000000000000000 ) ) ;
#33130 = CARTESIAN_POINT ( 'NONE',  ( 27.69756682629397915, 5.407089921784862696, 162.3720029866663594 ) ) ;
#33131 = CARTESIAN_POINT ( 'NONE',  ( 30.72331255028488428, -6.928203230275514990, 161.1379710058604644 ) ) ;
#33132 = CARTESIAN_POINT ( 'NONE',  ( 21.00000000000000000, 245.6124999999999829, 6.928203230275506996 ) ) ;
#33133 = CARTESIAN_POINT ( 'NONE',  ( 19.56230152254410370, 5.196152422706631135, -4.087499998771032317 ) ) ;
#33134 = EDGE_CURVE ( 'NONE', #28841, #18251, #4929, .T. ) ;
#33135 = CARTESIAN_POINT ( 'NONE',  ( -2.311890736173448424, 78.07731371789856212, 12.53471296425189330 ) ) ;
#33136 = CARTESIAN_POINT ( 'NONE',  ( 6.932735513423970097, 101.5476862821014521, 10.69584247140445044 ) ) ;
#33137 = ORIENTED_EDGE ( 'NONE', *, *, #33000, .F. ) ;
#33138 = ORIENTED_EDGE ( 'NONE', *, *, #27314, .T. ) ;
#33139 = PRODUCT_DEFINITION ( 'UNKNOWN', '', #25670, #5807 ) ;
#33140 = CARTESIAN_POINT ( 'NONE',  ( 13.50000000000001421, 198.9125000012290343, 23.38268590217984055 ) ) ;
#33141 = DIRECTION ( 'NONE',  ( 0.000000000000000000, 0.000000000000000000, -1.000000000000000000 ) ) ;
#33142 = AXIS2_PLACEMENT_3D ( 'NONE', #2512, #11232, #22804 ) ;
#33143 = CARTESIAN_POINT ( 'NONE',  ( 13.23911966647199812, 76.35231371789853938, 8.632099005475788900 ) ) ;
#33144 = CARTESIAN_POINT ( 'NONE',  ( 15.24356964375000167, -3.323476615752272600, -5.615624999385488536 ) ) ;
#33145 = CARTESIAN_POINT ( 'NONE',  ( 21.00000000000000000, 244.5718750006145115, 6.646953231504538984 ) ) ;
#33146 = CARTESIAN_POINT ( 'NONE',  ( -51.98288769728823411, 205.5309553116392465, -1.321298161741839117 ) ) ;
#33147 = CARTESIAN_POINT ( 'NONE',  ( 15.00000000000000178, -3.464101615137757051, -6.656249998770961795 ) ) ;
#33148 = CARTESIAN_POINT ( 'NONE',  ( 5.529263428287300108, 49.32731371789854791, 7.954856959092309943 ) ) ;
#33149 = CARTESIAN_POINT ( 'NONE',  ( 22.80587116629411426, -3.604726614523235284, -8.053124999385516958 ) ) ;
#33150 = CARTESIAN_POINT ( 'NONE',  ( -8.843639120294245259, 108.2648137178985621, -3.474262827703533230 ) ) ;
#33151 = FACE_OUTER_BOUND ( 'NONE', #13419, .T. ) ;
#33152 = CARTESIAN_POINT ( 'NONE',  ( -12.50000000000000355, 34.08981371789854364, 0.1745138560722786503 ) ) ;
#33153 = CARTESIAN_POINT ( 'NONE',  ( 7.228626920339068285, 80.27268628210146062, -10.49813415415989581 ) ) ;
#33154 = CARTESIAN_POINT ( 'NONE',  ( 16.56230152254411081, 6.928203230275506996, -8.549999998770985599 ) ) ;
#33155 = CARTESIAN_POINT ( 'NONE',  ( -1.045839947578415010E-13, 196.0625000000000284, 27.00000000000000355 ) ) ;
#33156 = CARTESIAN_POINT ( 'NONE',  ( 37.17272443640959523, -3.604726614523235284, 163.2181584645603323 ) ) ;
#33157 = CARTESIAN_POINT ( 'NONE',  ( 13.44051670066911441, -5.407089921784865361, -4.621874999385545024 ) ) ;
#33158 = CARTESIAN_POINT ( 'NONE',  ( 15.00000000000000000, 0.000000000000000000, -0.9000000000000119016 ) ) ;
#33159 = CARTESIAN_POINT ( 'NONE',  ( 14.99999999999952394, -3.464101615137481716, -4.912499999999994316 ) ) ;
#33160 = CARTESIAN_POINT ( 'NONE',  ( -27.00000000000000355, 199.6250000012290400, -15.58845726811989429 ) ) ;
#33161 = CARTESIAN_POINT ( 'NONE',  ( -2.064181346179269738, 102.6976862821014294, 9.465287035748067623 ) ) ;
#33162 = CYLINDRICAL_SURFACE ( 'NONE', #25547, 5.999999999999998224 ) ;
#33163 = CARTESIAN_POINT ( 'NONE',  ( 4.622313124798573369, 138.6351862821014720, 11.61527771782819940 ) ) ;
#33164 = CARTESIAN_POINT ( 'NONE',  ( -11.00000000000001243, 143.0000000000000000, -1.227709706637561792E-13 ) ) ;
#33165 = CARTESIAN_POINT ( 'NONE',  ( 23.87821517812500005, 240.4468750006145115, 4.985214923628404016 ) ) ;
#33166 = ORIENTED_EDGE ( 'NONE', *, *, #14594, .T. ) ;
#33167 = CARTESIAN_POINT ( 'NONE',  ( 27.83320295094501162, -5.407089921784859143, 163.9223309855715911 ) ) ;
#33168 = CIRCLE ( 'NONE', #34962, 25.00000000000000000 ) ;
#33169 = CARTESIAN_POINT ( 'NONE',  ( 23.87821517812499650, 4.985214923628404904, -2.990624999385460558 ) ) ;
#33170 = DIRECTION ( 'NONE',  ( 0.000000000000000000, 0.000000000000000000, 1.000000000000000000 ) ) ;
#33171 = CARTESIAN_POINT ( 'NONE',  ( 28.17268606342371129, -5.196152422706632912, 166.4053165932387515 ) ) ;
#33172 = CARTESIAN_POINT ( 'NONE',  ( 34.43419986258128773, 5.196152422706637353, 169.1324673380528623 ) ) ;
#33173 = CARTESIAN_POINT ( 'NONE',  ( -47.00000000000000711, 244.5000000000000000, -2.499999999999997780 ) ) ;
#33174 = CARTESIAN_POINT ( 'NONE',  ( 15.24356964375000167, 241.7968750006145342, 3.323476615752272600 ) ) ;
#33175 = CARTESIAN_POINT ( 'NONE',  ( 13.44051670066911086, 5.407089921784856479, -2.015624999385540406 ) ) ;
#33176 = CARTESIAN_POINT ( 'NONE',  ( -0.1745138560723084320, 27.18981371789855572, -9.500000000000005329 ) ) ;
#33177 = CARTESIAN_POINT ( 'NONE',  ( -27.24356964375000345, 196.7093750006145569, 0.000000000000000000 ) ) ;
#33179 = ORIENTED_EDGE ( 'NONE', *, *, #1371, .T. ) ;
#33178 = ORIENTED_EDGE ( 'NONE', *, *, #19803, .T. ) ;
#33180 = CARTESIAN_POINT ( 'NONE',  ( 21.00000000000000000, 248.0593750006145228, 6.646953231504538984 ) ) ;
#33181 = CARTESIAN_POINT ( 'NONE',  ( -6.932735513424201912, 23.45231371789854791, 10.69584247140429412 ) ) ;
#33182 = CARTESIAN_POINT ( 'NONE',  ( 15.24356964374999990, 3.323476615752268604, -1.078124999385470462 ) ) ;
#33183 = CARTESIAN_POINT ( 'NONE',  ( -0.1745138560722442889, 137.5898137178985792, -15.50000000000000533 ) ) ;
#33184 = CARTESIAN_POINT ( 'NONE',  ( 15.00000000000000178, -3.464101615137757051, -8.906249998770972454 ) ) ;
#33185 = EDGE_CURVE ( 'NONE', #36053, #21699, #2315, .T. ) ;
#33186 = VERTEX_POINT ( 'NONE', #37460 ) ;
#33187 = CARTESIAN_POINT ( 'NONE',  ( 13.44051670066911441, -5.407089921784865361, -5.071874999385522997 ) ) ;
#33188 = ORIENTED_EDGE ( 'NONE', *, *, #18627, .F. ) ;
#33189 = CARTESIAN_POINT ( 'NONE',  ( -1.926257025242585782E-15, 196.0906250006145228, -31.45816453501075927 ) ) ;
#33190 = CARTESIAN_POINT ( 'NONE',  ( 12.46528703574805874, 137.1976862821014720, 2.660918448318279950 ) ) ;
#33191 = CARTESIAN_POINT ( 'NONE',  ( 27.89366724747619131, 5.407089921784862696, 164.6134410573727678 ) ) ;
#33192 = CARTESIAN_POINT ( 'NONE',  ( -58.30877896937849414, 212.1620413398627534, -8.530955311639255356 ) ) ;
#33193 = AXIS2_PLACEMENT_3D ( 'NONE', #10946, #36342, #24608 ) ;
#33194 = CARTESIAN_POINT ( 'NONE',  ( 20.99999999999999645, 246.2593750006145115, 6.646953231504538984 ) ) ;
#33195 =( NAMED_UNIT ( * ) SI_UNIT ( $, .STERADIAN. ) SOLID_ANGLE_UNIT ( ) );
#33196 = CARTESIAN_POINT ( 'NONE',  ( 26.99999999999999645, 196.6625000000000512, -15.58845726811990495 ) ) ;
#33197 = CARTESIAN_POINT ( 'NONE',  ( -51.57961230271184405, 211.3212981617417938, 4.469044688360757966 ) ) ;
#33199 = EDGE_CURVE ( 'NONE', #10880, #2775, #22719, .T. ) ;
#33198 = CARTESIAN_POINT ( 'NONE',  ( 20.99999999999999289, 245.8374999999999773, -5.999999999999997335 ) ) ;
#33200 = CARTESIAN_POINT ( 'NONE',  ( 10.56230152254411614, -3.464101615137757051, -0.7499999987710380678 ) ) ;
#33201 = ORIENTED_EDGE ( 'NONE', *, *, #30770, .T. ) ;
#33202 = CARTESIAN_POINT ( 'NONE',  ( 1.120210788295102201E-13, 195.5000000012290400, -27.00000000000000711 ) ) ;
#33203 = CARTESIAN_POINT ( 'NONE',  ( -2.908627838312119351, 125.1226862821014691, -15.53471296425195369 ) ) ;
#33204 = CARTESIAN_POINT ( 'NONE',  ( -51.19122103062157692, 207.8379586601371329, -8.530955311639223382 ) ) ;
#33205 = CARTESIAN_POINT ( 'NONE',  ( -9.500000000000005329, 113.9101862821014493, -0.1745138560725176813 ) ) ;
#33206 = CARTESIAN_POINT ( 'NONE',  ( 18.00000000000000355, 241.5249999999999773, 5.196152422706632912 ) ) ;
#33207 = CARTESIAN_POINT ( 'NONE',  ( 12.46528703574805874, 8.397686282101442856, 2.660918448318279950 ) ) ;
#33208 = CARTESIAN_POINT ( 'NONE',  ( 10.56230152254410726, 0.000000000000000000, -8.100000000000024514 ) ) ;
#33209 = VERTEX_POINT ( 'NONE', #20238 ) ;
#33210 = SURFACE_STYLE_FILL_AREA ( #27147 ) ;
#33211 = CARTESIAN_POINT ( 'NONE',  ( -5.529263428287477744, 75.67268628210143788, 7.954856959092191815 ) ) ;
#33212 = DIRECTION ( 'NONE',  ( 0.9961946980917462113, 0.000000000000000000, -0.08715574274765118534 ) ) ;
#33213 = CARTESIAN_POINT ( 'NONE',  ( -3.796722387233375073, 10.98518628210143433, 8.710071997420127943 ) ) ;
#33214 = CARTESIAN_POINT ( 'NONE',  ( -27.24356964374999635, 198.0406250006145399, 15.72908226750539384 ) ) ;
#33215 = CARTESIAN_POINT ( 'NONE',  ( 27.00000000000003908, -3.464101615137728185, -2.062499999999993339 ) ) ;
#33216 = CARTESIAN_POINT ( 'NONE',  ( -27.24356964374999990, 197.5718750006145399, -15.72908226750537786 ) ) ;
#33217 = CARTESIAN_POINT ( 'NONE',  ( 19.17052166273705538, -5.587842338165578404, -10.00000000000000355 ) ) ;
#33218 = EDGE_CURVE ( 'NONE', #4551, #11581, #34737, .T. ) ;
#33219 = PLANE ( 'NONE',  #36917 ) ;
#33220 = CARTESIAN_POINT ( 'NONE',  ( -8.843639120294245259, 80.66481371789856780, -3.474262827703533230 ) ) ;
#33221 = EDGE_LOOP ( 'NONE', ( #5928, #15960, #6918, #3464, #2036, #12953 ) ) ;
#33222 = CARTESIAN_POINT ( 'NONE',  ( 26.99999999999999645, 244.4687500012290684, -3.464101615137755275 ) ) ;
#33223 = CARTESIAN_POINT ( 'NONE',  ( -12.53471296425189152, 80.37731371789854506, -2.311890736173453309 ) ) ;
#33224 = CARTESIAN_POINT ( 'NONE',  ( 13.44051670066911086, 5.407089921784862696, -2.971874999385532234 ) ) ;
#33225 = CARTESIAN_POINT ( 'NONE',  ( 15.00000000000000178, 242.8375000000000057, 3.464101615137757051 ) ) ;
#33226 = CARTESIAN_POINT ( 'NONE',  ( 18.12178482187500350, -4.985214923628407568, -4.228124999385491023 ) ) ;
#33227 = CARTESIAN_POINT ( 'NONE',  ( -0.1745138560722763466, 45.58981371789855075, -12.50000000000000355 ) ) ;
#33228 = ADVANCED_FACE ( 'NONE', ( #34262 ), #1096, .T. ) ;
#33229 = VERTEX_POINT ( 'NONE', #35712 ) ;
#33230 = CARTESIAN_POINT ( 'NONE',  ( 15.24356964374999990, 3.323476615752268604, -7.378124999385474503 ) ) ;
#33231 = CARTESIAN_POINT ( 'NONE',  ( 21.00000000000000000, 245.1343750006145115, -6.646953231504538984 ) ) ;
#33232 = CARTESIAN_POINT ( 'NONE',  ( -10.49813415415989581, 22.77268628210143575, -7.228626920339068285 ) ) ;
#33233 = CARTESIAN_POINT ( 'NONE',  ( -41.68377896937850124, 208.3738570449995109, 6.530955311639247363 ) ) ;
#33234 = CARTESIAN_POINT ( 'NONE',  ( -52.56919563604516554, 216.5000000000000000, -0.1155267958017906493 ) ) ;
#33235 =( NAMED_UNIT ( * ) PLANE_ANGLE_UNIT ( ) SI_UNIT ( $, .RADIAN. ) );
#33236 = CARTESIAN_POINT ( 'NONE',  ( 30.61545731874177534, -6.928203230275506996, 159.9051800681962732 ) ) ;
#33237 = CARTESIAN_POINT ( 'NONE',  ( 4.944772684328420986, 68.01481371789854791, 11.48171059495408208 ) ) ;
#33238 = CARTESIAN_POINT ( 'NONE',  ( -51.78497103062156981, 206.1606490808709111, -2.350049139982163027 ) ) ;
#33239 = CARTESIAN_POINT ( 'NONE',  ( -60.49330436395489841, 210.1155267958017134, -6.500000000000000888 ) ) ;
#33240 = CARTESIAN_POINT ( 'NONE',  ( 16.56230152254410726, 0.000000000000000000, -10.00000000000000000 ) ) ;
#33241 = CARTESIAN_POINT ( 'NONE',  ( -8.927990412390371944, 53.92731371789854222, -13.04141134922778988 ) ) ;
#33242 = CARTESIAN_POINT ( 'NONE',  ( -44.05877896937850124, 212.1620413398627534, -8.530955311639255356 ) ) ;
#33243 =( BOUNDED_CURVE ( )  B_SPLINE_CURVE ( 2, ( #11751, #23319, #5872, #7843, #31471, #26152, #22954 ),
 .UNSPECIFIED., .F., .F. ) 
 B_SPLINE_CURVE_WITH_KNOTS ( ( 3, 2, 2, 3 ),
 ( 0.5652173913043470055, 0.5724637681159410185, 0.5797101449275351426, 0.5869565217391291556 ),
 .UNSPECIFIED. ) 
 CURVE ( )  GEOMETRIC_REPRESENTATION_ITEM ( )  RATIONAL_B_SPLINE_CURVE ( ( 1.000000000000014433, 0.8660254037844243857, 1.000000000000000000, 0.8660254037844387076, 1.000000000000000000, 0.8660254037844633546, 0.9999999999999753530 ) ) 
 REPRESENTATION_ITEM ( '' )  );
#33244 = DIRECTION ( 'NONE',  ( 0.000000000000000000, 1.000000000000000000, 0.000000000000000000 ) ) ;
#33245 = CARTESIAN_POINT ( 'NONE',  ( 4.622313124798573369, 65.03518628210144925, 11.61527771782819940 ) ) ;
#33246 = CARTESIAN_POINT ( 'NONE',  ( -8.632099005475501130, 32.54768628210143788, -13.23911966647218996 ) ) ;
#33247 = FACE_OUTER_BOUND ( 'NONE', #2450, .T. ) ;
#33248 = CARTESIAN_POINT ( 'NONE',  ( -27.00000000000000355, 197.3750000012290400, -15.58845726811989429 ) ) ;
#33249 = ORIENTED_EDGE ( 'NONE', *, *, #8678, .F. ) ;
#33250 = CARTESIAN_POINT ( 'NONE',  ( 10.83675517735155225, 36.86018628210144499, 11.08355503943142573 ) ) ;
#33251 = CARTESIAN_POINT ( 'NONE',  ( 13.62178482187499640, 198.7531250006145456, -23.59362340125807123 ) ) ;
#33252 = EDGE_CURVE ( 'NONE', #33506, #25295, #27190, .T. ) ;
#33253 = DIRECTION ( 'NONE',  ( -0.000000000000000000, -1.000000000000000000, -0.000000000000000000 ) ) ;
#33254 = CARTESIAN_POINT ( 'NONE',  ( -26.99999999999999645, 199.1375000000000171, 15.58845726811991561 ) ) ;
#33255 = CARTESIAN_POINT ( 'NONE',  ( -36.14955436395490551, 214.8429017333601792, -4.673758765035196383 ) ) ;
#33256 = DIRECTION ( 'NONE',  ( -1.000000000000000000, 0.000000000000000000, 0.000000000000000000 ) ) ;
#33257 = CARTESIAN_POINT ( 'NONE',  ( 12.46528703574805874, 17.59768628210143859, 2.660918448318279950 ) ) ;
#33258 = CARTESIAN_POINT ( 'NONE',  ( 20.99999999999999645, 185.0294372515228645, -5.999999999999999112 ) ) ;
#33259 = CARTESIAN_POINT ( 'NONE',  ( -8.843639120294245259, 126.6648137178985820, -3.474262827703533230 ) ) ;
#33260 = CARTESIAN_POINT ( 'NONE',  ( 20.99999999999999645, 243.8968750006145285, -6.646953231504538984 ) ) ;
#33261 = ORIENTED_EDGE ( 'NONE', *, *, #6855, .T. ) ;
#33262 = CARTESIAN_POINT ( 'NONE',  ( 18.00000000000000000, 249.5312500012290684, -5.196152422706630247 ) ) ;
#33263 = EDGE_CURVE ( 'NONE', #13931, #26175, #4966, .T. ) ;
#33264 = CARTESIAN_POINT ( 'NONE',  ( 18.00000000000000355, -5.196152422706632912, -7.068749998770940124 ) ) ;
#33265 = DIRECTION ( 'NONE',  ( -0.000000000000000000, 0.000000000000000000, -1.000000000000000000 ) ) ;
#33266 = CARTESIAN_POINT ( 'NONE',  ( 22.80587116629410716, -3.604726614523235284, -6.703124999385561722 ) ) ;
#33267 = CARTESIAN_POINT ( 'NONE',  ( 34.03340388509710834, 5.407089921784857367, 163.1540242288032232 ) ) ;
#33268 = DIRECTION ( 'NONE',  ( 0.000000000000000000, 0.000000000000000000, 1.000000000000000000 ) ) ;
#33269 = CARTESIAN_POINT ( 'NONE',  ( -27.00000000000000355, 197.3000000000000114, 0.000000000000000000 ) ) ;
#33270 = EDGE_LOOP ( 'NONE', ( #3264, #15659, #4371, #31678 ) ) ;
#33271 = CARTESIAN_POINT ( 'NONE',  ( 7.228626920339069173, 25.07268628210145067, -10.49813415415989404 ) ) ;
#33272 = ORIENTED_EDGE ( 'NONE', *, *, #27886, .T. ) ;
#33273 = ORIENTED_EDGE ( 'NONE', *, *, #19562, .T. ) ;
#33274 = CARTESIAN_POINT ( 'NONE',  ( 20.99999999999999645, 250.0000000000000000, 0.000000000000000000 ) ) ;
#33275 = CARTESIAN_POINT ( 'NONE',  ( 15.24356964375000167, -3.323476615752272600, -1.003124999385444305 ) ) ;
#33276 = CARTESIAN_POINT ( 'NONE',  ( 13.56230152254411792, -5.196152422706638241, -9.375000000000078160 ) ) ;
#33277 = CARTESIAN_POINT ( 'NONE',  ( 15.00000000000000000, 0.000000000000000000, -5.849999999999994316 ) ) ;
#33278 = CARTESIAN_POINT ( 'NONE',  ( 21.00000000000000000, 6.646953231504538984, -8.353124999385492799 ) ) ;
#33279 = CARTESIAN_POINT ( 'NONE',  ( -11.61527771782819940, 76.53518628210146346, 4.622313124798574258 ) ) ;
#33280 = CARTESIAN_POINT ( 'NONE',  ( -15.53471296425195369, 132.0226862821014322, 2.908627838312118019 ) ) ;
#33281 = CARTESIAN_POINT ( 'NONE',  ( 27.78048522105927987, -5.196152422706632912, 161.9224404518259064 ) ) ;
#33282 = EDGE_CURVE ( 'NONE', #149, #21332, #8850, .T. ) ;
#33283 = CARTESIAN_POINT ( 'NONE',  ( 21.00000000000000000, 210.0000000000000000, 5.999999999999996447 ) ) ;
#33284 = CARTESIAN_POINT ( 'NONE',  ( -49.40252896937850124, 207.6499508600178387, -3.839350919129087547 ) ) ;
#33285 = CARTESIAN_POINT ( 'NONE',  ( 26.99999999999999289, 0.000000000000000000, 49.73803434254939759 ) ) ;
#33286 = CARTESIAN_POINT ( 'NONE',  ( 37.18746345154497845, -3.464101615137751278, 166.1812744261865475 ) ) ;
#33287 = CARTESIAN_POINT ( 'NONE',  ( -0.1745138560722763466, 137.5898137178985792, -12.50000000000000355 ) ) ;
#33288 = CARTESIAN_POINT ( 'NONE',  ( -40.89955436395488420, 214.8429017333601792, -4.673758765035196383 ) ) ;
#33289 = CARTESIAN_POINT ( 'NONE',  ( -54.75372103062156270, 218.5309553116391896, -2.162041339862839084 ) ) ;
#33290 = CARTESIAN_POINT ( 'NONE',  ( 20.99999999999999645, 6.646953231504538984, -2.165624999385510563 ) ) ;
#33291 = CARTESIAN_POINT ( 'NONE',  ( -27.24356964375000345, 199.3531250006145399, 0.000000000000000000 ) ) ;
#33292 = CARTESIAN_POINT ( 'NONE',  ( -3.257655550456946880, 118.9023137178985650, -15.46528703574811736 ) ) ;
#33293 = CARTESIAN_POINT ( 'NONE',  ( -48.01711230271182274, 216.4690446883607535, -1.857196546604089393 ) ) ;
#33294 = EDGE_CURVE ( 'NONE', #33538, #14209, #31124, .T. ) ;
#33295 = ORIENTED_EDGE ( 'NONE', *, *, #36699, .F. ) ;
#33296 =( BOUNDED_CURVE ( )  B_SPLINE_CURVE ( 2, ( #3743, #29333, #15509, #9628, #3369, #15316, #26869, #6781, #18356 ),
 .UNSPECIFIED., .F., .F. ) 
 B_SPLINE_CURVE_WITH_KNOTS ( ( 3, 2, 2, 2, 3 ),
 ( 0.4456521739130434590, 0.4492753623188405765, 0.4565217391304347561, 0.4637681159420289911, 0.4673913043478261087 ),
 .UNSPECIFIED. ) 
 CURVE ( )  GEOMETRIC_REPRESENTATION_ITEM ( )  RATIONAL_B_SPLINE_CURVE ( ( 0.9330127018922191873, 0.9330127018922187432, 1.000000000000000000, 0.8660254037844387076, 1.000000000000000000, 0.8660254037844387076, 1.000000000000000000, 0.9330127018922188542, 0.9330127018922194093 ) ) 
 REPRESENTATION_ITEM ( '' )  );
#33297 = CARTESIAN_POINT ( 'NONE',  ( 30.73311757145110690, -6.928203230275506996, 161.2500429106201523 ) ) ;
#33298 = CARTESIAN_POINT ( 'NONE',  ( -12.53471296425194836, 132.0226862821014606, 2.311890736173176641 ) ) ;
#33299 = CARTESIAN_POINT ( 'NONE',  ( 2.999999999999997335, 244.5000000000000000, -11.00000000000000000 ) ) ;
#33300 = CARTESIAN_POINT ( 'NONE',  ( 31.09835460584942624, -7.209453229046482114, 165.4247213166987081 ) ) ;
#33301 = VECTOR ( 'NONE', #8362, 1000.000000000000000 ) ;
#33302 = CARTESIAN_POINT ( 'NONE',  ( -15.46528703574804986, 95.79768628210145209, -3.257655550457287497 ) ) ;
#33303 = CARTESIAN_POINT ( 'NONE',  ( -57.32663769728823411, 204.3130714775002730, 3.149950860017883603 ) ) ;
#33304 = CARTESIAN_POINT ( 'NONE',  ( 19.68408634441910721, -5.407089921784855591, -4.490624999385572913 ) ) ;
#33305 = CARTESIAN_POINT ( 'NONE',  ( 3.474262827703335166, 37.43518628210144072, 8.843639120294326972 ) ) ;
#33306 = CARTESIAN_POINT ( 'NONE',  ( 15.00000000000000000, 0.000000000000000000, -2.643749998770955401 ) ) ;
#33307 = CARTESIAN_POINT ( 'NONE',  ( -40.70163769728823411, 217.4189793300686233, -4.149950860017907139 ) ) ;
#33308 = DIRECTION ( 'NONE',  ( 0.08715574274765150453, 0.000000000000000000, 0.9961946980917461003 ) ) ;
#33309 = CARTESIAN_POINT ( 'NONE',  ( -6.932735513423968321, 69.34768628210143504, -10.69584247140445221 ) ) ;
#33310 = CARTESIAN_POINT ( 'NONE',  ( 5.727106289114498080E-15, 199.2125000000000057, 31.17691453623979214 ) ) ;
#33311 = CARTESIAN_POINT ( 'NONE',  ( 10.56230152254321020, -3.464101615137235690, -7.949999998771044574 ) ) ;
#33313 = CARTESIAN_POINT ( 'NONE',  ( 13.44051670066911086, -5.407089921784865361, -0.5718749993855187785 ) ) ;
#33312 = CARTESIAN_POINT ( 'NONE',  ( -3.796722387233375073, 38.58518628210143930, 8.710071997420127943 ) ) ;
#33314 = DIRECTION ( 'NONE',  ( 0.000000000000000000, 0.000000000000000000, 1.000000000000000000 ) ) ;
#33315 = ORIENTED_EDGE ( 'NONE', *, *, #25845, .T. ) ;
#33316 = CARTESIAN_POINT ( 'NONE',  ( 26.99999999999999645, 7.347880794884117764E-16, -2.925000000000010925 ) ) ;
#33317 = CARTESIAN_POINT ( 'NONE',  ( 24.55824627498148160, -3.604726614523244610, 162.3078687509092788 ) ) ;
#33318 = CARTESIAN_POINT ( 'NONE',  ( 36.70701741954144381, -3.464101615137755275, 160.6897511517314285 ) ) ;
#33319 = CARTESIAN_POINT ( 'NONE',  ( 26.99999999999999645, 244.8625000000000114, -3.464101615137755275 ) ) ;
#33320 = CARTESIAN_POINT ( 'NONE',  ( 25.29522554115172639, 0.000000000000000000, 167.9369320615487311 ) ) ;
#33321 =( BOUNDED_CURVE ( )  B_SPLINE_CURVE ( 2, ( #28221, #5095, #22176, #2249, #11160, #13828, #8325, #2066, #31254 ),
 .UNSPECIFIED., .F., .F. ) 
 B_SPLINE_CURVE_WITH_KNOTS ( ( 3, 2, 2, 2, 3 ),
 ( 0.09782608695652174335, 0.1014492753623188470, 0.1086956521739130405, 0.1159420289855072478, 0.1195652173913043653 ),
 .UNSPECIFIED. ) 
 CURVE ( )  GEOMETRIC_REPRESENTATION_ITEM ( )  RATIONAL_B_SPLINE_CURVE ( ( 0.9330127018922194093, 0.9330127018922194093, 1.000000000000000000, 0.8660254037844387076, 1.000000000000000000, 0.8660254037844387076, 1.000000000000000000, 0.9330127018922190762, 0.9330127018922194093 ) ) 
 REPRESENTATION_ITEM ( '' )  );
#33322 = CARTESIAN_POINT ( 'NONE',  ( 7.228626920338837358, 76.92731371789857064, 10.49813415416005036 ) ) ;
#33323 = CARTESIAN_POINT ( 'NONE',  ( -4.622313124798576922, 78.83518628210146062, -11.61527771782819762 ) ) ;
#33324 = ORIENTED_EDGE ( 'NONE', *, *, #15199, .T. ) ;
#33325 = VERTEX_POINT ( 'NONE', #16943 ) ;
#33326 = CARTESIAN_POINT ( 'NONE',  ( 26.99999999999999645, 197.6750000012290513, -15.58845726811990495 ) ) ;
#33327 = CYLINDRICAL_SURFACE ( 'NONE', #7182, 6.000000000000001776 ) ;
#33328 = CARTESIAN_POINT ( 'NONE',  ( -0.1745138560722442889, 54.78981371789855359, -15.50000000000000533 ) ) ;
#33329 = CARTESIAN_POINT ( 'NONE',  ( 18.12178482187500350, -4.985214923628407568, -6.478124999385492799 ) ) ;
#33330 = CARTESIAN_POINT ( 'NONE',  ( 15.24356964374999990, 244.8718750006145513, -3.323476615752268604 ) ) ;
#33331 = CARTESIAN_POINT ( 'NONE',  ( -62.47247103062156981, 207.6499508600178387, 3.839350919129076445 ) ) ;
#33332 = CARTESIAN_POINT ( 'NONE',  ( 13.50000000000001421, 195.3125000012290400, 23.38268590217984055 ) ) ;
#33333 = CARTESIAN_POINT ( 'NONE',  ( 8.710071997420211432, 65.71481371789855075, -3.796722387233181895 ) ) ;
#33334 = EDGE_CURVE ( 'NONE', #22708, #25295, #12726, .T. ) ;
#33335 = CARTESIAN_POINT ( 'NONE',  ( 16.56230152254411081, 7.209453229046475009, -7.453124999385500438 ) ) ;
#33336 = ADVANCED_FACE ( 'NONE', ( #13350 ), #1965, .F. ) ;
#33337 = CARTESIAN_POINT ( 'NONE',  ( 1.715153634034445762, 119.4773137178985678, -9.534712964251895073 ) ) ;
#33338 = LINE ( 'NONE', #27089, #11324 ) ;
#33339 = CARTESIAN_POINT ( 'NONE',  ( 2.311890736173452865, 27.47731371789855004, -12.53471296425189152 ) ) ;
#33340 = EDGE_CURVE ( 'NONE', #36194, #30424, #22447, .T. ) ;
#33341 = CARTESIAN_POINT ( 'NONE',  ( -6.932735513423968321, 78.54768628210146630, -10.69584247140445221 ) ) ;
#33342 = CARTESIAN_POINT ( 'NONE',  ( 16.56230152254410726, 6.928203230275506996, -8.999999998771013310 ) ) ;
#33343 = ADVANCED_FACE ( 'NONE', ( #4993 ), #28485, .F. ) ;
#33344 = DIRECTION ( 'NONE',  ( -2.057406622567553763E-16, 0.000000000000000000, 1.000000000000000000 ) ) ;
#33345 = CARTESIAN_POINT ( 'NONE',  ( 24.56314878551103575, -3.604726614523240613, 162.3639047026768765 ) ) ;
#33346 = CARTESIAN_POINT ( 'NONE',  ( 19.68408634441912142, -5.407089921784861808, -6.796874999385527083 ) ) ;
#33347 = CARTESIAN_POINT ( 'NONE',  ( 24.89648801797452293, -3.464101615138005741, 163.3793413165545587 ) ) ;
#33348 = CARTESIAN_POINT ( 'NONE',  ( 15.00000000000000178, 0.000000000000000000, -3.993749998770945719 ) ) ;
#33349 = CARTESIAN_POINT ( 'NONE',  ( 0.5000000000000000000, 244.5000000000000000, 0.000000000000000000 ) ) ;
#33350 = CARTESIAN_POINT ( 'NONE',  ( -3.796722387233375073, 93.78518628210144925, 8.710071997420127943 ) ) ;
#33351 = DIRECTION ( 'NONE',  ( 0.000000000000000000, 0.000000000000000000, 1.000000000000000000 ) ) ;
#33352 = CARTESIAN_POINT ( 'NONE',  ( 2.311890736173175753, 129.7226862821014777, 12.53471296425194836 ) ) ;
#33353 = CARTESIAN_POINT ( 'NONE',  ( -10.07132003121360775, 143.0000000000000000, 4.865397298893943123 ) ) ;
#33354 = CARTESIAN_POINT ( 'NONE',  ( 21.00000000000000000, 249.7468750006145797, -6.646953231504538984 ) ) ;
#33356 = EDGE_LOOP ( 'NONE', ( #34603, #15467, #6503, #36718 ) ) ;
#33355 = AXIS2_PLACEMENT_3D ( 'NONE', #7648, #4791, #13515 ) ;
#33357 = CARTESIAN_POINT ( 'NONE',  ( 30.94637677943320497, -7.209453229046475009, 163.6876068119011904 ) ) ;
#33358 = CARTESIAN_POINT ( 'NONE',  ( 26.75643035624999655, 3.323476615752271712, -5.278124999385452654 ) ) ;
#33359 = CARTESIAN_POINT ( 'NONE',  ( -27.24356964375000345, 197.6093750006145342, 0.000000000000000000 ) ) ;
#33360 = CARTESIAN_POINT ( 'NONE',  ( 37.41624727615045742, 7.347880794884125653E-16, 168.7962855074530069 ) ) ;
#33361 = CARTESIAN_POINT ( 'NONE',  ( 33.67594490067671842, -5.196152422706635576, 160.4655734646546534 ) ) ;
#33362 = CARTESIAN_POINT ( 'NONE',  ( 21.00000000000000000, 242.3218750006145115, 6.646953231504538984 ) ) ;
#33363 = CARTESIAN_POINT ( 'NONE',  ( 6.932735513424201024, 138.4523137178985621, -10.69584247140429412 ) ) ;
#33364 = CARTESIAN_POINT ( 'NONE',  ( -27.24356964375000345, 197.1218750006145513, -15.72908226750537786 ) ) ;
#33366 = ORIENTED_EDGE ( 'NONE', *, *, #27555, .F. ) ;
#33365 = ORIENTED_EDGE ( 'NONE', *, *, #20123, .F. ) ;
#33367 = CARTESIAN_POINT ( 'NONE',  ( 21.00000000000000000, 243.5593750006145228, 6.646953231504538984 ) ) ;
#33368 = CARTESIAN_POINT ( 'NONE',  ( 4.944772684328420986, 22.01481371789855501, 11.48171059495408208 ) ) ;
#33369 = CARTESIAN_POINT ( 'NONE',  ( 15.24356964375000167, -3.323476615752272600, -4.153124999385478411 ) ) ;
#33370 = CARTESIAN_POINT ( 'NONE',  ( 3.257655550456945548, 105.1023137178985678, 15.46528703574811736 ) ) ;
#33371 = CARTESIAN_POINT ( 'NONE',  ( 14.45804369857214589, -5.892651062571511389, -9.999999999999991118 ) ) ;
#33372 = CARTESIAN_POINT ( 'NONE',  ( 26.99999999999999645, -3.464101615137751278, -10.10624999877097352 ) ) ;
#33373 = ORIENTED_EDGE ( 'NONE', *, *, #29160, .T. ) ;
#33374 = CARTESIAN_POINT ( 'NONE',  ( 16.56230152254411081, -7.209453229046482114, -6.834374999385501859 ) ) ;
#33375 = EDGE_LOOP ( 'NONE', ( #34373, #22544, #11438, #26218 ) ) ;
#33376 = CARTESIAN_POINT ( 'NONE',  ( -13.62178482187498396, 196.2781250006145228, 23.59362340125808188 ) ) ;
#33377 = CARTESIAN_POINT ( 'NONE',  ( 2.660918448318279950, 125.6976862821014578, -12.46528703574805697 ) ) ;
#33378 = CARTESIAN_POINT ( 'NONE',  ( -72.05441616160760532, 219.4495263357960368, 5.000000000000000000 ) ) ;
#33379 = MANIFOLD_SOLID_BREP ( 'Thread1', #19303 ) ;
#33380 = CARTESIAN_POINT ( 'NONE',  ( 30.80420397407610622, 7.209453229046482114, 162.0625642106390671 ) ) ;
#33381 = AXIS2_PLACEMENT_3D ( 'NONE', #13525, #31839, #32215 ) ;
#33382 = CARTESIAN_POINT ( 'NONE',  ( -55.53794563604517975, 203.8621396198271043, 6.307003348498029460 ) ) ;
#33383 = CARTESIAN_POINT ( 'NONE',  ( 15.24356964374999990, 246.5968750006145171, 0.000000000000000000 ) ) ;
#33384 = LINE ( 'NONE', #19552, #10351 ) ;
#33385 = CARTESIAN_POINT ( 'NONE',  ( -30.40252896937850124, 207.6499508600178387, -3.839350919129087547 ) ) ;
#33386 = CARTESIAN_POINT ( 'NONE',  ( 12.53471296425194836, 136.6226862821014834, -2.311890736173178418 ) ) ;
#33387 = CARTESIAN_POINT ( 'NONE',  ( 10.56230152254411081, 0.000000000000000000, -2.137499998771025034 ) ) ;
#33388 = ORIENTED_EDGE ( 'NONE', *, *, #26483, .T. ) ;
#33389 = CARTESIAN_POINT ( 'NONE',  ( 13.50000000000001421, 195.3125000012290400, 23.38268590217984055 ) ) ;
#33390 = CARTESIAN_POINT ( 'NONE',  ( 14.38691631536207538, 117.9351862821014407, -5.770363421893813793 ) ) ;
#33391 = CARTESIAN_POINT ( 'NONE',  ( 6.594114490232313663, 110.4601862821014606, 6.840914352312096547 ) ) ;
#33392 = CARTESIAN_POINT ( 'NONE',  ( 13.50000000000001421, 199.2500000000000000, 23.38268590217984055 ) ) ;
#33393 = CARTESIAN_POINT ( 'NONE',  ( 12.50000000000000355, 8.110186282101444988, 0.1745138560725507937 ) ) ;
#33394 = B_SPLINE_CURVE_WITH_KNOTS ( 'NONE', 3,
 ( #35251, #18406, #6644, #9305 ),
 .UNSPECIFIED., .F., .F.,
 ( 4, 4 ),
 ( 0.000000000000000000, 1.000000000000000000 ),
 .UNSPECIFIED. ) ;
#33395 = CARTESIAN_POINT ( 'NONE',  ( 19.56230152254412147, -5.196152422706635576, -9.750000000000063949 ) ) ;
#33396 = ORIENTED_EDGE ( 'NONE', *, *, #2504, .T. ) ;
#33397 = CARTESIAN_POINT ( 'NONE',  ( 29.49486714975617474, 6.148716665048037378, 159.5363409456820136 ) ) ;
#33398 = CARTESIAN_POINT ( 'NONE',  ( -9.534712964251941258, 86.02268628210144641, 1.715153634034234154 ) ) ;
#33399 = CARTESIAN_POINT ( 'NONE',  ( -6.594114490232462877, 124.9398137178985451, 6.840914352311949109 ) ) ;
#33400 = CARTESIAN_POINT ( 'NONE',  ( -1.926257025242585782E-15, 195.1906250006145456, -31.45816453501075927 ) ) ;
#33401 = CARTESIAN_POINT ( 'NONE',  ( 26.99999999999999645, 7.347880794884117764E-16, -2.024999999999999023 ) ) ;
#33402 = CARTESIAN_POINT ( 'NONE',  ( -27.24356964374999990, 198.0218750006145569, -15.72908226750537786 ) ) ;
#33403 = CARTESIAN_POINT ( 'NONE',  ( -14.50000000000000000, 215.7563705986615901, 5.555555555555558023 ) ) ;
#33404 = CARTESIAN_POINT ( 'NONE',  ( 22.60769515458672885, 243.8325961894323086, 5.999999999999997335 ) ) ;
#33405 = CARTESIAN_POINT ( 'NONE',  ( -8.152565276336593669, 62.55231371789854222, -5.233372021372610483 ) ) ;
#33406 = ORIENTED_EDGE ( 'NONE', *, *, #19711, .T. ) ;
#33407 = VECTOR ( 'NONE', #17733, 1000.000000000000000 ) ;
#33408 = CARTESIAN_POINT ( 'NONE',  ( 15.00000000000000000, 243.7562500012290627, 0.000000000000000000 ) ) ;
#33409 = CARTESIAN_POINT ( 'NONE',  ( -12.50000000000000355, 80.08981371789855075, 0.1745138560722786503 ) ) ;
#33410 = CARTESIAN_POINT ( 'NONE',  ( 22.80587116629412847, 3.604726614523243278, -6.234374999385518201 ) ) ;
#33411 = FACE_OUTER_BOUND ( 'NONE', #17838, .T. ) ;
#33412 = CARTESIAN_POINT ( 'NONE',  ( 23.87821517812500005, -4.985214923628404016, -5.953124999385495109 ) ) ;
#33413 = CARTESIAN_POINT ( 'NONE',  ( 0.1745138560722779009, 40.98981371789854933, 12.50000000000000355 ) ) ;
#33414 = ORIENTED_EDGE ( 'NONE', *, *, #29259, .T. ) ;
#33415 = CARTESIAN_POINT ( 'NONE',  ( 18.12178482187500350, -4.985214923628407568, -6.365624999385477878 ) ) ;
#33416 = CARTESIAN_POINT ( 'NONE',  ( 12.53471296425194836, 26.22268628210144925, -2.311890736173178418 ) ) ;
#33417 = CARTESIAN_POINT ( 'NONE',  ( 37.60577953318700395, 3.604726614523243278, 168.1680008707037075 ) ) ;
#33418 = CARTESIAN_POINT ( 'NONE',  ( -51.57961230271182274, 211.8571965466040297, 6.469044688360755302 ) ) ;
#33419 = VECTOR ( 'NONE', #12316, 1000.000000000000000 ) ;
#33420 = CARTESIAN_POINT ( 'NONE',  ( 29.51984228635672380, 5.908847293266075162, 159.3365288790247121 ) ) ;
#33421 = CARTESIAN_POINT ( 'NONE',  ( -12.50000000000000355, 61.68981371789855928, 0.1745138560722786503 ) ) ;
#33422 = CARTESIAN_POINT ( 'NONE',  ( -50.59747103062156981, 212.3500491399821613, -3.839350919129076445 ) ) ;
#33423 = CARTESIAN_POINT ( 'NONE',  ( -55.74330436395489841, 210.1155267958017134, -6.500000000000000888 ) ) ;
#33424 = CARTESIAN_POINT ( 'NONE',  ( 10.56230152254495103, 3.464101615138235335, -1.724999998771002074 ) ) ;
#33425 = CARTESIAN_POINT ( 'NONE',  ( 8.632099005475788900, 37.25231371789855217, -13.23911966647199812 ) ) ;
#33426 = CARTESIAN_POINT ( 'NONE',  ( -44.45461230271183695, 207.6069050685336492, -8.469044688360751749 ) ) ;
#33427 = CARTESIAN_POINT ( 'NONE',  ( 27.00000000000000355, 199.7750000000000057, -3.306546357697854128E-15 ) ) ;
#33428 = CARTESIAN_POINT ( 'NONE',  ( 6.932735513423970097, 64.74768628210145494, 10.69584247140445044 ) ) ;
#33429 = CARTESIAN_POINT ( 'NONE',  ( 0.1745138560725837118, 15.01018628210143291, -15.50000000000000533 ) ) ;
#33430 = CARTESIAN_POINT ( 'NONE',  ( 16.56230152254411436, -6.928203230275514990, -1.237499999999996270 ) ) ;
#33431 = DIRECTION ( 'NONE',  ( 0.000000000000000000, 0.000000000000000000, 1.000000000000000000 ) ) ;
#33432 = ORIENTED_EDGE ( 'NONE', *, *, #676, .T. ) ;
#33433 = CARTESIAN_POINT ( 'NONE',  ( -13.04141134922759804, 22.77268628210143220, -8.927990412390657937 ) ) ;
#33434 = CARTESIAN_POINT ( 'NONE',  ( 13.62178482187499640, 197.4031250006145228, -23.59362340125807123 ) ) ;
#33435 = CARTESIAN_POINT ( 'NONE',  ( 22.56230152254542887, 3.464101615136989665, -8.624999998771029297 ) ) ;
#33436 = CYLINDRICAL_SURFACE ( 'NONE', #14139, 5.999999999999998224 ) ;
#33437 = DIRECTION ( 'NONE',  ( 0.000000000000000000, 0.000000000000000000, -1.000000000000000000 ) ) ;
#33438 = FACE_OUTER_BOUND ( 'NONE', #25479, .T. ) ;
#33439 = CARTESIAN_POINT ( 'NONE',  ( -1.045839947578415010E-13, 196.1750000012290229, 27.00000000000000355 ) ) ;
#33440 = CARTESIAN_POINT ( 'NONE',  ( 15.24356964374999990, 247.1593750006145171, 0.000000000000000000 ) ) ;
#33441 = CARTESIAN_POINT ( 'NONE',  ( 1.715153634034445762, 119.4773137178985678, -9.534712964251895073 ) ) ;
#33442 = CARTESIAN_POINT ( 'NONE',  ( 20.99999999999999645, 245.0218750006145285, 6.646953231504538984 ) ) ;
#33443 = EDGE_LOOP ( 'NONE', ( #23086, #14236, #10384, #19584 ) ) ;
#33444 = CARTESIAN_POINT ( 'NONE',  ( 26.99999999999999289, 0.000000000000000000, -8.000000000000000000 ) ) ;
#33445 = CARTESIAN_POINT ( 'NONE',  ( -2.311890736173447980, 142.4773137178985678, 12.53471296425189330 ) ) ;
#33446 = CARTESIAN_POINT ( 'NONE',  ( 16.56230152254410726, -7.209453229046475009, -8.578124999385506655 ) ) ;
#33447 = CARTESIAN_POINT ( 'NONE',  ( 34.13799077639428958, -5.407089921784855591, 164.3494578665133474 ) ) ;
#33448 = DIRECTION ( 'NONE',  ( 0.000000000000000000, 0.000000000000000000, -1.000000000000000000 ) ) ;
#33449 = CARTESIAN_POINT ( 'NONE',  ( -13.50000000000000533, 197.6750000000000114, -23.38268590217984411 ) ) ;
#33450 = AXIS2_PLACEMENT_3D ( 'NONE', #8341, #29863, #35354 ) ;
#33451 = EDGE_CURVE ( 'NONE', #19674, #32379, #16610, .T. ) ;
#33452 = EDGE_LOOP ( 'NONE', ( #24595, #2659, #1001, #15773 ) ) ;
#33453 = CARTESIAN_POINT ( 'NONE',  ( -12.53471296425194659, 30.82268628210144001, 2.311890736173176641 ) ) ;
#33454 = ORIENTED_EDGE ( 'NONE', *, *, #16324, .T. ) ;
#33455 = VERTEX_POINT ( 'NONE', #11988 ) ;
#33456 = CARTESIAN_POINT ( 'NONE',  ( 21.00000000000000000, -6.928203230275506996, -4.781249998770952914 ) ) ;
#33457 = DIRECTION ( 'NONE',  ( -0.000000000000000000, -0.000000000000000000, -1.000000000000000000 ) ) ;
#33458 = CARTESIAN_POINT ( 'NONE',  ( 10.56230152254410548, 0.000000000000000000, -9.450000000000041922 ) ) ;
#33459 = CARTESIAN_POINT ( 'NONE',  ( 18.00000000000000000, 5.196152422706630247, -4.574999999999995737 ) ) ;
#33460 = CARTESIAN_POINT ( 'NONE',  ( 23.87821517812500005, -4.985214923628404016, -9.440624999385471838 ) ) ;
#33461 = CARTESIAN_POINT ( 'NONE',  ( 4.944772684328679446, 70.78518628210144925, -11.48171059495397373 ) ) ;
#33462 = CARTESIAN_POINT ( 'NONE',  ( -3.257655550456946880, 8.502313717898553946, -15.46528703574811736 ) ) ;
#33463 = CARTESIAN_POINT ( 'NONE',  ( -26.99999999999999645, 197.3375000000000057, 15.58845726811991561 ) ) ;
#33464 = ADVANCED_FACE ( 'NONE', ( #29036 ), #14280, .T. ) ;
#33465 = CARTESIAN_POINT ( 'NONE',  ( 18.00000000000000000, 243.6812500012290457, -5.196152422706630247 ) ) ;
#33466 = CARTESIAN_POINT ( 'NONE',  ( -61.07961230271182984, 211.3212981617417938, 4.469044688360757966 ) ) ;
#33467 = DIRECTION ( 'NONE',  ( -0.000000000000000000, 1.000000000000000000, -0.000000000000000000 ) ) ;
#33468 = CARTESIAN_POINT ( 'NONE',  ( 34.27405118538959528, -5.196152422706629359, 167.3019595815335947 ) ) ;
#33469 = CARTESIAN_POINT ( 'NONE',  ( -11.48171059495408208, 125.5148137178985763, 4.944772684328421875 ) ) ;
#33470 = CARTESIAN_POINT ( 'NONE',  ( -43.67038769728823411, 208.1428034533959703, 6.469044688360770401 ) ) ;
#33471 = CARTESIAN_POINT ( 'NONE',  ( -55.54538769728824832, 212.3930949314662371, -8.469044688360781947 ) ) ;
#33472 = CARTESIAN_POINT ( 'NONE',  ( 26.75643035624999655, 7.049594010296217766E-16, -1.828124999385477567 ) ) ;
#33473 = CARTESIAN_POINT ( 'NONE',  ( -13.62178482187500528, 196.5781250006145342, -23.59362340125807123 ) ) ;
#33474 = CARTESIAN_POINT ( 'NONE',  ( -15.46528703574811736, 98.20231371789854791, 3.257655550456946436 ) ) ;
#33475 = CARTESIAN_POINT ( 'NONE',  ( -41.88169563604517265, 210.1155267958017703, 6.500000000000000888 ) ) ;
#33476 = EDGE_CURVE ( 'NONE', #10799, #30158, #20462, .T. ) ;
#33477 = ORIENTED_EDGE ( 'NONE', *, *, #11457, .F. ) ;
#33478 = CARTESIAN_POINT ( 'NONE',  ( 36.71682244070834855, -3.464101615137353374, 160.8018230564910027 ) ) ;
#33479 = CARTESIAN_POINT ( 'NONE',  ( -11.61527771782819940, 122.5351862821014635, 4.622313124798574258 ) ) ;
#33480 = CARTESIAN_POINT ( 'NONE',  ( -15.46528703574804986, 77.39768628210144641, -3.257655550457287497 ) ) ;
#33481 = CARTESIAN_POINT ( 'NONE',  ( 15.24356964374999990, 249.8593750006145342, 0.000000000000000000 ) ) ;
#33482 = CARTESIAN_POINT ( 'NONE',  ( 27.86752052465190133, -5.407089921784865361, 164.3145826479452296 ) ) ;
#33483 = CARTESIAN_POINT ( 'NONE',  ( 0.1745138560725837118, 88.61018628210146630, -15.50000000000000533 ) ) ;
#33484 = CARTESIAN_POINT ( 'NONE',  ( -58.71205436395489841, 214.6737587650351884, 4.842901733360205796 ) ) ;
#33485 = CARTESIAN_POINT ( 'NONE',  ( 16.56230152254410015, -7.209453229046475009, -4.078124999385484450 ) ) ;
#33486 = CARTESIAN_POINT ( 'NONE',  ( 1.715153634034233487, 46.92268628210143788, 9.534712964251941258 ) ) ;
#33487 = CARTESIAN_POINT ( 'NONE',  ( 0.000000000000000000, 148.0000000000000000, 0.000000000000000000 ) ) ;
#33488 = CARTESIAN_POINT ( 'NONE',  ( -36.74330436395489130, 210.1155267958016850, -8.500000000000003553 ) ) ;
#33489 = CARTESIAN_POINT ( 'NONE',  ( 22.80587116629412137, 7.646167579472024665E-16, -9.421874999385515537 ) ) ;
#33490 = CARTESIAN_POINT ( 'NONE',  ( -11.48171059495397373, 50.08518628210144641, -4.944772684328680334 ) ) ;
#33491 = CARTESIAN_POINT ( 'NONE',  ( 22.56230152254412147, 7.347880794884125653E-16, -8.325000000000027711 ) ) ;
#33492 = CARTESIAN_POINT ( 'NONE',  ( 24.56230152254410726, 0.000000000000000000, 2.535898384862258492 ) ) ;
#33494 = CARTESIAN_POINT ( 'NONE',  ( 16.56230152254411436, -7.209453229046482114, -0.5343749993854981506 ) ) ;
#33493 = CARTESIAN_POINT ( 'NONE',  ( 9.465287035748067623, 35.99768628210143362, 2.064181346179272847 ) ) ;
#33495 = LINE ( 'NONE', #21950, #6435 ) ;
#33496 = ORIENTED_EDGE ( 'NONE', *, *, #5464, .F. ) ;
#33497 = CARTESIAN_POINT ( 'NONE',  ( 21.00000000000000000, 6.928203230275506996, -1.462500000000010125 ) ) ;
#33498 = STYLED_ITEM ( 'NONE', ( #12582 ), #21035 ) ;
#33499 = CARTESIAN_POINT ( 'NONE',  ( 24.63341810310133084, 0.000000000000000000, 163.1670866780133906 ) ) ;
#33500 = CARTESIAN_POINT ( 'NONE',  ( 33.84589859903464060, 5.196152422706637353, 162.4081531259335804 ) ) ;
#33501 = CARTESIAN_POINT ( 'NONE',  ( 21.00000000000000000, 246.5125000000000171, 6.928203230275506996 ) ) ;
#33502 = CARTESIAN_POINT ( 'NONE',  ( 10.49999999999999467, 222.9518338469886203, -12.50000000000000000 ) ) ;
#33503 = CARTESIAN_POINT ( 'NONE',  ( -11.61527771782809282, 80.66481371789856780, -4.622313124798832717 ) ) ;
#33504 = CARTESIAN_POINT ( 'NONE',  ( 0.1745138560725515708, 88.61018628210146630, -12.50000000000000355 ) ) ;
#33505 = ORIENTED_EDGE ( 'NONE', *, *, #1699, .T. ) ;
#33506 = VERTEX_POINT ( 'NONE', #11431 ) ;
#33507 = CARTESIAN_POINT ( 'NONE',  ( -26.99999999999998934, 197.4500000012290570, 15.58845726811991561 ) ) ;
#33508 = CARTESIAN_POINT ( 'NONE',  ( -13.49999999999998401, 196.9250000000000114, 23.38268590217985476 ) ) ;
#33509 = EDGE_CURVE ( 'NONE', #20600, #21259, #28218, .T. ) ;
#33510 = CARTESIAN_POINT ( 'NONE',  ( 2.908627838312458636, 64.27731371789853654, -15.53471296425188442 ) ) ;
#33511 = CARTESIAN_POINT ( 'NONE',  ( 21.00000000000000000, 6.646953231504538984, -6.215624999385504168 ) ) ;
#33512 = CARTESIAN_POINT ( 'NONE',  ( 18.12178482187499640, 245.2843750006145456, -4.985214923628404904 ) ) ;
#33513 = AXIS2_PLACEMENT_3D ( 'NONE', #30185, #4772, #10458 ) ;
#33514 = CARTESIAN_POINT ( 'NONE',  ( -57.52455436395489841, 206.6211998817774997, 3.209657149897401585 ) ) ;
#33515 = CARTESIAN_POINT ( 'NONE',  ( -27.00000000000000355, 199.5500000000000114, 0.000000000000000000 ) ) ;
#33516 = CARTESIAN_POINT ( 'NONE',  ( -2.064181346179062349, 45.30231371789854933, -9.465287035748106703 ) ) ;
#33517 = CARTESIAN_POINT ( 'NONE',  ( 10.31873187879410736, -3.604726614523240613, -8.203124999385504879 ) ) ;
#33518 =( BOUNDED_CURVE ( )  B_SPLINE_CURVE ( 2, ( #27531, #8000, #31125, #4590, #13128, #2303, #24682 ),
 .UNSPECIFIED., .F., .F. ) 
 B_SPLINE_CURVE_WITH_KNOTS ( ( 3, 2, 2, 3 ),
 ( 0.3478260869565210633, 0.3550724637681153539, 0.3623188405797096445, 0.3695652173913038796 ),
 .UNSPECIFIED. ) 
 CURVE ( )  GEOMETRIC_REPRESENTATION_ITEM ( )  RATIONAL_B_SPLINE_CURVE ( ( 1.000000000000012212, 0.8660254037844263841, 1.000000000000000000, 0.8660254037844387076, 1.000000000000000000, 0.8660254037844469233, 0.9999999999999917843 ) ) 
 REPRESENTATION_ITEM ( '' )  );
#33519 = CARTESIAN_POINT ( 'NONE',  ( 2.064181346179061460, 95.90231371789855075, 9.465287035748106703 ) ) ;
#33520 = CARTESIAN_POINT ( 'NONE',  ( -13.62178482187500528, 198.4343750006145228, -23.59362340125807123 ) ) ;
#33521 = CARTESIAN_POINT ( 'NONE',  ( -4.622313124798826500, 32.36481371789854933, 11.61527771782809637 ) ) ;
#33522 = CARTESIAN_POINT ( 'NONE',  ( -4.944772684328673229, 75.38518628210144357, 11.48171059495397728 ) ) ;
#33523 = CARTESIAN_POINT ( 'NONE',  ( 13.56230152254411614, -5.196152422706632912, -9.262499998771044574 ) ) ;
#33524 = AXIS2_PLACEMENT_3D ( 'NONE', #25516, #10928, #34050 ) ;
#33525 = DIRECTION ( 'NONE',  ( -0.000000000000000000, -1.000000000000000000, -0.000000000000000000 ) ) ;
#33526 = CARTESIAN_POINT ( 'NONE',  ( 27.66324925258708589, 5.407089921784856479, 161.9797513242927209 ) ) ;
#33527 = CARTESIAN_POINT ( 'NONE',  ( 15.00000000000000000, 3.464101615137752166, -0.8812499987709473404 ) ) ;
#33528 = CARTESIAN_POINT ( 'NONE',  ( 22.80587116629411781, 3.604726614523243278, -5.784374999385522464 ) ) ;
#33529 = CARTESIAN_POINT ( 'NONE',  ( 33.87204532185894124, -5.196152422706635576, 162.7070115353610618 ) ) ;
#33530 = CARTESIAN_POINT ( 'NONE',  ( 15.00000000000000000, 0.000000000000000000, -4.049999999999998046 ) ) ;
#33531 = CARTESIAN_POINT ( 'NONE',  ( -8.152565276336710909, 94.64768628210147483, 5.233372021372435512 ) ) ;
#33532 = CARTESIAN_POINT ( 'NONE',  ( 19.56230152254412502, 5.196152422706637353, -6.000000000000060396 ) ) ;
#33533 = EDGE_CURVE ( 'NONE', #33538, #10561, #29423, .T. ) ;
#33534 =( BOUNDED_CURVE ( )  B_SPLINE_CURVE ( 2, ( #32713, #15287, #9969, #1243, #4279, #21732, #33465, #1433, #24011 ),
 .UNSPECIFIED., .F., .F. ) 
 B_SPLINE_CURVE_WITH_KNOTS ( ( 3, 2, 2, 2, 3 ),
 ( 0.5543478260869565410, 0.5579710144927536586, 0.5652173913043477826, 0.5724637681159420177, 0.5760869565217391353 ),
 .UNSPECIFIED. ) 
 CURVE ( )  GEOMETRIC_REPRESENTATION_ITEM ( )  RATIONAL_B_SPLINE_CURVE ( ( 0.9330127018922194093, 0.9330127018922194093, 1.000000000000000000, 0.8660254037844387076, 1.000000000000000000, 0.8660254037844387076, 1.000000000000000000, 0.9330127018922194093, 0.9330127018922194093 ) ) 
 REPRESENTATION_ITEM ( '' )  );
#33535 = CARTESIAN_POINT ( 'NONE',  ( -11.48171059495397373, 123.6851862821014549, -4.944772684328680334 ) ) ;
#33536 = CARTESIAN_POINT ( 'NONE',  ( 10.56230152254307519, 3.464101615137159751, -4.537500000000036948 ) ) ;
#33537 = CARTESIAN_POINT ( 'NONE',  ( 26.75643035624999655, 249.5968750006145171, 3.323476615752267715 ) ) ;
#33538 = VERTEX_POINT ( 'NONE', #17313 ) ;
#33539 = CARTESIAN_POINT ( 'NONE',  ( 24.87037277869651319, 3.604726614523236616, 165.8754910134502722 ) ) ;
#33540 = CARTESIAN_POINT ( 'NONE',  ( 23.87821517812499650, 4.985214923628404904, -5.690624999385468286 ) ) ;
#33541 = CARTESIAN_POINT ( 'NONE',  ( 13.62178482187501416, 197.3093750006145513, 23.59362340125806767 ) ) ;
#33542 = CYLINDRICAL_SURFACE ( 'NONE', #937, 7.500000000000000000 ) ;
#33543 = CARTESIAN_POINT ( 'NONE',  ( 19.39230484541326760, 239.7986538117967257, 5.999999999999999112 ) ) ;
#33544 = CARTESIAN_POINT ( 'NONE',  ( 21.00000000000000000, 244.1218750006145513, 6.646953231504538984 ) ) ;
#33545 = FACE_OUTER_BOUND ( 'NONE', #16675, .T. ) ;
#33546 = CARTESIAN_POINT ( 'NONE',  ( -8.843639120294245259, 7.064813717898548617, -3.474262827703533230 ) ) ;
#33547 = CARTESIAN_POINT ( 'NONE',  ( -12.53471296425194659, 141.2226862821014777, 2.311890736173176641 ) ) ;
#33549 = ORIENTED_EDGE ( 'NONE', *, *, #13312, .T. ) ;
#33548 = ORIENTED_EDGE ( 'NONE', *, *, #27085, .F. ) ;
#33550 = AXIS2_PLACEMENT_3D ( 'NONE', #8786, #20167, #23195 ) ;
#33551 = AXIS2_PLACEMENT_3D ( 'NONE', #25862, #20561, #8255 ) ;
#33552 = CARTESIAN_POINT ( 'NONE',  ( 26.75643035624999655, 245.0218750006145001, -7.049594010296217766E-16 ) ) ;
#33553 = CARTESIAN_POINT ( 'NONE',  ( -77.00000000000002842, 210.0000000000000000, -2.499999999999998668 ) ) ;
#33554 = EDGE_CURVE ( 'NONE', #21332, #8445, #34733, .T. ) ;
#33555 =( GEOMETRIC_REPRESENTATION_CONTEXT ( 3 ) GLOBAL_UNCERTAINTY_ASSIGNED_CONTEXT ( ( #4786 ) ) GLOBAL_UNIT_ASSIGNED_CONTEXT ( ( #19083, #36298, #25491 ) ) REPRESENTATION_CONTEXT ( 'NONE', 'WORKASPACE' ) );
#33556 = CARTESIAN_POINT ( 'NONE',  ( 26.75643035624999655, -3.323476615752267715, -4.903124999385481964 ) ) ;
#33557 = CARTESIAN_POINT ( 'NONE',  ( 10.83675517735179206, 120.3398137178985507, -11.08355503943118769 ) ) ;
#33559 = CARTESIAN_POINT ( 'NONE',  ( 11.73492611592313573, -4.045813723653100880, -9.999999999999998224 ) ) ;
#33558 = MECHANICAL_DESIGN_GEOMETRIC_PRESENTATION_REPRESENTATION (  '', ( #12361 ), #28697 ) ;
#33560 = CARTESIAN_POINT ( 'NONE',  ( 21.00000000000000000, -6.928203230275506996, -9.731249998770937992 ) ) ;
#33561 = EDGE_CURVE ( 'NONE', #25530, #11819, #8777, .T. ) ;
#33562 = CARTESIAN_POINT ( 'NONE',  ( 19.68408634441911076, 5.407089921784862696, -7.546874999385555505 ) ) ;
#33563 = EDGE_LOOP ( 'NONE', ( #12718, #36380, #4825, #34320 ) ) ;
#33564 = CARTESIAN_POINT ( 'NONE',  ( 27.00000000000001066, 199.4000000012290172, 15.58845726811988897 ) ) ;
#33565 = CARTESIAN_POINT ( 'NONE',  ( -11.61527771782819940, 140.9351862821014834, 4.622313124798574258 ) ) ;
#33566 = CARTESIAN_POINT ( 'NONE',  ( 22.80587116629410716, 3.604726614523238837, -0.3281249993855308023 ) ) ;
#33567 = CARTESIAN_POINT ( 'NONE',  ( 37.08938175740716758, -3.604726614523238837, 162.2655472845100917 ) ) ;
#33568 = CARTESIAN_POINT ( 'NONE',  ( -55.93377896937850124, 207.8379586601372750, 8.530955311639258909 ) ) ;
#33569 = CARTESIAN_POINT ( 'NONE',  ( 20.99999999999999645, 247.1593750006145171, 6.646953231504538984 ) ) ;
#33570 =( NAMED_UNIT ( * ) PLANE_ANGLE_UNIT ( ) SI_UNIT ( $, .RADIAN. ) );
#33571 = CARTESIAN_POINT ( 'NONE',  ( 22.56230152254391896, -3.464101615137866741, -2.849999998770999632 ) ) ;
#33572 = CARTESIAN_POINT ( 'NONE',  ( -38.91294563604516554, 213.2096571498974527, -3.378800118222469617 ) ) ;
#33573 = CARTESIAN_POINT ( 'NONE',  ( -4.944772684328673229, 130.5851862821014606, 11.48171059495397728 ) ) ;
#33574 = CARTESIAN_POINT ( 'NONE',  ( 19.56230152254411792, -5.196152422706629359, -1.537499998771035825 ) ) ;
#33575 = VERTEX_POINT ( 'NONE', #11245 ) ;
#33576 = CARTESIAN_POINT ( 'NONE',  ( 15.00000000000000355, 7.347880794884112834E-16, -8.000000000000000000 ) ) ;
#33577 = CARTESIAN_POINT ( 'NONE',  ( 15.00000000000000000, 244.6000000000000227, 0.000000000000000000 ) ) ;
#33578 = CARTESIAN_POINT ( 'NONE',  ( -8.927990412390661490, 121.6726862821014521, 13.04141134922759804 ) ) ;
#33579 = CYLINDRICAL_SURFACE ( 'NONE', #35092, 1.500000000000001332 ) ;
#33580 = CARTESIAN_POINT ( 'NONE',  ( 10.69584247140445221, 16.44768628210144001, -6.932735513423970097 ) ) ;
#33581 = CARTESIAN_POINT ( 'NONE',  ( 13.56230152254410548, 5.196152422706636465, -9.525000000000034106 ) ) ;
#33582 = EDGE_LOOP ( 'NONE', ( #18212, #34377, #33642, #599 ) ) ;
#33583 = CARTESIAN_POINT ( 'NONE',  ( 21.00000000000000000, 210.0000000000000284, 8.000000000000000000 ) ) ;
#33584 = CARTESIAN_POINT ( 'NONE',  ( -0.1745138560725182642, 84.01018628210145778, 9.500000000000005329 ) ) ;
#33585 = CARTESIAN_POINT ( 'NONE',  ( 5.529263428287300108, 132.1273137178985735, 7.954856959092309943 ) ) ;
#33586 = CARTESIAN_POINT ( 'NONE',  ( -27.24356964375000345, 195.7531250006145456, 0.000000000000000000 ) ) ;
#33587 = CARTESIAN_POINT ( 'NONE',  ( 18.00000000000000355, -5.196152422706632912, -5.775000000000002132 ) ) ;
#33588 = CARTESIAN_POINT ( 'NONE',  ( -27.24356964375000345, 198.0593750006145513, 0.000000000000000000 ) ) ;
#33589 = EDGE_CURVE ( 'NONE', #22836, #24000, #32081, .T. ) ;
#33590 = CARTESIAN_POINT ( 'NONE',  ( 12.48663586349064403, 194.9999999999999716, 24.21355016816918493 ) ) ;
#33591 = DIRECTION ( 'NONE',  ( 0.000000000000000000, 0.000000000000000000, 1.000000000000000000 ) ) ;
#33592 = CARTESIAN_POINT ( 'NONE',  ( 8.710071997420211432, 56.51481371789856212, -3.796722387233181895 ) ) ;
#33593 = CARTESIAN_POINT ( 'NONE',  ( 18.00000000000000355, -5.196152422706632912, -9.374999999999994671 ) ) ;
#33594 = ORIENTED_EDGE ( 'NONE', *, *, #10257, .F. ) ;
#33595 = CARTESIAN_POINT ( 'NONE',  ( 26.99999999999999645, 241.2437500012290457, 3.464101615137751278 ) ) ;
#33596 = CARTESIAN_POINT ( 'NONE',  ( -2.311890736173447980, 68.87731371789855928, 12.53471296425189330 ) ) ;
#33597 = CARTESIAN_POINT ( 'NONE',  ( 13.44051670066911441, -5.407089921784865361, -6.871874999385546801 ) ) ;
#33598 = CARTESIAN_POINT ( 'NONE',  ( 27.24356964375000345, 198.2281250006145399, -3.336375036156643733E-15 ) ) ;
#33599 = CARTESIAN_POINT ( 'NONE',  ( 26.75643035624999655, 3.323476615752271712, -6.740624999385494753 ) ) ;
#33600 = CARTESIAN_POINT ( 'NONE',  ( 8.962234695871567070, 21.43981371789854862, 8.715434833792127023 ) ) ;
#33601 = EDGE_CURVE ( 'NONE', #12755, #15590, #14713, .T. ) ;
#33602 = VERTEX_POINT ( 'NONE', #35105 ) ;
#33603 = CARTESIAN_POINT ( 'NONE',  ( 36.99463137071579411, 7.347880794884117764E-16, 163.9771936566585566 ) ) ;
#33604 = CARTESIAN_POINT ( 'NONE',  ( 12.53471296425194836, 7.822686282101448896, -2.311890736173178418 ) ) ;
#33605 = VECTOR ( 'NONE', #12844, 1000.000000000000000 ) ;
#33606 = CARTESIAN_POINT ( 'NONE',  ( 28.25972136701633630, -5.407089921784865361, 168.7974587893581315 ) ) ;
#33607 = CIRCLE ( 'NONE', #19098, 7.500000000000000000 ) ;
#33608 = CARTESIAN_POINT ( 'NONE',  ( -49.20461230271183695, 208.1428034533959135, -6.469044688360754414 ) ) ;
#33609 = FACE_OUTER_BOUND ( 'NONE', #505, .T. ) ;
#33610 = CARTESIAN_POINT ( 'NONE',  ( 6.932735513424201024, 74.05231371789855643, -10.69584247140429412 ) ) ;
#33611 = CARTESIAN_POINT ( 'NONE',  ( -33.97247103062156270, 207.6499508600178387, 3.839350919129076445 ) ) ;
#33612 = CARTESIAN_POINT ( 'NONE',  ( -58.11830436395490551, 209.8844732041982581, 6.500000000000000888 ) ) ;
#33613 = CARTESIAN_POINT ( 'NONE',  ( 19.56230152254410370, 5.196152422706631135, -1.837499998771002785 ) ) ;
#33614 = CARTESIAN_POINT ( 'NONE',  ( -8.147294799025798895, 219.8188806670532358, -2.997157372947703458 ) ) ;
#33615 = CARTESIAN_POINT ( 'NONE',  ( 6.092822981423662299, 31.21481371789855430, 14.25334919248795096 ) ) ;
#33616 = CARTESIAN_POINT ( 'NONE',  ( -41.68377896937850124, 207.8379586601372750, 8.530955311639258909 ) ) ;
#33617 = CARTESIAN_POINT ( 'NONE',  ( 20.99999999999997868, 216.0000000000000000, 7.347880794884120722E-16 ) ) ;
#33618 = CARTESIAN_POINT ( 'NONE',  ( 2.311890736173175753, 74.52268628210146062, 12.53471296425194836 ) ) ;
#33619 = CARTESIAN_POINT ( 'NONE',  ( 6.092822981423978490, 15.58518628210145351, -14.25334919248782306 ) ) ;
#33620 = CARTESIAN_POINT ( 'NONE',  ( 19.56230152254412147, 5.196152422706637353, -1.500000000000029088 ) ) ;
#33621 = CARTESIAN_POINT ( 'NONE',  ( -28.92641906063026269, 202.2706296558042993, -2.079858847736485661 ) ) ;
#33622 = EDGE_LOOP ( 'NONE', ( #3945, #26729, #14474, #36370, #14483 ) ) ;
#33623 = CARTESIAN_POINT ( 'NONE',  ( 5.770363421893814682, 37.43518628210144072, 14.38691631536207183 ) ) ;
#33624 = AXIS2_PLACEMENT_3D ( 'NONE', #11670, #11490, #28728 ) ;
#33625 = CARTESIAN_POINT ( 'NONE',  ( -1.926257025242585782E-15, 195.1906250006145456, -31.45816453501076637 ) ) ;
#33626 = CARTESIAN_POINT ( 'NONE',  ( -27.24356964375000345, 198.9593750006145285, 0.000000000000000000 ) ) ;
#33627 = CARTESIAN_POINT ( 'NONE',  ( 26.99999999999999645, 247.4875000000000682, 3.464101615137751278 ) ) ;
#33628 = PRESENTATION_STYLE_ASSIGNMENT (( #4810 ) ) ;
#33629 = CARTESIAN_POINT ( 'NONE',  ( -1.045839947578415010E-13, 195.1625000000000512, 27.00000000000000355 ) ) ;
#33630 = CARTESIAN_POINT ( 'NONE',  ( -12.46528703574805697, 3.797686282101447652, -2.660918448318280838 ) ) ;
#33631 = VECTOR ( 'NONE', #3101, 1000.000000000000000 ) ;
#33632 = CARTESIAN_POINT ( 'NONE',  ( 18.12178482187500350, 246.7843750006145456, 4.985214923628407568 ) ) ;
#33633 = CARTESIAN_POINT ( 'NONE',  ( -9.500000000000005329, 116.8898137178985621, 0.1745138560723101806 ) ) ;
#33634 = CARTESIAN_POINT ( 'NONE',  ( 18.12178482187500350, 243.1843750006145513, 4.985214923628407568 ) ) ;
#33635 = VERTEX_POINT ( 'NONE', #14842 ) ;
#33636 = CARTESIAN_POINT ( 'NONE',  ( 15.00000000000000178, 249.1937500012290627, 3.464101615137757051 ) ) ;
#33637 = CARTESIAN_POINT ( 'NONE',  ( -11.48171059495408208, 134.7148137178985507, 4.944772684328421875 ) ) ;
#33638 = CARTESIAN_POINT ( 'NONE',  ( 16.56230152254411081, -7.209453229046475009, -8.128124999385510918 ) ) ;
#33639 = CARTESIAN_POINT ( 'NONE',  ( 37.25770128558855987, 3.604726614523238837, 164.1894482951998100 ) ) ;
#33640 = CARTESIAN_POINT ( 'NONE',  ( 15.24356964374999990, 3.323476615752268604, -0.2906249993854697622 ) ) ;
#33641 = CARTESIAN_POINT ( 'NONE',  ( -27.00000000000000355, 198.2000000000000171, 0.000000000000000000 ) ) ;
#33642 = ORIENTED_EDGE ( 'NONE', *, *, #6896, .T. ) ;
#33643 = CARTESIAN_POINT ( 'NONE',  ( -0.1745138560725500443, 28.81018628210144072, 12.50000000000000355 ) ) ;
#33644 = VERTEX_POINT ( 'NONE', #5545 ) ;
#33645 = EDGE_LOOP ( 'NONE', ( #26499, #3097, #13182, #15898, #17667, #20111, #33324, #34296, #5175, #33179, #31815, #31379, #36245, #23193, #4571, #23810, #4454, #5839, #14893, #19536, #13303, #35961, #33406, #29484, #37073, #30793 ) ) ;
#33646 = CARTESIAN_POINT ( 'NONE',  ( 23.99999999999999645, 5.196152422706631135, -5.493749998770947052 ) ) ;
#33647 = CARTESIAN_POINT ( 'NONE',  ( 15.24356964374999990, 0.000000000000000000, -0.5906249993854750802 ) ) ;
#33648 = DIRECTION ( 'NONE',  ( -0.000000000000000000, -1.000000000000000000, -0.000000000000000000 ) ) ;
#33649 = CARTESIAN_POINT ( 'NONE',  ( 23.87821517812499650, 249.5968750006145171, -4.985214923628404904 ) ) ;
#33650 = CARTESIAN_POINT ( 'NONE',  ( -10.49813415415989581, 68.77268628210146062, -7.228626920339068285 ) ) ;
#33651 = CARTESIAN_POINT ( 'NONE',  ( 13.23911966647218996, 136.0476862821014379, -8.632099005475504683 ) ) ;
#33652 = CARTESIAN_POINT ( 'NONE',  ( -63.05877896937850124, 211.6261429550004891, -6.530955311639245586 ) ) ;
#33653 = CARTESIAN_POINT ( 'NONE',  ( 15.04813726045348155, 225.8716339721264319, -0.7835069059937238567 ) ) ;
#33654 = CARTESIAN_POINT ( 'NONE',  ( -53.75669563604516554, 209.8844732041982297, -4.499999999999996447 ) ) ;
#33655 = CARTESIAN_POINT ( 'NONE',  ( 26.99999999999999645, 197.1125000000000114, -15.58845726811990495 ) ) ;
#33656 = CARTESIAN_POINT ( 'NONE',  ( 25.05663669538002836, 3.464101615137752166, 165.2098490755225555 ) ) ;
#33657 = CARTESIAN_POINT ( 'NONE',  ( -4.622313124798826500, 115.1648137178985678, 11.61527771782809637 ) ) ;
#33658 = CARTESIAN_POINT ( 'NONE',  ( -35.15997103062156270, 215.5714017266979852, 3.350049139982118618 ) ) ;
#33659 = CARTESIAN_POINT ( 'NONE',  ( -60.69122103062156981, 207.8379586601371329, -8.530955311639223382 ) ) ;
#33660 = CARTESIAN_POINT ( 'NONE',  ( 20.99999999999999645, -6.646953231504538984, -2.390624999385460914 ) ) ;
#33661 = CARTESIAN_POINT ( 'NONE',  ( 27.24356964375000345, 195.0781250006145342, -3.336375036156643733E-15 ) ) ;
#33662 = CARTESIAN_POINT ( 'NONE',  ( 6.092822981423662299, 95.61481371789857064, 14.25334919248795096 ) ) ;
#33663 = CARTESIAN_POINT ( 'NONE',  ( -49.79836230271183695, 204.3130714775002446, -3.149950860017828091 ) ) ;
#33664 = ORIENTED_EDGE ( 'NONE', *, *, #21920, .F. ) ;
#33665 = CARTESIAN_POINT ( 'NONE',  ( 36.72009078106068358, 7.347880794884117764E-16, 160.8391803576695622 ) ) ;
#33666 = CARTESIAN_POINT ( 'NONE',  ( 11.61527771782819940, 117.9351862821014549, -4.622313124798573369 ) ) ;
#33667 = EDGE_CURVE ( 'NONE', #34407, #1229, #26498, .T. ) ;
#33668 = CARTESIAN_POINT ( 'NONE',  ( -15.50000000000000533, 67.91018628210144925, -0.1745138560725808530 ) ) ;
#33669 = CARTESIAN_POINT ( 'NONE',  ( 18.65685424949248628, 4.000000000000095035, 50.10230395283967653 ) ) ;
#33670 = CARTESIAN_POINT ( 'NONE',  ( 34.13308826586474254, -5.407089921784861808, 164.2934219147456929 ) ) ;
#33671 = CARTESIAN_POINT ( 'NONE',  ( -6.092822981423970496, 93.78518628210144925, 14.25334919248782661 ) ) ;
#33672 = CARTESIAN_POINT ( 'NONE',  ( -50.00372103062156981, 216.5309553116392181, -1.626142955000564383 ) ) ;
#33673 = CARTESIAN_POINT ( 'NONE',  ( 13.44051670066911619, -5.407089921784859143, -7.265624999385544847 ) ) ;
#33674 = CARTESIAN_POINT ( 'NONE',  ( 2.064181346179272847, 33.69768628210143646, -9.465287035748065847 ) ) ;
#33675 = CARTESIAN_POINT ( 'NONE',  ( 15.00000000000000178, 246.4375000000000000, 3.464101615137757051 ) ) ;
#33676 = CARTESIAN_POINT ( 'NONE',  ( -63.65997103062156981, 215.5714017266979852, 3.350049139982118618 ) ) ;
#33677 = DIRECTION ( 'NONE',  ( -0.000000000000000000, -0.000000000000000000, 1.000000000000000000 ) ) ;
#33678 = CARTESIAN_POINT ( 'NONE',  ( -11.61527771782819940, 48.93518628210144783, 4.622313124798574258 ) ) ;
#33679 = DIRECTION ( 'NONE',  ( 0.000000000000000000, 0.000000000000000000, 1.000000000000000000 ) ) ;
#33680 = CYLINDRICAL_SURFACE ( 'NONE', #8714, 2.649999999999992806 ) ;
#33682 = CARTESIAN_POINT ( 'NONE',  ( 19.68408634441911431, -5.407089921784861808, -0.4968749993855270386 ) ) ;
#33681 = CARTESIAN_POINT ( 'NONE',  ( 6.594114490232313663, 27.66018628210143859, 6.840914352312096547 ) ) ;
#33683 = CARTESIAN_POINT ( 'NONE',  ( 18.00000000000000355, 241.9749999999999943, 5.196152422706632912 ) ) ;
#33684 = ORIENTED_EDGE ( 'NONE', *, *, #33807, .T. ) ;
#33685 = CARTESIAN_POINT ( 'NONE',  ( 21.00000000000000000, -6.928203230275506996, -1.237499999999996270 ) ) ;
#33686 = CARTESIAN_POINT ( 'NONE',  ( 34.05464809739185483, -5.407089921784861808, 163.3968466864631068 ) ) ;
#33687 = CARTESIAN_POINT ( 'NONE',  ( 30.78214267663955184, 6.928203230275514990, 161.8104024270723755 ) ) ;
#33688 = CARTESIAN_POINT ( 'NONE',  ( 26.99999999999999645, 243.4375000000000000, 3.464101615137751278 ) ) ;
#33689 = DIRECTION ( 'NONE',  ( -0.000000000000000000, -1.000000000000000000, -0.000000000000000000 ) ) ;
#33690 = ADVANCED_FACE ( 'NONE', ( #22999, #34548 ), #20158, .T. ) ;
#33691 = VECTOR ( 'NONE', #12375, 1000.000000000000000 ) ;
#33692 = CARTESIAN_POINT ( 'NONE',  ( 12.53471296425189330, 84.97731371789855359, 2.311890736173451977 ) ) ;
#33693 = CARTESIAN_POINT ( 'NONE',  ( -12.53471296425194659, 86.02268628210146062, 2.311890736173176641 ) ) ;
#33694 = ORIENTED_EDGE ( 'NONE', *, *, #2642, .T. ) ;
#33695 = ORIENTED_EDGE ( 'NONE', *, *, #18060, .T. ) ;
#33696 = CARTESIAN_POINT ( 'NONE',  ( 26.99999999999999645, 199.0250000012290457, -15.58845726811990495 ) ) ;
#33697 = CYLINDRICAL_SURFACE ( 'NONE', #11406, 5.999999999999999112 ) ;
#33698 = CARTESIAN_POINT ( 'NONE',  ( -15.46528703574811736, 61.40231371789855785, 3.257655550456946436 ) ) ;
#33699 = CARTESIAN_POINT ( 'NONE',  ( 18.12178482187500350, -4.985214923628407568, -8.728124999385494576 ) ) ;
#33700 = EDGE_CURVE ( 'NONE', #26085, #16407, #34305, .T. ) ;
#33701 = CARTESIAN_POINT ( 'NONE',  ( 26.75643035624999655, 242.8468750006145456, 3.323476615752267715 ) ) ;
#33702 = CARTESIAN_POINT ( 'NONE',  ( -57.12872103062156270, 205.4690446883607535, 1.090244570138264368 ) ) ;
#33703 = CARTESIAN_POINT ( 'NONE',  ( -5.233372021372612259, 41.85231371789854649, 8.152565276336593669 ) ) ;
#33704 = CARTESIAN_POINT ( 'NONE',  ( 13.44051670066911086, 5.407089921784856479, -7.415624999385555860 ) ) ;
#33705 = CARTESIAN_POINT ( 'NONE',  ( 8.710071997420211432, 93.31481371789855928, -3.796722387233181895 ) ) ;
#33706 = CARTESIAN_POINT ( 'NONE',  ( 13.62178482187499640, 198.3593750006145342, -23.59362340125807123 ) ) ;
#33707 = CARTESIAN_POINT ( 'NONE',  ( -4.944772684328424539, 8.214813717898532985, -11.48171059495408031 ) ) ;
#33708 = CARTESIAN_POINT ( 'NONE',  ( -2.660918448318275509, 56.69768628210145067, 12.46528703574805874 ) ) ;
#33709 = CARTESIAN_POINT ( 'NONE',  ( 22.56230152254411436, -3.464101615137751278, -9.149999998771001231 ) ) ;
#33710 = CARTESIAN_POINT ( 'NONE',  ( 31.05668326629465170, 6.928203230275514990, 164.9484157260613699 ) ) ;
#33711 = CARTESIAN_POINT ( 'NONE',  ( 33.82423010250274586, -5.407089921784855591, 160.7631569533830600 ) ) ;
#33712 = CARTESIAN_POINT ( 'NONE',  ( 19.68408634441910721, 5.407089921784862696, -9.796874999385529748 ) ) ;
#33713 = CARTESIAN_POINT ( 'NONE',  ( 10.31873187879410736, 0.000000000000000000, -7.396874999385516958 ) ) ;
#33714 = VECTOR ( 'NONE', #3687, 1000.000000000000000 ) ;
#33715 = CARTESIAN_POINT ( 'NONE',  ( 36.58935716683290451, -3.464101615137295642, 159.3448883093075779 ) ) ;
#33716 = EDGE_CURVE ( 'NONE', #4030, #22836, #24503, .T. ) ;
#33717 = CARTESIAN_POINT ( 'NONE',  ( 15.02283181144952628, 7.347880794884122694E-16, 50.52293445648592751 ) ) ;
#33718 = CARTESIAN_POINT ( 'NONE',  ( -9.465287035748065847, 95.79768628210145209, -2.064181346179273735 ) ) ;
#33719 = CARTESIAN_POINT ( 'NONE',  ( 0.000000000000000000, 148.0000000000000000, -5.000000000000000888 ) ) ;
#33720 = CARTESIAN_POINT ( 'NONE',  ( -4.944772684328673229, 112.1851862821014549, 11.48171059495397728 ) ) ;
#33721 = CARTESIAN_POINT ( 'NONE',  ( 10.56230152254349086, 3.464101615137404888, -3.187499999999991562 ) ) ;
#33722 = DIRECTION ( 'NONE',  ( 1.000000000000000000, 0.000000000000000000, 0.000000000000000000 ) ) ;
#33723 = VERTEX_POINT ( 'NONE', #29995 ) ;
#33724 = CARTESIAN_POINT ( 'NONE',  ( 24.79520095057666396, 0.000000000000000000, 165.0162730863461604 ) ) ;
#33725 = CARTESIAN_POINT ( 'NONE',  ( 23.87821517812500005, -4.985214923628404016, -4.940624999385468286 ) ) ;
#33726 = CIRCLE ( 'NONE', #30705, 5.999999999999999112 ) ;
#33728 = EDGE_CURVE ( 'NONE', #17309, #14417, #7149, .T. ) ;
#33727 = CARTESIAN_POINT ( 'NONE',  ( -27.24356964374999279, 197.6468750006145285, 15.72908226750539384 ) ) ;
#33729 = CARTESIAN_POINT ( 'NONE',  ( 34.53836246964132073, 5.407089921784862696, 168.9257272608723213 ) ) ;
#33730 = CARTESIAN_POINT ( 'NONE',  ( 25.32790894457497899, -3.464101615137761048, 168.3105050721087821 ) ) ;
#33731 = DIRECTION ( 'NONE',  ( -0.000000000000000000, -0.000000000000000000, 1.000000000000000000 ) ) ;
#33732 = CARTESIAN_POINT ( 'NONE',  ( 15.24356964374999990, 242.1718750006145342, -3.323476615752268604 ) ) ;
#33733 = PLANE ( 'NONE',  #11193 ) ;
#33734 = CARTESIAN_POINT ( 'NONE',  ( 12.46528703574811558, 139.6023137178985394, -2.660918448318005503 ) ) ;
#33735 = CARTESIAN_POINT ( 'NONE',  ( -1.926257025242585782E-15, 195.6968750006145683, -31.45816453501076637 ) ) ;
#33737 = ORIENTED_EDGE ( 'NONE', *, *, #35976, .F. ) ;
#33736 = ORIENTED_EDGE ( 'NONE', *, *, #32646, .F. ) ;
#33738 = CARTESIAN_POINT ( 'NONE',  ( 18.12178482187499640, 244.2718750006145001, -4.985214923628404904 ) ) ;
#33739 = EDGE_CURVE ( 'NONE', #10799, #10052, #36951, .T. ) ;
#33740 = DIRECTION ( 'NONE',  ( -0.000000000000000000, -1.000000000000000000, -0.000000000000000000 ) ) ;
#33741 = CARTESIAN_POINT ( 'NONE',  ( 26.75643035624999655, -3.323476615752267715, -3.103124999385467486 ) ) ;
#33742 = CARTESIAN_POINT ( 'NONE',  ( -3.257655550456946880, 118.9023137178985650, -15.46528703574811736 ) ) ;
#33743 =( BOUNDED_SURFACE ( )  B_SPLINE_SURFACE ( 1, 2, ( 
 ( #6268, #24276, #32794, #29954, #3420, #15745, #29574, #27113, #12704, #9861, #18602, #32982, #11952, #9117, #17845, #14988, #26538, #568, #12135, #19860, #2029, #27485, #28365, #13606, #19678, #11124, #37263, #15937, #5246, #33875, #31037, #28182, #5059, #25156, #21624, #25710, #8104, #16823, #22323, #16641, #19491, #24460, #31582, #28544, #7219, #34429, #8287, #36009, #36711, #31217, #33175, #2213, #13795, #7917, #10048, #25342, #18791, #13975, #36891, #22511, #10937, #10750, #37078, #5422, #34058, #31403, #2400, #25525, #11310, #22701, #34245, #17003, #30332, #4356, #2586, #14156, #22878, #8466, #20036, #5605, #27296, #1327, #12896, #32505, #12233, #11858, #23061, #23427, #11492, #20409, #17376, #108, #35159, #8650, #14341, #14709, #6174, #31951, #28730, #35344, #5796, #9209, #20593, #17746, #32322, #9398, #6363, #5983, #20973, #292, #34979, #23804, #17563, #34607, #26632, #34793, #3141, #20219, #3326, #29098, #31765, #20780, #17190, #12045, #29287, #28919, #25895, #14897, #2953, #26445, #661, #478, #23615, #9021, #32134, #17934, #14523, #29478, #26257, #3515, #26079, #15082, #2768, #37443, #11672, #23247, #8837, #32886, #9584, #21898, #3890, #12612, #6936, #16028, #13175, #27016, #27199, #9953, #4079, #21347, #12425, #1041, #30428, #36099, #18313, #33080, #9769, #18124, #24730, #32696, #24548, #21534, #7123, #21715, #36280, #33266, #18506, #10328, #1225, #12797, #1606, #30045, #854, #27577, #24178, #15651, #35539, #30236, #24366, #21158, #10142, #6551, #1415, #18695, #6738, #3702, #29667, #15462, #4448, #15271, #26824, #23994, #35910, #29853, #4262, #35723, #15837, #27385, #12993, #7305, #18877, #4634, #22458, #33638, #25659, #28132, #7864, #30988, #27763, #16769, #1793, #33827, #19438, #28315, #11260, #33446, #5006, #16587, #7489, #22274, #25101, #16213, #19065, #7677, #34005, #27946, #36659, #10697, #30617, #37213, #34193, #13360, #2540, #13925, #24915, #19257, #36842, #36467, #2161, #13744, #1976, #10508, #25290, #22088, #19626, #10885, #8050, #31172, #4819, #5194, #11072, #30796, #25475, #2353, #16400, #16954, #37026, #22647, #8239, #13548, #19814 ),
 ( #28497, #31348, #14107, #5375, #28679, #29048, #17143, #26029, #23011, #5746, #3279, #14293, #19989, #20362, #22831, #6317, #616, #17889, #17514, #2717, #3092, #25846, #57, #34561, #17326, #14852, #37394, #31533, #31905, #11811, #11624, #34379, #3470, #11444, #26401, #26211, #23381, #434, #15039, #11999, #23199, #26587, #5934, #14660, #29434, #34747, #8600, #32274, #2904, #8790, #20171, #8975, #247, #31719, #23570, #8420, #17699, #34930, #28869, #5558, #14476, #20546, #20731, #32090, #6121, #29239, #35115, #9164, #996, #32463, #9910, #15421, #21494, #23949, #33224, #20924, #1184, #12379, #4405, #6886, #24139, #9733, #6506, #33035, #18081, #12572, #35681, #7084, #27536, #12186, #21305, #32841, #23758, #18462, #3844, #29622, #35297, #35491, #12758, #6695, #26967, #30004, #9353, #15988, #12948, #3657, #18838, #30193, #15228, #9541, #15605, #26778, #4033, #27161, #18266, #808, #24326, #21115, #35868, #18652, #4219, #15797, #32654, #27347, #1378, #29810, #24509, #36057, #10101, #7263, #21670, #30384, #5148, #21857, #30579, #2121, #36613, #30943, #36241, #25249, #28275, #22417, #33784, #13698, #1561, #16172, #36799, #22604, #10843, #33964, #7822, #22233, #8006, #7448, #19579, #27903, #19399, #27722, #36986, #31131, #13133, #33410, #25434, #4961, #1934, #4595, #16915, #36425, #7636, #13502, #11029, #8196, #22046, #16543, #28089, #10654, #16355, #19022, #33597, #34149, #16729, #13318, #1752, #2311, #24876, #13885, #19772, #31309, #10468, #5337, #19213, #4781, #25060, #24688, #30759, #10283, #34891, #14434, #37350, #11584, #23159, #11774, #29007, #37173, #20128, #28639, #25801, #26172, #34701, #8380, #5704, #2492, #29196, #14252, #11402, #11214, #2677, #17284, #34335, #14067, #28456, #28825, #8748, #3051, #22786, #20319, #8931, #31860, #5894, #6076, #14621, #208, #17472, #5515, #23340, #22973, #18, #20508, #32045, #17661, #3238, #34521, #25616, #8561, #19951, #31492, #31675, #17100, #2860, #25988, #25552, #2241, #25367, #2057, #10962, #10407, #33712, #5087, #13635, #37104, #36914, #33899, #28390, #25184, #10776, #19517, #36737, #27838, #22536, #31244, #2611 ) ),
 .UNSPECIFIED., .F., .F., .F. ) 
 B_SPLINE_SURFACE_WITH_KNOTS ( ( 2, 2 ),
 ( 3, 2, 2, 2, 2, 2, 2, 2, 2, 2, 2, 2, 2, 2, 2, 2, 2, 2, 2, 2, 2, 2, 2, 2, 2, 2, 2, 2, 2, 2, 2, 2, 2, 2, 2, 2, 2, 2, 2, 2, 2, 2, 2, 2, 2, 2, 2, 2, 2, 2, 2, 2, 2, 2, 2, 2, 2, 2, 2, 2, 2, 2, 2, 2, 2, 2, 2, 2, 2, 2, 2, 2, 2, 2, 2, 2, 2, 2, 2, 2, 2, 2, 2, 2, 2, 2, 2, 2, 2, 2, 2, 2, 2, 2, 2, 2, 2, 2, 2, 2, 2, 2, 2, 2, 2, 2, 2, 2, 2, 2, 2, 2, 2, 2, 2, 2, 2, 2, 2, 2, 2, 2, 2, 2, 2, 2, 2, 2, 2, 2, 2, 2, 2, 2, 2, 3 ),
 ( 0.000000000000000000, 1.000000000000000000 ),
 ( 0.000000000000000000, 0.007246376811594202987, 0.01449275362318840597, 0.02173913043478260809, 0.02898550724637681195, 0.03623188405797101580, 0.04347826086956521618, 0.05072463768115942351, 0.05797101449275362389, 0.06521739130434782428, 0.07246376811594203160, 0.07971014492753622505, 0.08695652173913043237, 0.09420289855072463969, 0.1014492753623188470, 0.1086956521739130405, 0.1159420289855072478, 0.1231884057971014551, 0.1304347826086956486, 0.1376811594202898559, 0.1449275362318840632, 0.1521739130434782705, 0.1594202898550724501, 0.1666666666666666574, 0.1739130434782608647, 0.1811594202898550721, 0.1884057971014492794, 0.1956521739130434867, 0.2028985507246376940, 0.2101449275362318736, 0.2173913043478260809, 0.2246376811594202882, 0.2318840579710144956, 0.2391304347826087029, 0.2463768115942029102, 0.2536231884057971175, 0.2608695652173912971, 0.2681159420289855322, 0.2753623188405797118, 0.2826086956521738913, 0.2898550724637681264, 0.2971014492753623060, 0.3043478260869565410, 0.3115942028985507206, 0.3188405797101449002, 0.3260869565217391353, 0.3333333333333333148, 0.3405797101449275499, 0.3478260869565217295, 0.3550724637681159646, 0.3623188405797101441, 0.3695652173913043237, 0.3768115942028985588, 0.3840579710144927383, 0.3913043478260869734, 0.3985507246376811530, 0.4057971014492753881, 0.4130434782608695676, 0.4202898550724637472, 0.4275362318840579823, 0.4347826086956521618, 0.4420289855072463969, 0.4492753623188405765, 0.4565217391304347561, 0.4637681159420289911, 0.4710144927536231707, 0.4782608695652174058, 0.4855072463768115854, 0.4927536231884058204, 0.5000000000000000000, 0.5072463768115942351, 0.5144927536231883591, 0.5217391304347825942, 0.5289855072463768293, 0.5362318840579710644, 0.5434782608695651884, 0.5507246376811594235, 0.5579710144927536586, 0.5652173913043477826, 0.5724637681159420177, 0.5797101449275362528, 0.5869565217391304879, 0.5942028985507246119, 0.6014492753623188470, 0.6086956521739130821, 0.6159420289855072062, 0.6231884057971014412, 0.6304347826086956763, 0.6376811594202898004, 0.6449275362318840354, 0.6521739130434782705, 0.6594202898550725056, 0.6666666666666666297, 0.6739130434782608647, 0.6811594202898550998, 0.6884057971014492239, 0.6956521739130434590, 0.7028985507246376940, 0.7101449275362319291, 0.7173913043478260532, 0.7246376811594202882, 0.7318840579710145233, 0.7391304347826086474, 0.7463768115942028825, 0.7536231884057971175, 0.7608695652173913526, 0.7681159420289854767, 0.7753623188405797118, 0.7826086956521739468, 0.7898550724637680709, 0.7971014492753623060, 0.8043478260869565410, 0.8115942028985507761, 0.8188405797101449002, 0.8260869565217391353, 0.8333333333333333703, 0.8405797101449274944, 0.8478260869565217295, 0.8550724637681159646, 0.8623188405797101996, 0.8695652173913043237, 0.8768115942028985588, 0.8840579710144927938, 0.8913043478260869179, 0.8985507246376811530, 0.9057971014492753881, 0.9130434782608695121, 0.9202898550724637472, 0.9275362318840579823, 0.9347826086956522174, 0.9420289855072463414, 0.9492753623188405765, 0.9565217391304348116, 0.9637681159420289356, 0.9662082893573751274, 0.9758703722509488587 ),
 .UNSPECIFIED. ) 
 GEOMETRIC_REPRESENTATION_ITEM ( )  RATIONAL_B_SPLINE_SURFACE ( (
 ( 1.000000000000000000, 0.8660254037844387076, 1.000000000000000000, 0.8660254037844387076, 1.000000000000000000, 0.8660254037844387076, 1.000000000000000000, 0.8660254037844387076, 1.000000000000000000, 0.8660254037844387076, 1.000000000000000000, 0.8660254037844387076, 1.000000000000000000, 0.8660254037844387076, 1.000000000000000000, 0.8660254037844387076, 1.000000000000000000, 0.8660254037844387076, 1.000000000000000000, 0.8660254037844387076, 1.000000000000000000, 0.8660254037844387076, 1.000000000000000000, 0.8660254037844387076, 1.000000000000000000, 0.8660254037844387076, 1.000000000000000000, 0.8660254037844387076, 1.000000000000000000, 0.8660254037844387076, 1.000000000000000000, 0.8660254037844387076, 1.000000000000000000, 0.8660254037844387076, 1.000000000000000000, 0.8660254037844387076, 1.000000000000000000, 0.8660254037844387076, 1.000000000000000000, 0.8660254037844387076, 1.000000000000000000, 0.8660254037844387076, 1.000000000000000000, 0.8660254037844387076, 1.000000000000000000, 0.8660254037844387076, 1.000000000000000000, 0.8660254037844387076, 1.000000000000000000, 0.8660254037844387076, 1.000000000000000000, 0.8660254037844387076, 1.000000000000000000, 0.8660254037844387076, 1.000000000000000000, 0.8660254037844387076, 1.000000000000000000, 0.8660254037844387076, 1.000000000000000000, 0.8660254037844387076, 1.000000000000000000, 0.8660254037844387076, 1.000000000000000000, 0.8660254037844387076, 1.000000000000000000, 0.8660254037844387076, 1.000000000000000000, 0.8660254037844387076, 1.000000000000000000, 0.8660254037844387076, 1.000000000000000000, 0.8660254037844387076, 1.000000000000000000, 0.8660254037844387076, 1.000000000000000000, 0.8660254037844387076, 1.000000000000000000, 0.8660254037844387076, 1.000000000000000000, 0.8660254037844387076, 1.000000000000000000, 0.8660254037844387076, 1.000000000000000000, 0.8660254037844387076, 1.000000000000000000, 0.8660254037844387076, 1.000000000000000000, 0.8660254037844387076, 1.000000000000000000, 0.8660254037844387076, 1.000000000000000000, 0.8660254037844387076, 1.000000000000000000, 0.8660254037844387076, 1.000000000000000000, 0.8660254037844387076, 1.000000000000000000, 0.8660254037844387076, 1.000000000000000000, 0.8660254037844387076, 1.000000000000000000, 0.8660254037844387076, 1.000000000000000000, 0.8660254037844387076, 1.000000000000000000, 0.8660254037844387076, 1.000000000000000000, 0.8660254037844387076, 1.000000000000000000, 0.8660254037844387076, 1.000000000000000000, 0.8660254037844387076, 1.000000000000000000, 0.8660254037844387076, 1.000000000000000000, 0.8660254037844387076, 1.000000000000000000, 0.8660254037844387076, 1.000000000000000000, 0.8660254037844387076, 1.000000000000000000, 0.8660254037844387076, 1.000000000000000000, 0.8660254037844387076, 1.000000000000000000, 0.8660254037844387076, 1.000000000000000000, 0.8660254037844387076, 1.000000000000000000, 0.8660254037844387076, 1.000000000000000000, 0.8660254037844387076, 1.000000000000000000, 0.8660254037844387076, 1.000000000000000000, 0.8660254037844387076, 1.000000000000000000, 0.8660254037844387076, 1.000000000000000000, 0.8660254037844387076, 1.000000000000000000, 0.8660254037844387076, 1.000000000000000000, 0.8660254037844387076, 1.000000000000000000, 0.8660254037844387076, 1.000000000000000000, 0.8660254037844387076, 1.000000000000000000, 0.8660254037844387076, 1.000000000000000000, 0.8660254037844387076, 1.000000000000000000, 0.8660254037844387076, 1.000000000000000000, 0.8660254037844387076, 1.000000000000000000, 0.8660254037844387076, 1.000000000000000000, 0.8660254037844387076, 1.000000000000000000, 0.8660254037844387076, 1.000000000000000000, 0.8660254037844387076, 1.000000000000000000, 0.8660254037844387076, 1.000000000000000000, 0.8660254037844387076, 1.000000000000000000, 0.8660254037844387076, 1.000000000000000000, 0.8660254037844387076, 1.000000000000000000, 0.8660254037844387076, 1.000000000000000000, 0.8660254037844387076, 1.000000000000000000, 0.8660254037844387076, 1.000000000000000000, 0.8660254037844387076, 1.000000000000000000, 0.8660254037844387076, 1.000000000000000000, 0.8660254037844387076, 1.000000000000000000, 0.8660254037844387076, 1.000000000000000000, 0.8660254037844387076, 1.000000000000000000, 0.8660254037844387076, 1.000000000000000000, 0.8660254037844387076, 1.000000000000000000, 0.8660254037844387076, 1.000000000000000000, 0.8660254037844387076, 1.000000000000000000, 0.8660254037844387076, 1.000000000000000000, 0.8660254037844387076, 1.000000000000000000, 0.8660254037844387076, 1.000000000000000000, 0.8660254037844387076, 1.000000000000000000, 0.8660254037844387076, 1.000000000000000000, 0.8660254037844387076, 1.000000000000000000, 0.8660254037844387076, 1.000000000000000000, 0.8660254037844387076, 1.000000000000000000, 0.8660254037844387076, 1.000000000000000000, 0.8660254037844387076, 1.000000000000000000, 0.8660254037844387076, 1.000000000000000000, 0.8660254037844387076, 1.000000000000000000, 0.8660254037844387076, 1.000000000000000000, 0.8660254037844387076, 1.000000000000000000, 0.8660254037844387076, 1.000000000000000000, 0.8660254037844387076, 1.000000000000000000, 0.8660254037844387076, 1.000000000000000000, 0.8660254037844387076, 1.000000000000000000, 0.8660254037844387076, 1.000000000000000000, 0.8660254037844387076, 1.000000000000000000, 0.8660254037844387076, 1.000000000000000000, 0.8660254037844387076, 1.000000000000000000, 0.8660254037844387076, 1.000000000000000000, 0.8660254037844387076, 1.000000000000000000, 0.8660254037844387076, 1.000000000000000000, 0.8660254037844387076, 1.000000000000000000, 0.8660254037844387076, 1.000000000000000000, 0.8660254037844387076, 1.000000000000000000, 0.8660254037844387076, 1.000000000000000000, 0.8660254037844387076, 1.000000000000000000, 0.8660254037844387076, 1.000000000000000000, 0.8660254037844387076, 1.000000000000000000, 0.8660254037844387076, 1.000000000000000000, 0.8660254037844387076, 1.000000000000000000, 0.8660254037844387076, 1.000000000000000000, 0.9548848677736607726, 0.9401542295229587953, 0.9401542295229587953, 0.9401542295229587953),
 ( 1.000000000000000000, 0.8660254037844387076, 1.000000000000000000, 0.8660254037844387076, 1.000000000000000000, 0.8660254037844387076, 1.000000000000000000, 0.8660254037844387076, 1.000000000000000000, 0.8660254037844387076, 1.000000000000000000, 0.8660254037844387076, 1.000000000000000000, 0.8660254037844387076, 1.000000000000000000, 0.8660254037844387076, 1.000000000000000000, 0.8660254037844387076, 1.000000000000000000, 0.8660254037844387076, 1.000000000000000000, 0.8660254037844387076, 1.000000000000000000, 0.8660254037844387076, 1.000000000000000000, 0.8660254037844387076, 1.000000000000000000, 0.8660254037844387076, 1.000000000000000000, 0.8660254037844387076, 1.000000000000000000, 0.8660254037844387076, 1.000000000000000000, 0.8660254037844387076, 1.000000000000000000, 0.8660254037844387076, 1.000000000000000000, 0.8660254037844387076, 1.000000000000000000, 0.8660254037844387076, 1.000000000000000000, 0.8660254037844387076, 1.000000000000000000, 0.8660254037844387076, 1.000000000000000000, 0.8660254037844387076, 1.000000000000000000, 0.8660254037844387076, 1.000000000000000000, 0.8660254037844387076, 1.000000000000000000, 0.8660254037844387076, 1.000000000000000000, 0.8660254037844387076, 1.000000000000000000, 0.8660254037844387076, 1.000000000000000000, 0.8660254037844387076, 1.000000000000000000, 0.8660254037844387076, 1.000000000000000000, 0.8660254037844387076, 1.000000000000000000, 0.8660254037844387076, 1.000000000000000000, 0.8660254037844387076, 1.000000000000000000, 0.8660254037844387076, 1.000000000000000000, 0.8660254037844387076, 1.000000000000000000, 0.8660254037844387076, 1.000000000000000000, 0.8660254037844387076, 1.000000000000000000, 0.8660254037844387076, 1.000000000000000000, 0.8660254037844387076, 1.000000000000000000, 0.8660254037844387076, 1.000000000000000000, 0.8660254037844387076, 1.000000000000000000, 0.8660254037844387076, 1.000000000000000000, 0.8660254037844387076, 1.000000000000000000, 0.8660254037844387076, 1.000000000000000000, 0.8660254037844387076, 1.000000000000000000, 0.8660254037844387076, 1.000000000000000000, 0.8660254037844387076, 1.000000000000000000, 0.8660254037844387076, 1.000000000000000000, 0.8660254037844387076, 1.000000000000000000, 0.8660254037844387076, 1.000000000000000000, 0.8660254037844387076, 1.000000000000000000, 0.8660254037844387076, 1.000000000000000000, 0.8660254037844387076, 1.000000000000000000, 0.8660254037844387076, 1.000000000000000000, 0.8660254037844387076, 1.000000000000000000, 0.8660254037844387076, 1.000000000000000000, 0.8660254037844387076, 1.000000000000000000, 0.8660254037844387076, 1.000000000000000000, 0.8660254037844387076, 1.000000000000000000, 0.8660254037844387076, 1.000000000000000000, 0.8660254037844387076, 1.000000000000000000, 0.8660254037844387076, 1.000000000000000000, 0.8660254037844387076, 1.000000000000000000, 0.8660254037844387076, 1.000000000000000000, 0.8660254037844387076, 1.000000000000000000, 0.8660254037844387076, 1.000000000000000000, 0.8660254037844387076, 1.000000000000000000, 0.8660254037844387076, 1.000000000000000000, 0.8660254037844387076, 1.000000000000000000, 0.8660254037844387076, 1.000000000000000000, 0.8660254037844387076, 1.000000000000000000, 0.8660254037844387076, 1.000000000000000000, 0.8660254037844387076, 1.000000000000000000, 0.8660254037844387076, 1.000000000000000000, 0.8660254037844387076, 1.000000000000000000, 0.8660254037844387076, 1.000000000000000000, 0.8660254037844387076, 1.000000000000000000, 0.8660254037844387076, 1.000000000000000000, 0.8660254037844387076, 1.000000000000000000, 0.8660254037844387076, 1.000000000000000000, 0.8660254037844387076, 1.000000000000000000, 0.8660254037844387076, 1.000000000000000000, 0.8660254037844387076, 1.000000000000000000, 0.8660254037844387076, 1.000000000000000000, 0.8660254037844387076, 1.000000000000000000, 0.8660254037844387076, 1.000000000000000000, 0.8660254037844387076, 1.000000000000000000, 0.8660254037844387076, 1.000000000000000000, 0.8660254037844387076, 1.000000000000000000, 0.8660254037844387076, 1.000000000000000000, 0.8660254037844387076, 1.000000000000000000, 0.8660254037844387076, 1.000000000000000000, 0.8660254037844387076, 1.000000000000000000, 0.8660254037844387076, 1.000000000000000000, 0.8660254037844387076, 1.000000000000000000, 0.8660254037844387076, 1.000000000000000000, 0.8660254037844387076, 1.000000000000000000, 0.8660254037844387076, 1.000000000000000000, 0.8660254037844387076, 1.000000000000000000, 0.8660254037844387076, 1.000000000000000000, 0.8660254037844387076, 1.000000000000000000, 0.8660254037844387076, 1.000000000000000000, 0.8660254037844387076, 1.000000000000000000, 0.8660254037844387076, 1.000000000000000000, 0.8660254037844387076, 1.000000000000000000, 0.8660254037844387076, 1.000000000000000000, 0.8660254037844387076, 1.000000000000000000, 0.8660254037844387076, 1.000000000000000000, 0.8660254037844387076, 1.000000000000000000, 0.8660254037844387076, 1.000000000000000000, 0.8660254037844387076, 1.000000000000000000, 0.8660254037844387076, 1.000000000000000000, 0.8660254037844387076, 1.000000000000000000, 0.8660254037844387076, 1.000000000000000000, 0.8660254037844387076, 1.000000000000000000, 0.8660254037844387076, 1.000000000000000000, 0.8660254037844387076, 1.000000000000000000, 0.8660254037844387076, 1.000000000000000000, 0.8660254037844387076, 1.000000000000000000, 0.8660254037844387076, 1.000000000000000000, 0.8660254037844387076, 1.000000000000000000, 0.8660254037844387076, 1.000000000000000000, 0.8660254037844387076, 1.000000000000000000, 0.8660254037844387076, 1.000000000000000000, 0.8660254037844387076, 1.000000000000000000, 0.8660254037844387076, 1.000000000000000000, 0.8660254037844387076, 1.000000000000000000, 0.8660254037844387076, 1.000000000000000000, 0.8660254037844387076, 1.000000000000000000, 0.8660254037844387076, 1.000000000000000000, 0.8660254037844387076, 1.000000000000000000, 0.8660254037844387076, 1.000000000000000000, 0.8660254037844387076, 1.000000000000000000, 0.9548848677736607726, 0.9401542295229587953, 0.9401542295229587953, 0.9401542295229587953) ) ) 
 REPRESENTATION_ITEM ( '' )  SURFACE ( )  );
#33744 = CARTESIAN_POINT ( 'NONE',  ( 21.00000000000000000, 244.2624999999999886, 5.999999999999998224 ) ) ;
#33745 = CARTESIAN_POINT ( 'NONE',  ( 18.12178482187499640, 4.985214923628404904, -1.678124999385494087 ) ) ;
#33746 = CARTESIAN_POINT ( 'NONE',  ( 19.68408634441911786, -5.407089921784861808, -9.046874999385529748 ) ) ;
#33747 = ORIENTED_EDGE ( 'NONE', *, *, #37101, .T. ) ;
#33748 = CARTESIAN_POINT ( 'NONE',  ( -27.24356964374999635, 194.8906250006145342, 15.72908226750539384 ) ) ;
#33749 = CARTESIAN_POINT ( 'NONE',  ( -12.53471296425194836, 113.6226862821014407, 2.311890736173176641 ) ) ;
#33750 = CARTESIAN_POINT ( 'NONE',  ( 22.80587116629410360, -3.604726614523235284, -0.4031249993855248182 ) ) ;
#33751 = ADVANCED_FACE ( 'NONE', ( #35861 ), #23940, .T. ) ;
#33752 = CARTESIAN_POINT ( 'NONE',  ( -42.87127896937849414, 218.5309553116392465, 2.162041339862725842 ) ) ;
#33753 = CARTESIAN_POINT ( 'NONE',  ( 15.24356964374999990, 245.2093750006145285, -3.323476615752268604 ) ) ;
#33754 = CARTESIAN_POINT ( 'NONE',  ( -7.234628195640328663, 197.5049038117967086, 26.99999999999999289 ) ) ;
#33755 = CARTESIAN_POINT ( 'NONE',  ( -34.55877896937850124, 211.0902445701383101, -4.530955311639234040 ) ) ;
#33756 = CARTESIAN_POINT ( 'NONE',  ( 8.715434833791931624, 110.4601862821014606, 8.962234695871760692 ) ) ;
#33757 = CARTESIAN_POINT ( 'NONE',  ( 10.56230152254411259, -3.464101615137757051, -1.199999998771033916 ) ) ;
#33758 = ORIENTED_EDGE ( 'NONE', *, *, #3459, .T. ) ;
#33759 =( BOUNDED_CURVE ( )  B_SPLINE_CURVE ( 2, ( #36745, #25745, #19714, #16486, #20073, #25193, #31072, #8142, #5280 ),
 .UNSPECIFIED., .F., .F. ) 
 B_SPLINE_CURVE_WITH_KNOTS ( ( 3, 2, 2, 2, 3 ),
 ( 0.8804347826086956763, 0.8840579710144927938, 0.8913043478260869179, 0.8985507246376811530, 0.9021739130434782705 ),
 .UNSPECIFIED. ) 
 CURVE ( )  GEOMETRIC_REPRESENTATION_ITEM ( )  RATIONAL_B_SPLINE_CURVE ( ( 0.9330127018922194093, 0.9330127018922194093, 1.000000000000000000, 0.8660254037844387076, 1.000000000000000000, 0.8660254037844387076, 1.000000000000000000, 0.9330127018922194093, 0.9330127018922194093 ) ) 
 REPRESENTATION_ITEM ( '' )  );
#33760 = CARTESIAN_POINT ( 'NONE',  ( -47.03497103062156981, 204.4285982733020148, -3.350049139982115509 ) ) ;
#33761 = FACE_OUTER_BOUND ( 'NONE', #30948, .T. ) ;
#33762 = CARTESIAN_POINT ( 'NONE',  ( 15.50000000000000533, 118.5101862821014720, 0.1745138560725827404 ) ) ;
#33763 = UNCERTAINTY_MEASURE_WITH_UNIT (LENGTH_MEASURE( 1.000000000000000082E-05 ), #28256, 'distance_accuracy_value', 'NONE');
#33764 = ADVANCED_FACE ( 'NONE', ( #4399 ), #12751, .T. ) ;
#33765 = CARTESIAN_POINT ( 'NONE',  ( 26.99999999999999645, 242.6312500012290343, -7.347880794884117764E-16 ) ) ;
#33766 = CARTESIAN_POINT ( 'NONE',  ( -12.50000000000000355, 3.510186282101451560, -0.1745138560725492671 ) ) ;
#33767 = CARTESIAN_POINT ( 'NONE',  ( 13.56230152254410726, 5.196152422706636465, -8.625000000000021316 ) ) ;
#33768 = ORIENTED_EDGE ( 'NONE', *, *, #20856, .T. ) ;
#33769 = CARTESIAN_POINT ( 'NONE',  ( -12.50000000000000355, 3.510186282101451560, -0.1745138560725492671 ) ) ;
#33770 = CARTESIAN_POINT ( 'NONE',  ( -3.474262827703337830, 88.03518628210144925, -8.843639120294326972 ) ) ;
#33771 = CARTESIAN_POINT ( 'NONE',  ( 20.99999999999999645, 185.0294372515228645, 0.000000000000000000 ) ) ;
#33772 = CARTESIAN_POINT ( 'NONE',  ( 9.534712964251900402, 130.9773137178985394, 1.715153634034445540 ) ) ;
#33773 = CARTESIAN_POINT ( 'NONE',  ( -27.24356964374999990, 195.7156250006145513, -15.72908226750537786 ) ) ;
#33774 = CARTESIAN_POINT ( 'NONE',  ( 19.39230484541327471, 246.9986538117966859, 6.000000000000002665 ) ) ;
#33775 = CARTESIAN_POINT ( 'NONE',  ( 13.62178482187499640, 197.9093750006145456, -23.59362340125807123 ) ) ;
#33776 = CARTESIAN_POINT ( 'NONE',  ( -11.00000000000001243, 143.0000000000000000, -1.227709706637561792E-13 ) ) ;
#33777 = CARTESIAN_POINT ( 'NONE',  ( 23.99999999999999645, 244.0000000000000000, -5.196152422706631135 ) ) ;
#33778 = CARTESIAN_POINT ( 'NONE',  ( 9.465287035748106703, 66.00231371789855928, -2.064181346179063237 ) ) ;
#33779 = CARTESIAN_POINT ( 'NONE',  ( 26.99999999999999645, 7.347880794884117764E-16, -9.674999999999990052 ) ) ;
#33780 = ORIENTED_EDGE ( 'NONE', *, *, #34020, .F. ) ;
#33781 = EDGE_CURVE ( 'NONE', #6483, #28398, #19769, .T. ) ;
#33782 = CARTESIAN_POINT ( 'NONE',  ( 26.99999999999999645, 242.5937500012290400, 3.464101615137751278 ) ) ;
#33783 = CARTESIAN_POINT ( 'NONE',  ( -2.311890736173447980, 59.67731371789855643, 12.53471296425189330 ) ) ;
#33784 = CARTESIAN_POINT ( 'NONE',  ( 13.44051670066911264, -5.407089921784865361, -5.521874999385528504 ) ) ;
#33785 = CARTESIAN_POINT ( 'NONE',  ( 13.62178482187499640, 197.8531250006145399, -23.59362340125807123 ) ) ;
#33786 = CARTESIAN_POINT ( 'NONE',  ( 18.12178482187499640, 4.985214923628404904, -6.178124999385470772 ) ) ;
#33787 = CARTESIAN_POINT ( 'NONE',  ( -8.962234695871565293, 35.23981371789855643, -8.715434833792128799 ) ) ;
#33788 = ORIENTED_EDGE ( 'NONE', *, *, #31566, .F. ) ;
#33789 = CIRCLE ( 'NONE', #35594, 8.000000000000000000 ) ;
#33790 = CARTESIAN_POINT ( 'NONE',  ( 16.56230152254411792, 7.209453229046482114, -0.7593749993855121172 ) ) ;
#33791 = CARTESIAN_POINT ( 'NONE',  ( 10.56230152254411081, 0.000000000000000000, -9.337499998771036758 ) ) ;
#33792 = CARTESIAN_POINT ( 'NONE',  ( -44.65252896937850835, 206.6499508600178387, -5.571401726697954970 ) ) ;
#33793 =( LENGTH_UNIT ( ) NAMED_UNIT ( * ) SI_UNIT ( .MILLI., .METRE. ) );
#33794 =( BOUNDED_CURVE ( )  B_SPLINE_CURVE ( 2, ( #11613, #23000, #26018, #20537, #35288, #31893, #29037, #23371, #26201 ),
 .UNSPECIFIED., .F., .F. ) 
 B_SPLINE_CURVE_WITH_KNOTS ( ( 3, 2, 2, 2, 3 ),
 ( 0.4375000000000000000, 0.4444444444444444198, 0.4583333333333333148, 0.4722222222222222099, 0.4791666666666666852 ),
 .UNSPECIFIED. ) 
 CURVE ( )  GEOMETRIC_REPRESENTATION_ITEM ( )  RATIONAL_B_SPLINE_CURVE ( ( 0.9330127018922194093, 0.9330127018922194093, 1.000000000000000000, 0.8660254037844387076, 1.000000000000000000, 0.8660254037844387076, 1.000000000000000000, 0.9330127018922190762, 0.9330127018922194093 ) ) 
 REPRESENTATION_ITEM ( '' )  );
#33795 = CARTESIAN_POINT ( 'NONE',  ( 13.56230152254410903, 5.196152422706636465, -2.775000000000027445 ) ) ;
#33796 = CARTESIAN_POINT ( 'NONE',  ( -2.311890736173448424, 59.67731371789855643, 12.53471296425189330 ) ) ;
#33797 = EDGE_CURVE ( 'NONE', #7868, #4455, #1866, .T. ) ;
#33798 = CARTESIAN_POINT ( 'NONE',  ( -33.77455436395489841, 206.6211998817774997, 3.209657149897401585 ) ) ;
#33799 = CARTESIAN_POINT ( 'NONE',  ( -53.36830436395489841, 209.8844732041982581, 6.500000000000000888 ) ) ;
#33800 = AXIS2_PLACEMENT_3D ( 'NONE', #2568, #2009, #13583 ) ;
#33801 = FACE_OUTER_BOUND ( 'NONE', #11728, .T. ) ;
#33802 = LINE ( 'NONE', #4424, #7704 ) ;
#33803 = CARTESIAN_POINT ( 'NONE',  ( 13.04141134922778988, 47.02731371789855075, -8.927990412390371944 ) ) ;
#33804 = CARTESIAN_POINT ( 'NONE',  ( -69.20163769728823411, 217.4189793300686233, -4.149950860017907139 ) ) ;
#33805 = CARTESIAN_POINT ( 'NONE',  ( -10.69584247140444866, 21.04768628210144854, 6.932735513423972762 ) ) ;
#33806 = CARTESIAN_POINT ( 'NONE',  ( 8.715434833791931624, 73.66018628210144925, 8.962234695871760692 ) ) ;
#33807 = EDGE_CURVE ( 'NONE', #16979, #15182, #26548, .T. ) ;
#33808 = CARTESIAN_POINT ( 'NONE',  ( -14.38691631536207183, 12.13518628210144712, 5.770363421893814682 ) ) ;
#33809 = CARTESIAN_POINT ( 'NONE',  ( 16.56230152254411436, 6.928203230275514990, -2.812500000000029754 ) ) ;
#33810 = CARTESIAN_POINT ( 'NONE',  ( -27.87471972953270338, 209.4684846313719788, -8.000000000000003553 ) ) ;
#33811 = ORIENTED_EDGE ( 'NONE', *, *, #23727, .F. ) ;
#33812 = CARTESIAN_POINT ( 'NONE',  ( 5.770363421893814682, 28.23518628210144854, 14.38691631536207183 ) ) ;
#33813 = CARTESIAN_POINT ( 'NONE',  ( -13.62178482187498396, 195.8281250006145342, 23.59362340125808188 ) ) ;
#33814 = CARTESIAN_POINT ( 'NONE',  ( -27.24356964374999635, 198.9968750006145228, 15.72908226750539384 ) ) ;
#33815 = CARTESIAN_POINT ( 'NONE',  ( 16.56230152254410726, 0.000000000000000000, -10.00000000000000000 ) ) ;
#33816 = DIRECTION ( 'NONE',  ( 0.000000000000000000, 1.000000000000000000, 0.000000000000000000 ) ) ;
#33817 = DIRECTION ( 'NONE',  ( -0.000000000000000000, -1.000000000000000000, -0.000000000000000000 ) ) ;
#33818 = CARTESIAN_POINT ( 'NONE',  ( 26.99999999999999645, 7.347880794884117764E-16, -4.725000000000006750 ) ) ;
#33819 = CARTESIAN_POINT ( 'NONE',  ( 26.75643035624999655, 248.2843750006145456, -7.049594010296217766E-16 ) ) ;
#33820 = CARTESIAN_POINT ( 'NONE',  ( 9.465287035748106703, 121.2023137178985479, -2.064181346179063237 ) ) ;
#33821 = CARTESIAN_POINT ( 'NONE',  ( 20.99999999999999645, 241.1968750006145399, -6.646953231504538984 ) ) ;
#33822 = ORIENTED_EDGE ( 'NONE', *, *, #13434, .F. ) ;
#33823 = CARTESIAN_POINT ( 'NONE',  ( -61.08705436395488420, 205.3262412349647263, -4.842901733360204020 ) ) ;
#33824 =( LENGTH_UNIT ( ) NAMED_UNIT ( * ) SI_UNIT ( .MILLI., .METRE. ) );
#33825 = CARTESIAN_POINT ( 'NONE',  ( 26.99999999999999645, 247.9937500012290457, 3.464101615137751278 ) ) ;
#33826 = CARTESIAN_POINT ( 'NONE',  ( -2.311890736173447980, 124.0773137178985621, 12.53471296425189330 ) ) ;
#33827 = CARTESIAN_POINT ( 'NONE',  ( 22.80587116629410360, 3.604726614523238837, -8.428124999385516958 ) ) ;
#33828 = CARTESIAN_POINT ( 'NONE',  ( 37.09428426793671463, -3.604726614523235284, 162.3215832362777746 ) ) ;
#33829 = CARTESIAN_POINT ( 'NONE',  ( 23.87821517812499650, 4.985214923628404904, -0.8531249993854739255 ) ) ;
#33830 = CARTESIAN_POINT ( 'NONE',  ( 13.50000000000001421, 197.4500000000000171, 23.38268590217984055 ) ) ;
#33831 = ORIENTED_EDGE ( 'NONE', *, *, #14204, .F. ) ;
#33832 = CARTESIAN_POINT ( 'NONE',  ( -8.715434833791929847, 32.26018628210145067, -8.962234695871762469 ) ) ;
#33833 = VERTEX_POINT ( 'NONE', #33776 ) ;
#33834 = EDGE_LOOP ( 'NONE', ( #37439, #12041, #30897, #17608 ) ) ;
#33835 = CARTESIAN_POINT ( 'NONE',  ( 15.00000000000000000, 3.464101615137752166, -4.031249998770949361 ) ) ;
#33836 = CARTESIAN_POINT ( 'NONE',  ( 26.75643035624999655, 7.049594010296217766E-16, -3.065624999385479832 ) ) ;
#33837 = DIRECTION ( 'NONE',  ( 1.000000000000000000, 0.000000000000000000, 0.000000000000000000 ) ) ;
#33838 = CARTESIAN_POINT ( 'NONE',  ( 24.82131618996089273, 3.464101615137476831, 162.5201233906748826 ) ) ;
#33839 = CARTESIAN_POINT ( 'NONE',  ( 21.00000000000000000, 248.5093750006144830, 6.646953231504538984 ) ) ;
#33840 = CARTESIAN_POINT ( 'NONE',  ( -4.944772684328673229, 66.18518628210144072, 11.48171059495397728 ) ) ;
#33841 = CARTESIAN_POINT ( 'NONE',  ( -67.21502896937850835, 215.5714017266979567, -3.350049139982168800 ) ) ;
#33842 = CARTESIAN_POINT ( 'NONE',  ( 14.68278727570712761, 216.3172127243002478, -0.6964482669459951536 ) ) ;
#33843 = CARTESIAN_POINT ( 'NONE',  ( -51.57961230271184405, 211.3212981617417938, 4.469044688360757966 ) ) ;
#33844 = CARTESIAN_POINT ( 'NONE',  ( 30.98804811898798661, 6.928203230275506996, 164.1639124025385001 ) ) ;
#33845 = CARTESIAN_POINT ( 'NONE',  ( -8.962234695871565293, 118.0398137178985678, -8.715434833792128799 ) ) ;
#33846 = CARTESIAN_POINT ( 'NONE',  ( -36.54538769728823411, 211.8571965466039444, -6.469044688360768625 ) ) ;
#33847 = CARTESIAN_POINT ( 'NONE',  ( -58.11830436395491262, 209.8844732041983150, 8.500000000000003553 ) ) ;
#33848 = CARTESIAN_POINT ( 'NONE',  ( 23.87821517812499650, 4.985214923628404904, -2.203124999385491556 ) ) ;
#33849 = CARTESIAN_POINT ( 'NONE',  ( 27.24356964374999635, 197.3656250006145285, -15.72908226750539029 ) ) ;
#33850 = CARTESIAN_POINT ( 'NONE',  ( -15.53471296425188442, 98.77731371789855075, -2.908627838312459080 ) ) ;
#33851 = CARTESIAN_POINT ( 'NONE',  ( -31.59002896937850124, 204.4285982733020433, 3.350049139982171020 ) ) ;
#33852 = ORIENTED_EDGE ( 'NONE', *, *, #28922, .T. ) ;
#33853 = CARTESIAN_POINT ( 'NONE',  ( 30.92921799263332261, -6.928203230275506996, 163.4914809813265606 ) ) ;
#33854 = CARTESIAN_POINT ( 'NONE',  ( -8.715434833791929847, 115.0601862821014549, -8.962234695871762469 ) ) ;
#33855 = CARTESIAN_POINT ( 'NONE',  ( -15.46528703574804986, 58.99768628210144783, -3.257655550457287497 ) ) ;
#33856 = CARTESIAN_POINT ( 'NONE',  ( 20.99999999999997868, 245.6687500012290855, 5.999999999999999112 ) ) ;
#33857 = CARTESIAN_POINT ( 'NONE',  ( 30.94147426890365438, -7.209453229046482114, 163.6315708601335359 ) ) ;
#33858 = CARTESIAN_POINT ( 'NONE',  ( -8.927990412390661490, 84.87268628210145494, 13.04141134922759804 ) ) ;
#33859 = CARTESIAN_POINT ( 'NONE',  ( -43.07663769728823411, 204.3130714775002730, 3.149950860017883603 ) ) ;
#33860 = CARTESIAN_POINT ( 'NONE',  ( 22.80587116629410360, 7.646167579472015790E-16, -7.565624999385539340 ) ) ;
#33861 = CARTESIAN_POINT ( 'NONE',  ( 8.843639120294328748, 25.93518628210144072, -3.474262827703334722 ) ) ;
#33862 = DIRECTION ( 'NONE',  ( 0.9961946980917462113, 0.000000000000000000, -0.08715574274765118534 ) ) ;
#33863 = CARTESIAN_POINT ( 'NONE',  ( -68.60788769728823411, 216.4690446883607535, 1.857196546604031662 ) ) ;
#33864 = EDGE_CURVE ( 'NONE', #33538, #33209, #7200, .T. ) ;
#33865 = CARTESIAN_POINT ( 'NONE',  ( 2.311890736173175753, 65.32268628210144357, 12.53471296425194836 ) ) ;
#33866 = CARTESIAN_POINT ( 'NONE',  ( -1.909035429704832693E-15, 196.7374999999999829, -31.17691453623979214 ) ) ;
#33867 = DIRECTION ( 'NONE',  ( 0.000000000000000000, 0.000000000000000000, 1.000000000000000000 ) ) ;
#33869 = CARTESIAN_POINT ( 'NONE',  ( 16.56230152254411436, 7.209453229046482114, -1.659374999385503591 ) ) ;
#33868 = CARTESIAN_POINT ( 'NONE',  ( 6.594114490232313663, 18.46018628210144286, 6.840914352312096547 ) ) ;
#33870 = CARTESIAN_POINT ( 'NONE',  ( 0.000000000000000000, 210.0000000000000284, 0.000000000000000000 ) ) ;
#33871 = ORIENTED_EDGE ( 'NONE', *, *, #10195, .F. ) ;
#33872 = CARTESIAN_POINT ( 'NONE',  ( 18.00000000000000000, 5.196152422706630247, -2.774999999999999467 ) ) ;
#33873 = CARTESIAN_POINT ( 'NONE',  ( 36.98809468990209126, 3.464101615138066137, 163.9024790530773430 ) ) ;
#33874 = CARTESIAN_POINT ( 'NONE',  ( 27.59297993499679791, -5.407089921784865361, 161.1765693489562352 ) ) ;
#33875 = CARTESIAN_POINT ( 'NONE',  ( 22.80587116629411071, 3.604726614523238837, -1.228124999385522331 ) ) ;
#33876 = CARTESIAN_POINT ( 'NONE',  ( 33.63672481644027812, -5.196152422706635576, 160.0172858505133604 ) ) ;
#33877 = CARTESIAN_POINT ( 'NONE',  ( 23.99999999999999645, 244.0000000000000000, -5.196152422706631135 ) ) ;
#33878 = PLANE ( 'NONE',  #37243 ) ;
#33879 = CARTESIAN_POINT ( 'NONE',  ( -8.962234695871565293, 81.23981371789855643, -8.715434833792128799 ) ) ;
#33880 = CARTESIAN_POINT ( 'NONE',  ( -2.311890736173176641, 88.32268628210145778, -12.53471296425194659 ) ) ;
#33881 = ORIENTED_EDGE ( 'NONE', *, *, #13054, .T. ) ;
#33882 = ORIENTED_EDGE ( 'NONE', *, *, #31144, .T. ) ;
#33883 = CARTESIAN_POINT ( 'NONE',  ( -13.50000000000000533, 199.1375000012290286, -23.38268590217984411 ) ) ;
#33884 = CARTESIAN_POINT ( 'NONE',  ( 37.21687851461555852, -3.464101615137548773, 166.5174901355681243 ) ) ;
#33885 = CARTESIAN_POINT ( 'NONE',  ( 2.908627838312458636, 55.07731371789854080, -15.53471296425188442 ) ) ;
#33886 = CARTESIAN_POINT ( 'NONE',  ( 26.75643035624999655, 3.323476615752271712, -9.890624999385464022 ) ) ;
#33887 = CARTESIAN_POINT ( 'NONE',  ( 15.24356964374999990, 242.2093750006145285, 0.000000000000000000 ) ) ;
#33888 = CARTESIAN_POINT ( 'NONE',  ( -58.71205436395490551, 213.2096571498974242, 3.378800118222489601 ) ) ;
#33889 = CARTESIAN_POINT ( 'NONE',  ( -7.234628195640302017, 199.6424038105676857, 27.00000000000000711 ) ) ;
#33890 = CARTESIAN_POINT ( 'NONE',  ( -9.534712964251895073, 43.57731371789854080, -1.715153634034446428 ) ) ;
#33891 = AXIS2_PLACEMENT_3D ( 'NONE', #28989, #11566, #3217 ) ;
#33892 = CARTESIAN_POINT ( 'NONE',  ( -7.954856959092309943, 97.62731371789854506, 5.529263428287300108 ) ) ;
#33893 = CARTESIAN_POINT ( 'NONE',  ( -13.62178482187500528, 199.3343750006145569, -23.59362340125807123 ) ) ;
#33894 = CARTESIAN_POINT ( 'NONE',  ( -2.660918448318004614, 17.70231371789854435, -12.46528703574811558 ) ) ;
#33895 = CARTESIAN_POINT ( 'NONE',  ( -8.962234695871760692, 57.56018628210145494, 8.715434833791933400 ) ) ;
#33896 = CARTESIAN_POINT ( 'NONE',  ( 10.56230152254411081, 0.000000000000000000, -9.337499998771036758 ) ) ;
#33897 = DIRECTION ( 'NONE',  ( -0.000000000000000000, 0.000000000000000000, 1.000000000000000000 ) ) ;
#33898 = CARTESIAN_POINT ( 'NONE',  ( 36.90145218710753738, 7.646167579472015790E-16, 160.1175024667497837 ) ) ;
#33899 = CARTESIAN_POINT ( 'NONE',  ( 16.56230152254411436, -7.209453229046482114, -9.984374999385536853 ) ) ;
#33900 = CARTESIAN_POINT ( 'NONE',  ( 19.68408634441911076, 5.407089921784862696, -7.546874999385555505 ) ) ;
#33901 = CARTESIAN_POINT ( 'NONE',  ( -13.50000000000000533, 197.6750000000000114, -23.38268590217984411 ) ) ;
#33902 = AXIS2_PLACEMENT_3D ( 'NONE', #29335, #18358, #26678 ) ;
#33903 = CARTESIAN_POINT ( 'NONE',  ( 17.00000000000000000, 4.898587196589406912E-16, -8.000000000000000000 ) ) ;
#33904 = CARTESIAN_POINT ( 'NONE',  ( 5.529263428287477744, 80.27268628210143220, -7.954856959092191815 ) ) ;
#33905 = CARTESIAN_POINT ( 'NONE',  ( 1.120210788295102201E-13, 196.8500000012290343, -27.00000000000000711 ) ) ;
#33906 = CARTESIAN_POINT ( 'NONE',  ( -4.944772684328673229, 121.3851862821014578, 11.48171059495397728 ) ) ;
#33907 = CARTESIAN_POINT ( 'NONE',  ( -14.50000000000000000, 210.0000000000000000, 0.000000000000000000 ) ) ;
#33908 = DIRECTION ( 'NONE',  ( -0.000000000000000000, -1.000000000000000000, -0.000000000000000000 ) ) ;
#33909 = ORIENTED_EDGE ( 'NONE', *, *, #26807, .T. ) ;
#33910 = CARTESIAN_POINT ( 'NONE',  ( 34.09877069215784218, -5.407089921784855591, 163.9011702523720544 ) ) ;
#33911 = CARTESIAN_POINT ( 'NONE',  ( 21.00000000000000000, -6.646953231504538984, -5.878124999385467397 ) ) ;
#33912 = CARTESIAN_POINT ( 'NONE',  ( 27.24356964375000700, 197.3468750006145740, 15.72908226750537075 ) ) ;
#33913 = CARTESIAN_POINT ( 'NONE',  ( 25.14001085782205891, 3.604726614523240613, 168.9574683606716974 ) ) ;
#33914 = DIRECTION ( 'NONE',  ( 0.000000000000000000, 1.000000000000000000, 0.000000000000000000 ) ) ;
#33915 = DIRECTION ( 'NONE',  ( 0.000000000000000000, 0.000000000000000000, 1.000000000000000000 ) ) ;
#33916 = CARTESIAN_POINT ( 'NONE',  ( 15.24356964375000167, 240.8968750006145001, 3.323476615752272600 ) ) ;
#33917 = CARTESIAN_POINT ( 'NONE',  ( 26.99999999999999645, 7.347880794884117764E-16, -3.374999999999989342 ) ) ;
#33918 = CARTESIAN_POINT ( 'NONE',  ( -10.69584247140429412, 136.1523137178985792, -6.932735513424201024 ) ) ;
#33919 = CARTESIAN_POINT ( 'NONE',  ( 8.962234695871762469, 135.7601862821014720, -8.715434833791931624 ) ) ;
#33920=STYLED_ITEM('',(#37535),#20793);
#33922 = VERTEX_POINT ( 'NONE', #19764 ) ;
#33921 = VERTEX_POINT ( 'NONE', #16347 ) ;
#33923 = CARTESIAN_POINT ( 'NONE',  ( 18.12178482187500350, 243.9718750006145171, 4.985214923628407568 ) ) ;
#33924 = CARTESIAN_POINT ( 'NONE',  ( 4.944772684328420986, 12.81481371789855395, 11.48171059495408208 ) ) ;
#33925 = CARTESIAN_POINT ( 'NONE',  ( 15.24356964374999990, 3.323476615752268604, -5.128124999385462957 ) ) ;
#33926 = CARTESIAN_POINT ( 'NONE',  ( 11.08355503943118769, 113.4398137178985593, 10.83675517735179028 ) ) ;
#33927 = CARTESIAN_POINT ( 'NONE',  ( 22.60769515458672885, 244.4674038105676743, -5.999999999999998224 ) ) ;
#33928 = EDGE_CURVE ( 'NONE', #9957, #941, #25120, .T. ) ;
#33929 = CARTESIAN_POINT ( 'NONE',  ( 15.24356964375000167, -3.323476615752272600, -2.015624999385490668 ) ) ;
#33930 = CARTESIAN_POINT ( 'NONE',  ( 16.56230152254411436, 7.209453229046482114, -7.509374999385479477 ) ) ;
#33931 = CARTESIAN_POINT ( 'NONE',  ( -1.926257025242585782E-15, 195.1906250006145456, -31.45816453501075927 ) ) ;
#33932 = CIRCLE ( 'NONE', #10935, 2.649999999999992806 ) ;
#33933 = CARTESIAN_POINT ( 'NONE',  ( 11.48171059495397728, 109.8851862821014436, 4.944772684328674117 ) ) ;
#33934 = CARTESIAN_POINT ( 'NONE',  ( 19.68408634441910721, 5.407089921784857367, -2.540624999385538096 ) ) ;
#33935 = CARTESIAN_POINT ( 'NONE',  ( -37.52752896937849414, 214.3500491399821897, 7.303452534266821949 ) ) ;
#33936 = CARTESIAN_POINT ( 'NONE',  ( 20.99999999999999645, 245.3593750006145342, 6.646953231504538984 ) ) ;
#33937 = CARTESIAN_POINT ( 'NONE',  ( 13.56230152254411614, -5.196152422706632912, -7.462499998771049192 ) ) ;
#33938 = CARTESIAN_POINT ( 'NONE',  ( -36.53794563604517265, 206.7903428501025758, 3.378800118222471838 ) ) ;
#33939 = CARTESIAN_POINT ( 'NONE',  ( 2.660918448318279950, 125.6976862821014578, -12.46528703574805697 ) ) ;
#33940 = CARTESIAN_POINT ( 'NONE',  ( 22.56230152254410370, -3.464101615137751278, -1.049999998770981602 ) ) ;
#33941 = CARTESIAN_POINT ( 'NONE',  ( -42.68080436395489841, 203.5000000000000000, -0.1155267958017335561 ) ) ;
#33942 = CARTESIAN_POINT ( 'NONE',  ( 10.56230152254411081, 0.000000000000000000, -9.337499998771036758 ) ) ;
#33943 = FILL_AREA_STYLE ('',( #36404 ) ) ;
#33944 = CARTESIAN_POINT ( 'NONE',  ( 14.25334919248782661, 128.2851862821014493, 6.092822981423971385 ) ) ;
#33945 = EDGE_CURVE ( 'NONE', #27888, #13079, #33789, .T. ) ;
#33946 = CARTESIAN_POINT ( 'NONE',  ( 20.99999999999995381, 242.5187500012290513, 5.999999999999998224 ) ) ;
#33947 = CARTESIAN_POINT ( 'NONE',  ( -12.50000000000000355, 12.71018628210143753, -0.1745138560725492671 ) ) ;
#33948 = CARTESIAN_POINT ( 'NONE',  ( 10.31873187879410736, 3.604726614523236616, -0.1781249993854788494 ) ) ;
#33949 = CARTESIAN_POINT ( 'NONE',  ( 25.01527935017339743, 2.343145750507547032, 50.00000000000000000 ) ) ;
#33950 = VERTEX_POINT ( 'NONE', #31302 ) ;
#33951 = CARTESIAN_POINT ( 'NONE',  ( 22.56230152254438437, -3.464101615137601176, -7.912500000000031619 ) ) ;
#33952 = CARTESIAN_POINT ( 'NONE',  ( -8.152565276336710909, 76.24768628210145494, 5.233372021372435512 ) ) ;
#33953 = CARTESIAN_POINT ( 'NONE',  ( -1.926257025242585782E-15, 196.5406250006145399, -31.45816453501075927 ) ) ;
#33955 = CYLINDRICAL_SURFACE ( 'NONE', #18524, 6.000000000000001776 ) ;
#33954 =( BOUNDED_CURVE ( )  B_SPLINE_CURVE ( 2, ( #15958, #9884, #30734, #6857, #7056, #27321, #4569, #27512, #33198 ),
 .UNSPECIFIED., .F., .F. ) 
 B_SPLINE_CURVE_WITH_KNOTS ( ( 3, 2, 2, 2, 3 ),
 ( 0.3804347826086956763, 0.3840579710144927383, 0.3913043478260869734, 0.3985507246376811530, 0.4021739130434782705 ),
 .UNSPECIFIED. ) 
 CURVE ( )  GEOMETRIC_REPRESENTATION_ITEM ( )  RATIONAL_B_SPLINE_CURVE ( ( 0.9330127018922194093, 0.9330127018922198534, 1.000000000000000000, 0.8660254037844387076, 1.000000000000000000, 0.8660254037844387076, 1.000000000000000000, 0.9330127018922194093, 0.9330127018922194093 ) ) 
 REPRESENTATION_ITEM ( '' )  );
#33956 = CARTESIAN_POINT ( 'NONE',  ( -27.24356964374999990, 197.1218750006145228, -15.72908226750537786 ) ) ;
#33957 = DIRECTION ( 'NONE',  ( 1.000000000000000000, 0.000000000000000000, 0.000000000000000000 ) ) ;
#33958 = CARTESIAN_POINT ( 'NONE',  ( 16.56230152254410726, 6.928203230275506996, -6.749999998770969789 ) ) ;
#33959 = CARTESIAN_POINT ( 'NONE',  ( -3.474262827703527901, 59.96481371789855075, 8.843639120294245259 ) ) ;
#33960 = CARTESIAN_POINT ( 'NONE',  ( 15.00000000000000000, 0.000000000000000000, -9.000000000000007105 ) ) ;
#33961 = VERTEX_POINT ( 'NONE', #13692 ) ;
#33962 = CARTESIAN_POINT ( 'NONE',  ( 24.00000000000000000, 240.7562500012290627, 5.196152422706629359 ) ) ;
#33963 = CARTESIAN_POINT ( 'NONE',  ( 11.61527771782809637, 57.66481371789855359, 4.622313124798827388 ) ) ;
#33964 = CARTESIAN_POINT ( 'NONE',  ( 22.80587116629411781, 3.604726614523243278, -5.784374999385522464 ) ) ;
#33965 = CARTESIAN_POINT ( 'NONE',  ( 18.12178482187500350, -4.985214923628407568, -6.928124999385470772 ) ) ;
#33966 = CARTESIAN_POINT ( 'NONE',  ( 2.660918448318002838, 31.50231371789854862, 12.46528703574811558 ) ) ;
#33967 = VECTOR ( 'NONE', #23739, 1000.000000000000000 ) ;
#33968 = VERTEX_POINT ( 'NONE', #33403 ) ;
#33969 = UNCERTAINTY_MEASURE_WITH_UNIT (LENGTH_MEASURE( 1.000000000000000082E-05 ), #32358, 'distance_accuracy_value', 'NONE');
#33970 = CARTESIAN_POINT ( 'NONE',  ( 16.56230152254411436, -7.209453229046482114, -2.334374999385513849 ) ) ;
#33971 = CARTESIAN_POINT ( 'NONE',  ( -7.234628195640313564, 199.9075961894323541, -27.00000000000000355 ) ) ;
#33972 = CARTESIAN_POINT ( 'NONE',  ( 31.43172532185919721, 7.209453229046482114, 169.2351660368996420 ) ) ;
#33973 =( BOUNDED_SURFACE ( )  B_SPLINE_SURFACE ( 1, 2, ( 
 ( #18968, #15933, #24821, #30523, #33172, #7956, #33360, #4543, #27482, #19349, #2073, #10793, #24637, #36752, #13646, #30709, #25199, #7584, #27293, #7216, #4172, #10420, #12892, #25005, #19160, #4729, #10044, #16304, #18788, #16119, #30329, #1884, #15742, #10232, #21621, #4353, #21807, #22366, #27670, #36374, #10602, #30888, #21995, #27851, #36561, #13455, #22182, #33730, #4911, #16492, #28040, #30142, #1324, #11719, #34650, #28403, #17235, #34470, #22739, #34289, #23293, #23106, #34838, #3000, #25941, #31078, #25382, #8332, #34098, #8694, #19531, #13835, #25566, #5101, #10978, #5286, #2256, #16680, #31260, #17422, #31443, #2624, #8148, #19902, #36932, #28773, #5466, #22549, #14570, #14383, #28962, #19720, #14200, #11166, #25751, #17048, #28586, #16866, #2813, #28227, #26122, #8513, #2442, #14016, #22925, #37118, #20268, #20080, #37304, #11354, #31624, #5652, #37484, #11535, #31807, #5844, #154, #8878, #20830, #35026, #17613, #12474, #29528, #6027, #9070, #12283, #3184, #12662, #23664, #711, #14760, #3375, #29143, #20456, #9633, #26873, #24043, #15322, #904, #35588, #21210, #18173, #26304, #341, #29714, #6786, #24230, #11906, #6221, #23473, #35395, #32749, #35208, #9443, #3747, #3568, #9258, #20640, #21022, #18360, #31998, #32187, #17794, #29337, #14944, #27069, #6410, #32372, #29909, #3938, #26491, #523, #15513, #17985, #12090, #1093, #15130, #26681, #23856, #32557, #6599, #27997, #13414, #7174, #33500, #13233, #1470, #13044, #2030, #1844, #13607, #19311, #4685, #9818, #4132, #24599, #12849, #24962, #35774, #30100, #4314, #21395, #27255, #21584, #18558, #32936, #10003, #33687, #10192, #18930, #24417, #36149, #15704, #7545, #21768, #1278, #30849, #30667, #7728, #35965, #30483, #27438, #4503, #33318, #7358, #33131, #19117, #6990, #4874, #24782, #18747, #30289, #1659, #15893, #36520, #36333, #16080, #27629, #10379, #21954, #16266, #27816, #10564, #22141, #16453, #25157, #37079, #13796, #33876, #28731, #8288, #22324, #25343, #28545, #19492, #28920, #2401, #17004, #31038, #19679, #7918, #36712, #25896, #5606, #2769, #31583, #17191, #14342, #37444 ),
 ( #11493, #17377, #23062, #34059, #22879, #2587, #28366, #13976, #2954, #34608, #10751, #8651, #20220, #5060, #16642, #25526, #2214, #31766, #28183, #36892, #31218, #10938, #22512, #8105, #5247, #16824, #11125, #5797, #22702, #19861, #34246, #31404, #5423, #34430, #14157, #25711, #37264, #20037, #11311, #8467, #9210, #6175, #20781, #26446, #12046, #8838, #35346, #11673, #35540, #3516, #14710, #29854, #17935, #3142, #29668, #15083, #293, #17747, #479, #23248, #32324, #6364, #23616, #32506, #14524, #26080, #35160, #26258, #34794, #18125, #29479, #20410, #11859, #26633, #31952, #18314, #29288, #662, #5984, #9022, #17564, #109, #15272, #6552, #3703, #20974, #26825, #855, #12426, #23805, #29099, #23428, #9585, #12234, #34980, #20594, #32135, #9399, #3327, #23995, #21159, #32697, #14898, #6739, #4263, #15652, #16029, #13176, #15463, #27200, #9770, #18507, #30046, #22089, #1416, #27386, #21899, #4635, #4080, #21348, #36281, #15838, #33081, #1226, #12798, #33639, #12994, #24549, #33447, #16214, #24367, #32887, #10329, #36100, #7124, #7490, #18696, #6938, #24179, #30429, #19066, #7678, #30618, #35911, #1607, #18878, #30237, #10143, #19258, #27764, #3892, #24916, #1794, #27017, #9954, #21716, #21535, #13361, #1042, #35724, #33267, #12613, #7306, #4449, #27578, #24731, #36468, #10509, #5195, #13926, #7865, #19627, #13549, #28498, #34006, #33828, #25847, #25660, #28680, #19439, #25476, #22459, #37027, #16770, #28316, #25102, #14108, #27947, #14294, #19815, #30989, #8601, #34194, #5007, #8421, #31349, #16588, #8051, #2354, #1977, #11073, #22648, #8240, #11261, #30797, #4820, #5376, #28133, #36660, #34380, #16955, #10698, #2162, #2541, #22275, #34562, #31173, #37214, #13745, #25291, #36843, #16401, #31534, #22832, #19990, #5559, #17144, #2718, #37395, #11445, #10886, #23012, #15229, #23571, #17327, #34748, #31720, #435, #2905, #15040, #35116, #20732, #14477, #14853, #20547, #31906, #32275, #29435, #5747, #5935, #26030, #3471, #28870, #3658, #9165, #20363, #35492, #6318, #8791, #35298, #17890, #17515, #23382, #6122, #58, #12000, #26402, #29240, #617 ) ),
 .UNSPECIFIED., .F., .F., .F. ) 
 B_SPLINE_SURFACE_WITH_KNOTS ( ( 2, 2 ),
 ( 3, 2, 2, 2, 2, 2, 2, 2, 2, 2, 2, 2, 2, 2, 2, 2, 2, 2, 2, 2, 2, 2, 2, 2, 2, 2, 2, 2, 2, 2, 2, 2, 2, 2, 2, 2, 2, 2, 2, 2, 2, 2, 2, 2, 2, 2, 2, 2, 2, 2, 2, 2, 2, 2, 2, 2, 2, 2, 2, 2, 2, 2, 2, 2, 2, 2, 2, 2, 2, 2, 2, 2, 2, 2, 2, 2, 2, 2, 2, 2, 2, 2, 2, 2, 2, 2, 2, 2, 2, 2, 2, 2, 2, 2, 2, 2, 2, 2, 2, 2, 2, 2, 2, 2, 2, 2, 2, 2, 2, 2, 2, 2, 2, 2, 2, 2, 2, 2, 2, 2, 2, 2, 2, 2, 2, 2, 2, 2, 2, 2, 2, 2, 2, 2, 3 ),
 ( 0.000000000000000000, 1.000000000000000000 ),
 ( 0.000000000000000000, 0.007246376811594202987, 0.01449275362318840597, 0.02173913043478260809, 0.02898550724637681195, 0.03623188405797101580, 0.04347826086956521618, 0.05072463768115942351, 0.05797101449275362389, 0.06521739130434782428, 0.07246376811594203160, 0.07971014492753622505, 0.08695652173913043237, 0.09420289855072463969, 0.1014492753623188470, 0.1086956521739130405, 0.1159420289855072478, 0.1231884057971014551, 0.1304347826086956486, 0.1376811594202898559, 0.1449275362318840632, 0.1521739130434782705, 0.1594202898550724501, 0.1666666666666666574, 0.1739130434782608647, 0.1811594202898550721, 0.1884057971014492794, 0.1956521739130434867, 0.2028985507246376940, 0.2101449275362318736, 0.2173913043478260809, 0.2246376811594202882, 0.2318840579710144956, 0.2391304347826087029, 0.2463768115942029102, 0.2536231884057971175, 0.2608695652173912971, 0.2681159420289855322, 0.2753623188405797118, 0.2826086956521738913, 0.2898550724637681264, 0.2971014492753623060, 0.3043478260869565410, 0.3115942028985507206, 0.3188405797101449002, 0.3260869565217391353, 0.3333333333333333148, 0.3405797101449275499, 0.3478260869565217295, 0.3550724637681159646, 0.3623188405797101441, 0.3695652173913043237, 0.3768115942028985588, 0.3840579710144927383, 0.3913043478260869734, 0.3985507246376811530, 0.4057971014492753881, 0.4130434782608695676, 0.4202898550724637472, 0.4275362318840579823, 0.4347826086956521618, 0.4420289855072463969, 0.4492753623188405765, 0.4565217391304347561, 0.4637681159420289911, 0.4710144927536231707, 0.4782608695652174058, 0.4855072463768115854, 0.4927536231884058204, 0.5000000000000000000, 0.5072463768115942351, 0.5144927536231883591, 0.5217391304347825942, 0.5289855072463768293, 0.5362318840579710644, 0.5434782608695651884, 0.5507246376811594235, 0.5579710144927536586, 0.5652173913043477826, 0.5724637681159420177, 0.5797101449275362528, 0.5869565217391304879, 0.5942028985507246119, 0.6014492753623188470, 0.6086956521739130821, 0.6159420289855072062, 0.6231884057971014412, 0.6304347826086956763, 0.6376811594202898004, 0.6449275362318840354, 0.6521739130434782705, 0.6594202898550725056, 0.6666666666666666297, 0.6739130434782608647, 0.6811594202898550998, 0.6884057971014492239, 0.6956521739130434590, 0.7028985507246376940, 0.7101449275362319291, 0.7173913043478260532, 0.7246376811594202882, 0.7318840579710145233, 0.7391304347826086474, 0.7463768115942028825, 0.7536231884057971175, 0.7608695652173913526, 0.7681159420289854767, 0.7753623188405797118, 0.7826086956521739468, 0.7898550724637680709, 0.7971014492753623060, 0.8043478260869565410, 0.8115942028985507761, 0.8188405797101449002, 0.8260869565217391353, 0.8333333333333333703, 0.8405797101449274944, 0.8478260869565217295, 0.8550724637681159646, 0.8623188405797101996, 0.8695652173913043237, 0.8768115942028985588, 0.8840579710144927938, 0.8913043478260869179, 0.8985507246376811530, 0.9057971014492753881, 0.9130434782608695121, 0.9202898550724637472, 0.9275362318840579823, 0.9347826086956522174, 0.9420289855072463414, 0.9492753623188405765, 0.9565217391304348116, 0.9637681159420289356, 0.9662082948456578446 ),
 .UNSPECIFIED. ) 
 GEOMETRIC_REPRESENTATION_ITEM ( )  RATIONAL_B_SPLINE_SURFACE ( (
 ( 1.000000000000000000, 0.8660254037844387076, 1.000000000000000000, 0.8660254037844387076, 1.000000000000000000, 0.8660254037844387076, 1.000000000000000000, 0.8660254037844387076, 1.000000000000000000, 0.8660254037844387076, 1.000000000000000000, 0.8660254037844387076, 1.000000000000000000, 0.8660254037844387076, 1.000000000000000000, 0.8660254037844387076, 1.000000000000000000, 0.8660254037844387076, 1.000000000000000000, 0.8660254037844387076, 1.000000000000000000, 0.8660254037844387076, 1.000000000000000000, 0.8660254037844387076, 1.000000000000000000, 0.8660254037844387076, 1.000000000000000000, 0.8660254037844387076, 1.000000000000000000, 0.8660254037844387076, 1.000000000000000000, 0.8660254037844387076, 1.000000000000000000, 0.8660254037844387076, 1.000000000000000000, 0.8660254037844387076, 1.000000000000000000, 0.8660254037844387076, 1.000000000000000000, 0.8660254037844387076, 1.000000000000000000, 0.8660254037844387076, 1.000000000000000000, 0.8660254037844387076, 1.000000000000000000, 0.8660254037844387076, 1.000000000000000000, 0.8660254037844387076, 1.000000000000000000, 0.8660254037844387076, 1.000000000000000000, 0.8660254037844387076, 1.000000000000000000, 0.8660254037844387076, 1.000000000000000000, 0.8660254037844387076, 1.000000000000000000, 0.8660254037844387076, 1.000000000000000000, 0.8660254037844387076, 1.000000000000000000, 0.8660254037844387076, 1.000000000000000000, 0.8660254037844387076, 1.000000000000000000, 0.8660254037844387076, 1.000000000000000000, 0.8660254037844387076, 1.000000000000000000, 0.8660254037844387076, 1.000000000000000000, 0.8660254037844387076, 1.000000000000000000, 0.8660254037844387076, 1.000000000000000000, 0.8660254037844387076, 1.000000000000000000, 0.8660254037844387076, 1.000000000000000000, 0.8660254037844387076, 1.000000000000000000, 0.8660254037844387076, 1.000000000000000000, 0.8660254037844387076, 1.000000000000000000, 0.8660254037844387076, 1.000000000000000000, 0.8660254037844387076, 1.000000000000000000, 0.8660254037844387076, 1.000000000000000000, 0.8660254037844387076, 1.000000000000000000, 0.8660254037844387076, 1.000000000000000000, 0.8660254037844387076, 1.000000000000000000, 0.8660254037844387076, 1.000000000000000000, 0.8660254037844387076, 1.000000000000000000, 0.8660254037844387076, 1.000000000000000000, 0.8660254037844387076, 1.000000000000000000, 0.8660254037844387076, 1.000000000000000000, 0.8660254037844387076, 1.000000000000000000, 0.8660254037844387076, 1.000000000000000000, 0.8660254037844387076, 1.000000000000000000, 0.8660254037844387076, 1.000000000000000000, 0.8660254037844387076, 1.000000000000000000, 0.8660254037844387076, 1.000000000000000000, 0.8660254037844387076, 1.000000000000000000, 0.8660254037844387076, 1.000000000000000000, 0.8660254037844387076, 1.000000000000000000, 0.8660254037844387076, 1.000000000000000000, 0.8660254037844387076, 1.000000000000000000, 0.8660254037844387076, 1.000000000000000000, 0.8660254037844387076, 1.000000000000000000, 0.8660254037844387076, 1.000000000000000000, 0.8660254037844387076, 1.000000000000000000, 0.8660254037844387076, 1.000000000000000000, 0.8660254037844387076, 1.000000000000000000, 0.8660254037844387076, 1.000000000000000000, 0.8660254037844387076, 1.000000000000000000, 0.8660254037844387076, 1.000000000000000000, 0.8660254037844387076, 1.000000000000000000, 0.8660254037844387076, 1.000000000000000000, 0.8660254037844387076, 1.000000000000000000, 0.8660254037844387076, 1.000000000000000000, 0.8660254037844387076, 1.000000000000000000, 0.8660254037844387076, 1.000000000000000000, 0.8660254037844387076, 1.000000000000000000, 0.8660254037844387076, 1.000000000000000000, 0.8660254037844387076, 1.000000000000000000, 0.8660254037844387076, 1.000000000000000000, 0.8660254037844387076, 1.000000000000000000, 0.8660254037844387076, 1.000000000000000000, 0.8660254037844387076, 1.000000000000000000, 0.8660254037844387076, 1.000000000000000000, 0.8660254037844387076, 1.000000000000000000, 0.8660254037844387076, 1.000000000000000000, 0.8660254037844387076, 1.000000000000000000, 0.8660254037844387076, 1.000000000000000000, 0.8660254037844387076, 1.000000000000000000, 0.8660254037844387076, 1.000000000000000000, 0.8660254037844387076, 1.000000000000000000, 0.8660254037844387076, 1.000000000000000000, 0.8660254037844387076, 1.000000000000000000, 0.8660254037844387076, 1.000000000000000000, 0.8660254037844387076, 1.000000000000000000, 0.8660254037844387076, 1.000000000000000000, 0.8660254037844387076, 1.000000000000000000, 0.8660254037844387076, 1.000000000000000000, 0.8660254037844387076, 1.000000000000000000, 0.8660254037844387076, 1.000000000000000000, 0.8660254037844387076, 1.000000000000000000, 0.8660254037844387076, 1.000000000000000000, 0.8660254037844387076, 1.000000000000000000, 0.8660254037844387076, 1.000000000000000000, 0.8660254037844387076, 1.000000000000000000, 0.8660254037844387076, 1.000000000000000000, 0.8660254037844387076, 1.000000000000000000, 0.8660254037844387076, 1.000000000000000000, 0.8660254037844387076, 1.000000000000000000, 0.8660254037844387076, 1.000000000000000000, 0.8660254037844387076, 1.000000000000000000, 0.8660254037844387076, 1.000000000000000000, 0.8660254037844387076, 1.000000000000000000, 0.8660254037844387076, 1.000000000000000000, 0.8660254037844387076, 1.000000000000000000, 0.8660254037844387076, 1.000000000000000000, 0.8660254037844387076, 1.000000000000000000, 0.8660254037844387076, 1.000000000000000000, 0.8660254037844387076, 1.000000000000000000, 0.8660254037844387076, 1.000000000000000000, 0.8660254037844387076, 1.000000000000000000, 0.8660254037844387076, 1.000000000000000000, 0.8660254037844387076, 1.000000000000000000, 0.8660254037844387076, 1.000000000000000000, 0.8660254037844387076, 1.000000000000000000, 0.8660254037844387076, 1.000000000000000000, 0.8660254037844387076, 1.000000000000000000, 0.8660254037844387076, 1.000000000000000000, 0.8660254037844387076, 1.000000000000000000, 0.8660254037844387076, 1.000000000000000000, 0.9548847663035771038, 0.9401541632606846832),
 ( 1.000000000000000000, 0.8660254037844387076, 1.000000000000000000, 0.8660254037844387076, 1.000000000000000000, 0.8660254037844387076, 1.000000000000000000, 0.8660254037844387076, 1.000000000000000000, 0.8660254037844387076, 1.000000000000000000, 0.8660254037844387076, 1.000000000000000000, 0.8660254037844387076, 1.000000000000000000, 0.8660254037844387076, 1.000000000000000000, 0.8660254037844387076, 1.000000000000000000, 0.8660254037844387076, 1.000000000000000000, 0.8660254037844387076, 1.000000000000000000, 0.8660254037844387076, 1.000000000000000000, 0.8660254037844387076, 1.000000000000000000, 0.8660254037844387076, 1.000000000000000000, 0.8660254037844387076, 1.000000000000000000, 0.8660254037844387076, 1.000000000000000000, 0.8660254037844387076, 1.000000000000000000, 0.8660254037844387076, 1.000000000000000000, 0.8660254037844387076, 1.000000000000000000, 0.8660254037844387076, 1.000000000000000000, 0.8660254037844387076, 1.000000000000000000, 0.8660254037844387076, 1.000000000000000000, 0.8660254037844387076, 1.000000000000000000, 0.8660254037844387076, 1.000000000000000000, 0.8660254037844387076, 1.000000000000000000, 0.8660254037844387076, 1.000000000000000000, 0.8660254037844387076, 1.000000000000000000, 0.8660254037844387076, 1.000000000000000000, 0.8660254037844387076, 1.000000000000000000, 0.8660254037844387076, 1.000000000000000000, 0.8660254037844387076, 1.000000000000000000, 0.8660254037844387076, 1.000000000000000000, 0.8660254037844387076, 1.000000000000000000, 0.8660254037844387076, 1.000000000000000000, 0.8660254037844387076, 1.000000000000000000, 0.8660254037844387076, 1.000000000000000000, 0.8660254037844387076, 1.000000000000000000, 0.8660254037844387076, 1.000000000000000000, 0.8660254037844387076, 1.000000000000000000, 0.8660254037844387076, 1.000000000000000000, 0.8660254037844387076, 1.000000000000000000, 0.8660254037844387076, 1.000000000000000000, 0.8660254037844387076, 1.000000000000000000, 0.8660254037844387076, 1.000000000000000000, 0.8660254037844387076, 1.000000000000000000, 0.8660254037844387076, 1.000000000000000000, 0.8660254037844387076, 1.000000000000000000, 0.8660254037844387076, 1.000000000000000000, 0.8660254037844387076, 1.000000000000000000, 0.8660254037844387076, 1.000000000000000000, 0.8660254037844387076, 1.000000000000000000, 0.8660254037844387076, 1.000000000000000000, 0.8660254037844387076, 1.000000000000000000, 0.8660254037844387076, 1.000000000000000000, 0.8660254037844387076, 1.000000000000000000, 0.8660254037844387076, 1.000000000000000000, 0.8660254037844387076, 1.000000000000000000, 0.8660254037844387076, 1.000000000000000000, 0.8660254037844387076, 1.000000000000000000, 0.8660254037844387076, 1.000000000000000000, 0.8660254037844387076, 1.000000000000000000, 0.8660254037844387076, 1.000000000000000000, 0.8660254037844387076, 1.000000000000000000, 0.8660254037844387076, 1.000000000000000000, 0.8660254037844387076, 1.000000000000000000, 0.8660254037844387076, 1.000000000000000000, 0.8660254037844387076, 1.000000000000000000, 0.8660254037844387076, 1.000000000000000000, 0.8660254037844387076, 1.000000000000000000, 0.8660254037844387076, 1.000000000000000000, 0.8660254037844387076, 1.000000000000000000, 0.8660254037844387076, 1.000000000000000000, 0.8660254037844387076, 1.000000000000000000, 0.8660254037844387076, 1.000000000000000000, 0.8660254037844387076, 1.000000000000000000, 0.8660254037844387076, 1.000000000000000000, 0.8660254037844387076, 1.000000000000000000, 0.8660254037844387076, 1.000000000000000000, 0.8660254037844387076, 1.000000000000000000, 0.8660254037844387076, 1.000000000000000000, 0.8660254037844387076, 1.000000000000000000, 0.8660254037844387076, 1.000000000000000000, 0.8660254037844387076, 1.000000000000000000, 0.8660254037844387076, 1.000000000000000000, 0.8660254037844387076, 1.000000000000000000, 0.8660254037844387076, 1.000000000000000000, 0.8660254037844387076, 1.000000000000000000, 0.8660254037844387076, 1.000000000000000000, 0.8660254037844387076, 1.000000000000000000, 0.8660254037844387076, 1.000000000000000000, 0.8660254037844387076, 1.000000000000000000, 0.8660254037844387076, 1.000000000000000000, 0.8660254037844387076, 1.000000000000000000, 0.8660254037844387076, 1.000000000000000000, 0.8660254037844387076, 1.000000000000000000, 0.8660254037844387076, 1.000000000000000000, 0.8660254037844387076, 1.000000000000000000, 0.8660254037844387076, 1.000000000000000000, 0.8660254037844387076, 1.000000000000000000, 0.8660254037844387076, 1.000000000000000000, 0.8660254037844387076, 1.000000000000000000, 0.8660254037844387076, 1.000000000000000000, 0.8660254037844387076, 1.000000000000000000, 0.8660254037844387076, 1.000000000000000000, 0.8660254037844387076, 1.000000000000000000, 0.8660254037844387076, 1.000000000000000000, 0.8660254037844387076, 1.000000000000000000, 0.8660254037844387076, 1.000000000000000000, 0.8660254037844387076, 1.000000000000000000, 0.8660254037844387076, 1.000000000000000000, 0.8660254037844387076, 1.000000000000000000, 0.8660254037844387076, 1.000000000000000000, 0.8660254037844387076, 1.000000000000000000, 0.8660254037844387076, 1.000000000000000000, 0.8660254037844387076, 1.000000000000000000, 0.8660254037844387076, 1.000000000000000000, 0.8660254037844387076, 1.000000000000000000, 0.8660254037844387076, 1.000000000000000000, 0.8660254037844387076, 1.000000000000000000, 0.8660254037844387076, 1.000000000000000000, 0.8660254037844387076, 1.000000000000000000, 0.8660254037844387076, 1.000000000000000000, 0.8660254037844387076, 1.000000000000000000, 0.8660254037844387076, 1.000000000000000000, 0.8660254037844387076, 1.000000000000000000, 0.8660254037844387076, 1.000000000000000000, 0.8660254037844387076, 1.000000000000000000, 0.8660254037844387076, 1.000000000000000000, 0.8660254037844387076, 1.000000000000000000, 0.8660254037844387076, 1.000000000000000000, 0.8660254037844387076, 1.000000000000000000, 0.8660254037844387076, 1.000000000000000000, 0.8660254037844387076, 1.000000000000000000, 0.9548847663035771038, 0.9401541632606846832) ) ) 
 REPRESENTATION_ITEM ( '' )  SURFACE ( )  );
#33974 = CARTESIAN_POINT ( 'NONE',  ( -41.28794563604515133, 205.3262412349647832, 4.842901733360250205 ) ) ;
#33975 = CARTESIAN_POINT ( 'NONE',  ( 22.56230152254419252, 3.464101615137697987, -0.5249999987710254334 ) ) ;
#33976 = CYLINDRICAL_SURFACE ( 'NONE', #29678, 5.999999999999994671 ) ;
#33977 = CARTESIAN_POINT ( 'NONE',  ( -6.932735513424201912, 69.45231371789856212, 10.69584247140429412 ) ) ;
#33978 = CARTESIAN_POINT ( 'NONE',  ( -66.62127896937849414, 214.5309553116392749, 1.090244570138288127 ) ) ;
#33979 = CARTESIAN_POINT ( 'NONE',  ( -48.81622103062156270, 211.6261429550005744, 6.530955311639227823 ) ) ;
#33980 = DIRECTION ( 'NONE',  ( -0.000000000000000000, -1.000000000000000000, -0.000000000000000000 ) ) ;
#33981 = CARTESIAN_POINT ( 'NONE',  ( 6.092822981423662299, 40.41481371789855359, 14.25334919248795096 ) ) ;
#33982 = CARTESIAN_POINT ( 'NONE',  ( -67.61830436395490551, 209.8844732041983150, 8.500000000000003553 ) ) ;
#33983 = CARTESIAN_POINT ( 'NONE',  ( -4.622313124798576922, 14.43518628210144250, -11.61527771782819762 ) ) ;
#33984 = AXIS2_PLACEMENT_3D ( 'NONE', #17314, #3271, #25833 ) ;
#33985 = CARTESIAN_POINT ( 'NONE',  ( -10.69584247140444866, 67.04768628210145209, 6.932735513423972762 ) ) ;
#33986 = CARTESIAN_POINT ( 'NONE',  ( -5.770363421893818234, 5.235186282101429001, -14.38691631536207005 ) ) ;
#33987 = CARTESIAN_POINT ( 'NONE',  ( 19.56230152254412502, -5.196152422706635576, -3.000000000000058176 ) ) ;
#33988 = CARTESIAN_POINT ( 'NONE',  ( 1.120210788295102201E-13, 195.0500000012290798, -27.00000000000000711 ) ) ;
#33989 = ORIENTED_EDGE ( 'NONE', *, *, #20704, .F. ) ;
#33990 = CARTESIAN_POINT ( 'NONE',  ( 13.04141134922759804, 27.37268628210144428, 8.927990412390657937 ) ) ;
#33991 = CARTESIAN_POINT ( 'NONE',  ( -27.24356964374999279, 196.2406250006145285, 15.72908226750539384 ) ) ;
#33992 = CARTESIAN_POINT ( 'NONE',  ( 13.62178482187499640, 198.3593750006145342, -23.59362340125807123 ) ) ;
#33993 = DIRECTION ( 'NONE',  ( -0.5887012860850800999, 0.8083506638593009885, -0.000000000000000000 ) ) ;
#33994 = FILL_AREA_STYLE_COLOUR ( '', #17817 ) ;
#33995 = CARTESIAN_POINT ( 'NONE',  ( 0.000000000000000000, 2.000000000000000000, 0.000000000000000000 ) ) ;
#33996 = CARTESIAN_POINT ( 'NONE',  ( 15.00000000000000000, 247.7500000000000000, 0.000000000000000000 ) ) ;
#33997 = CARTESIAN_POINT ( 'NONE',  ( 18.12178482187499640, 248.8843750006145399, -4.985214923628404904 ) ) ;
#33998 = CARTESIAN_POINT ( 'NONE',  ( 8.152565276336593669, 113.1523137178985650, 5.233372021372610483 ) ) ;
#33999 = CARTESIAN_POINT ( 'NONE',  ( 26.75643035624999655, 242.0218750006145285, -3.323476615752271268 ) ) ;
#34000 = ORIENTED_EDGE ( 'NONE', *, *, #4553, .T. ) ;
#34001 = FACE_OUTER_BOUND ( 'NONE', #18120, .T. ) ;
#34002 = SURFACE_SIDE_STYLE ('',( #19435 ) ) ;
#34003 = CARTESIAN_POINT ( 'NONE',  ( 15.00000000000000000, 247.8062500012290457, 0.000000000000000000 ) ) ;
#34004 = CARTESIAN_POINT ( 'NONE',  ( 2.311890736173452421, 119.4773137178985678, -12.53471296425189152 ) ) ;
#34005 = CARTESIAN_POINT ( 'NONE',  ( 22.80587116629411071, 7.646167579472015790E-16, -8.915624999385585170 ) ) ;
#34006 = CARTESIAN_POINT ( 'NONE',  ( 37.09755260828975310, 7.646167579472015790E-16, 162.3589405374562205 ) ) ;
#34007 = CARTESIAN_POINT ( 'NONE',  ( 26.75643035624999655, -3.323476615752267715, -0.9656249993854794100 ) ) ;
#34008 = CARTESIAN_POINT ( 'NONE',  ( 26.99999999999999645, 195.3125000000000284, -15.58845726811990495 ) ) ;
#34009 = VERTEX_POINT ( 'NONE', #25241 ) ;
#34010 = ORIENTED_EDGE ( 'NONE', *, *, #33728, .T. ) ;
#34011 = ORIENTED_EDGE ( 'NONE', *, *, #21970, .T. ) ;
#34012 = CARTESIAN_POINT ( 'NONE',  ( 15.00000000000000178, -3.464101615137757051, -5.756249998770938348 ) ) ;
#34013 = CARTESIAN_POINT ( 'NONE',  ( 23.87821517812500005, -4.985214923628404016, -1.790624999385481697 ) ) ;
#34014 = CARTESIAN_POINT ( 'NONE',  ( -66.61573224020317241, 223.4103818930302054, -7.499999999999997335 ) ) ;
#34015 =( BOUNDED_CURVE ( )  B_SPLINE_CURVE ( 2, ( #24546, #9207, #32694, #30234, #18503, #29476, #6549, #30042, #17932 ),
 .UNSPECIFIED., .F., .F. ) 
 B_SPLINE_CURVE_WITH_KNOTS ( ( 3, 2, 2, 2, 3 ),
 ( 0.4239130434782608647, 0.4275362318840579823, 0.4347826086956521618, 0.4420289855072463969, 0.4456521739130434590 ),
 .UNSPECIFIED. ) 
 CURVE ( )  GEOMETRIC_REPRESENTATION_ITEM ( )  RATIONAL_B_SPLINE_CURVE ( ( 0.9330127018922194093, 0.9330127018922194093, 1.000000000000000000, 0.8660254037844387076, 1.000000000000000000, 0.8660254037844387076, 1.000000000000000000, 0.9330127018922198534, 0.9330127018922191873 ) ) 
 REPRESENTATION_ITEM ( '' )  );
#34016 = DIRECTION ( 'NONE',  ( 0.08715574274765150453, 0.000000000000000000, 0.9961946980917461003 ) ) ;
#34017 = CARTESIAN_POINT ( 'NONE',  ( 15.24356964375000167, 247.9843750006145058, 3.323476615752272600 ) ) ;
#34018 = CARTESIAN_POINT ( 'NONE',  ( -11.48171059495397373, 59.28518628210144215, -4.944772684328680334 ) ) ;
#34019 = EDGE_CURVE ( 'NONE', #18997, #36867, #1555, .T. ) ;
#34020 = EDGE_CURVE ( 'NONE', #32727, #36330, #10788, .T. ) ;
#34021 = CARTESIAN_POINT ( 'NONE',  ( -59.89211230271182984, 203.5309553116391896, 1.857196546604092724 ) ) ;
#34022 = CARTESIAN_POINT ( 'NONE',  ( 14.14550961275246621, 216.8544903872546286, -0.3345106846829432046 ) ) ;
#34023 = CARTESIAN_POINT ( 'NONE',  ( -43.26711230271184405, 214.4690446883608104, -1.321298161741814914 ) ) ;
#34024 =( LENGTH_UNIT ( ) NAMED_UNIT ( * ) SI_UNIT ( .MILLI., .METRE. ) );
#34025 = CARTESIAN_POINT ( 'NONE',  ( 36.99789971106883257, 3.464101615137755275, 164.0145509578369740 ) ) ;
#34026 = CARTESIAN_POINT ( 'NONE',  ( 8.715434833792128799, 129.5398137178985678, -8.962234695871567070 ) ) ;
#34027 = CARTESIAN_POINT ( 'NONE',  ( -33.57663769728823411, 204.3130714775002730, 3.149950860017883603 ) ) ;
#34028 = CARTESIAN_POINT ( 'NONE',  ( -42.48288769728823411, 201.5309553116392181, -2.393094931466246855 ) ) ;
#34029 = EDGE_CURVE ( 'NONE', #15992, #8565, #36185, .T. ) ;
#34030 = ITEM_DEFINED_TRANSFORMATION ( 'NONE', 'NONE', #13587,  #17215 ) ;
#34031 = CARTESIAN_POINT ( 'NONE',  ( 26.75643035624999655, -3.323476615752267271, -1.865624999385470772 ) ) ;
#34032 = CARTESIAN_POINT ( 'NONE',  ( -27.24356964375000345, 197.1031250006145399, 0.000000000000000000 ) ) ;
#34033 = CARTESIAN_POINT ( 'NONE',  ( 10.83675517735179206, 101.9398137178985735, -11.08355503943118769 ) ) ;
#34034 = CARTESIAN_POINT ( 'NONE',  ( -65.43377896937850835, 207.8379586601372750, 8.530955311639258909 ) ) ;
#34035 = ORIENTED_EDGE ( 'NONE', *, *, #26389, .T. ) ;
#34036 = CARTESIAN_POINT ( 'NONE',  ( 26.99999999999999645, 248.8937500012290513, 3.464101615137751278 ) ) ;
#34037 = CARTESIAN_POINT ( 'NONE',  ( 11.48171059495397728, 128.2851862821014493, 4.944772684328674117 ) ) ;
#34038 = CARTESIAN_POINT ( 'NONE',  ( -2.908627838312119351, 60.72268628210144925, -15.53471296425195369 ) ) ;
#34039 = CYLINDRICAL_SURFACE ( 'NONE', #16851, 5.500000000000005329 ) ;
#34040 = CARTESIAN_POINT ( 'NONE',  ( 33.98928129033111389, 5.407089921784862696, 162.6497006628943041 ) ) ;
#34041 = CARTESIAN_POINT ( 'NONE',  ( 15.46528703574804986, 81.99768628210142651, 3.257655550457285720 ) ) ;
#34042 = CARTESIAN_POINT ( 'NONE',  ( -40.89955436395488420, 214.8429017333601792, -4.673758765035197271 ) ) ;
#34043 = CARTESIAN_POINT ( 'NONE',  ( 16.56230152254411081, -7.209453229046475009, -6.328124999385527083 ) ) ;
#34044 = CARTESIAN_POINT ( 'NONE',  ( 6.840914352312096547, 25.36018628210144854, -6.594114490232313663 ) ) ;
#34045 = CARTESIAN_POINT ( 'NONE',  ( 20.99999999999999645, -6.928203230275506996, -3.487500000000006928 ) ) ;
#34046 = CARTESIAN_POINT ( 'NONE',  ( -66.82663769728823411, 204.3130714775002730, 3.149950860017883603 ) ) ;
#34047 = FILL_AREA_STYLE_COLOUR ( '', #9949 ) ;
#34048 = CARTESIAN_POINT ( 'NONE',  ( 6.932735513423970097, 64.74768628210145494, 10.69584247140445044 ) ) ;
#34049 = CARTESIAN_POINT ( 'NONE',  ( -27.00000000000000355, 197.3000000000000114, 0.000000000000000000 ) ) ;
#34050 = DIRECTION ( 'NONE',  ( -1.000000000000000000, 2.775557561562892929E-15, 0.000000000000000000 ) ) ;
#34052 = CARTESIAN_POINT ( 'NONE',  ( 22.80587116629411426, 7.646167579472024665E-16, -2.221874999385531346 ) ) ;
#34051 = CARTESIAN_POINT ( 'NONE',  ( 8.843639120294328748, 35.13518628210143646, -3.474262827703334722 ) ) ;
#34053 = CARTESIAN_POINT ( 'NONE',  ( 23.87821517812500005, 249.1093750006145342, 4.985214923628404016 ) ) ;
#34054 = VERTEX_POINT ( 'NONE', #19571 ) ;
#34055 = CARTESIAN_POINT ( 'NONE',  ( 21.00000000000000000, 6.928203230275506996, -4.612499999999980282 ) ) ;
#34056 = DIRECTION ( 'NONE',  ( -0.000000000000000000, -0.000000000000000000, 1.000000000000000000 ) ) ;
#34057 = CARTESIAN_POINT ( 'NONE',  ( 30.64732363713033081, 7.209453229046482114, 160.2694137540738950 ) ) ;
#34058 = CARTESIAN_POINT ( 'NONE',  ( 19.68408634441910721, 5.407089921784857367, -2.540624999385538096 ) ) ;
#34059 = CARTESIAN_POINT ( 'NONE',  ( 31.43662783238875136, 7.209453229046475009, 169.2912019886672681 ) ) ;
#34060 = CARTESIAN_POINT ( 'NONE',  ( 21.00000000000000000, 243.3625000000000398, 6.928203230275506996 ) ) ;
#34061 = DIRECTION ( 'NONE',  ( 1.000000000000000000, 0.000000000000000000, 0.000000000000000000 ) ) ;
#34062 = CARTESIAN_POINT ( 'NONE',  ( 2.311890736173175753, 92.92268628210145209, 12.53471296425194659 ) ) ;
#34063 = ORIENTED_EDGE ( 'NONE', *, *, #10394, .F. ) ;
#34064 = ORIENTED_EDGE ( 'NONE', *, *, #25595, .F. ) ;
#34065 = CARTESIAN_POINT ( 'NONE',  ( 27.00000000000000355, 194.9375000012290400, -3.306546357697854128E-15 ) ) ;
#34066 = CARTESIAN_POINT ( 'NONE',  ( -7.234628195640302017, 196.9424038105676971, 27.00000000000000711 ) ) ;
#34067 = CARTESIAN_POINT ( 'NONE',  ( -6.092822981423666739, 63.41481371789855359, -14.25334919248795096 ) ) ;
#34068 = CARTESIAN_POINT ( 'NONE',  ( 15.24356964374999990, 0.000000000000000000, -8.353124999385480365 ) ) ;
#34069 = CARTESIAN_POINT ( 'NONE',  ( 18.12178482187499640, 243.0343750006145456, -4.985214923628404904 ) ) ;
#34070 = CARTESIAN_POINT ( 'NONE',  ( -43.67038769728823411, 208.6787018382581778, 4.469044688360752637 ) ) ;
#34071 = CARTESIAN_POINT ( 'NONE',  ( 37.34434378849091019, -3.464101615137651358, 167.9744248827516913 ) ) ;
#34072 = CARTESIAN_POINT ( 'NONE',  ( 5.233372021372610483, 37.25231371789855217, -8.152565276336593669 ) ) ;
#34073 = CARTESIAN_POINT ( 'NONE',  ( 22.80587116629411071, -3.604726614523235284, -9.853124999385530103 ) ) ;
#34074 = AXIS2_PLACEMENT_3D ( 'NONE', #4156, #33344, #15726 ) ;
#34075 = CARTESIAN_POINT ( 'NONE',  ( -5.233372021372612259, 87.85231371789855359, 8.152565276336593669 ) ) ;
#34076 = CARTESIAN_POINT ( 'NONE',  ( -1.926257025242585782E-15, 198.8468750006145740, -31.45816453501075927 ) ) ;
#34077 = CARTESIAN_POINT ( 'NONE',  ( -4.944772684328424539, 17.41481371789854649, -11.48171059495408031 ) ) ;
#34078 = CARTESIAN_POINT ( 'NONE',  ( -11.61527771782819940, 67.33518628210144641, 4.622313124798574258 ) ) ;
#34079 = LINE ( 'NONE', #8131, #18362 ) ;
#34080 =( BOUNDED_CURVE ( )  B_SPLINE_CURVE ( 2, ( #13084, #33543, #30889, #36753, #24638, #10979, #10794, #7217, #36189 ),
 .UNSPECIFIED., .F., .F. ) 
 B_SPLINE_CURVE_WITH_KNOTS ( ( 3, 2, 2, 2, 3 ),
 ( 0.9456521739130434590, 0.9492753623188405765, 0.9565217391304348116, 0.9637681159420289356, 0.9662082966761270653 ),
 .UNSPECIFIED. ) 
 CURVE ( )  GEOMETRIC_REPRESENTATION_ITEM ( )  RATIONAL_B_SPLINE_CURVE ( ( 0.9330127018922194093, 0.9330127018922194093, 1.000000000000000000, 0.8660254037844387076, 1.000000000000000000, 0.8660254037844387076, 1.000000000000000000, 0.9548847324609573972, 0.9401541411607521326 ) ) 
 REPRESENTATION_ITEM ( '' )  );
#34081 = CARTESIAN_POINT ( 'NONE',  ( 15.00000000000000178, 247.3374999999999773, 3.464101615137757051 ) ) ;
#34082 = CARTESIAN_POINT ( 'NONE',  ( 33.95496371662422064, 5.407089921784857367, 162.2574490005206655 ) ) ;
#34083 = FACE_OUTER_BOUND ( 'NONE', #577, .T. ) ;
#34084 = CARTESIAN_POINT ( 'NONE',  ( 10.31873187879410558, 0.000000000000000000, -6.946874999385510563 ) ) ;
#34085 = CARTESIAN_POINT ( 'NONE',  ( 10.56230152254410903, 0.000000000000000000, -5.551115123125782702E-14 ) ) ;
#34086 = CARTESIAN_POINT ( 'NONE',  ( 23.99999999999999645, 247.2062500012290229, -5.196152422706631135 ) ) ;
#34087 = CARTESIAN_POINT ( 'NONE',  ( -6.840914352312096547, 85.16018628210146346, 6.594114490232313663 ) ) ;
#34088 = VECTOR ( 'NONE', #27414, 1000.000000000000000 ) ;
#34089 = CARTESIAN_POINT ( 'NONE',  ( 0.000000000000000000, 200.0000000000000000, 0.000000000000000000 ) ) ;
#34090 = CARTESIAN_POINT ( 'NONE',  ( 4.622313124798573369, 111.0351862821014635, 11.61527771782819940 ) ) ;
#34091 = CARTESIAN_POINT ( 'NONE',  ( 26.99999999999999645, 248.8750000000000000, -7.347880794884117764E-16 ) ) ;
#34092 = LINE ( 'NONE', #16674, #431 ) ;
#34093 = ORIENTED_EDGE ( 'NONE', *, *, #23960, .F. ) ;
#34094 = CARTESIAN_POINT ( 'NONE',  ( 24.64158895398392701, -3.604726614523240613, 163.2604799309594625 ) ) ;
#34095 = CARTESIAN_POINT ( 'NONE',  ( 15.24356964375000167, -3.323476615752272600, -6.403124999385489069 ) ) ;
#34096 = CARTESIAN_POINT ( 'NONE',  ( 13.62178482187499640, 197.0093750006145399, -23.59362340125807123 ) ) ;
#34097 = CARTESIAN_POINT ( 'NONE',  ( 31.27484498491342890, 7.209453229046482114, 167.4420155803344699 ) ) ;
#34098 = CARTESIAN_POINT ( 'NONE',  ( 34.22502607998692525, -5.196152422706635576, 166.7416000626326422 ) ) ;
#34099 = CARTESIAN_POINT ( 'NONE',  ( 22.56230152254290644, 3.464101615138464041, -4.237500000000027356 ) ) ;
#34100 = CARTESIAN_POINT ( 'NONE',  ( 23.87821517812500005, 241.4593750006145285, 4.985214923628404016 ) ) ;
#34101 = CARTESIAN_POINT ( 'NONE',  ( 31.02726820322443047, 6.928203230275506996, 164.6122000166797932 ) ) ;
#34102 = CARTESIAN_POINT ( 'NONE',  ( 2.660918448318002838, 123.5023137178985735, 12.46528703574811558 ) ) ;
#34104 = VERTEX_POINT ( 'NONE', #30572 ) ;
#34103 = ORIENTED_EDGE ( 'NONE', *, *, #11433, .F. ) ;
#34105 = CARTESIAN_POINT ( 'NONE',  ( 23.87821517812499650, 243.7468750006145228, -4.985214923628404904 ) ) ;
#34106 = LINE ( 'NONE', #5295, #24978 ) ;
#34107 = CARTESIAN_POINT ( 'NONE',  ( 15.24356964374999990, 0.000000000000000000, -3.290624999385455496 ) ) ;
#34108 = CARTESIAN_POINT ( 'NONE',  ( 14.25334919248795451, 111.7148137178985792, -6.092822981423661410 ) ) ;
#34109 = CARTESIAN_POINT ( 'NONE',  ( 15.26155779561005232, -6.106572496351636126, -10.00000000000000000 ) ) ;
#34110 = CARTESIAN_POINT ( 'NONE',  ( 23.87821517812499650, 4.985214923628404904, -2.653124999385497951 ) ) ;
#34111 = CARTESIAN_POINT ( 'NONE',  ( 19.68408634441911076, 5.407089921784862696, -8.446874999385538985 ) ) ;
#34112 = STYLED_ITEM ( 'NONE', ( #25999 ), #27800 ) ;
#34113 = CARTESIAN_POINT ( 'NONE',  ( -27.00000000000000355, 199.2125000012290457, 0.000000000000000000 ) ) ;
#34114 = CARTESIAN_POINT ( 'NONE',  ( 4.944772684328679446, 116.7851862821014635, -11.48171059495397373 ) ) ;
#34115 = CARTESIAN_POINT ( 'NONE',  ( 22.80587116629410716, 7.646167579472015790E-16, -3.515624999385541294 ) ) ;
#34116 = AXIS2_PLACEMENT_3D ( 'NONE', #704, #6404, #29138 ) ;
#34117 = CARTESIAN_POINT ( 'NONE',  ( -43.46502896937849414, 217.3034525342667962, -4.350049139982195001 ) ) ;
#34118 = CARTESIAN_POINT ( 'NONE',  ( 18.12178482187500350, 244.4218750006145058, 4.985214923628407568 ) ) ;
#34119 = CARTESIAN_POINT ( 'NONE',  ( 26.99999999999999645, 240.3625000000000114, -3.464101615137755275 ) ) ;
#34120 = CARTESIAN_POINT ( 'NONE',  ( -35.74627896937850124, 205.4690446883607535, -1.090244570138286351 ) ) ;
#34121 = CARTESIAN_POINT ( 'NONE',  ( -11.61527771782819940, 122.5351862821014635, 4.622313124798574258 ) ) ;
#34122 = CARTESIAN_POINT ( 'NONE',  ( 22.56230152254411436, 3.464101615137755275, -4.574999998771017928 ) ) ;
#34123 = CARTESIAN_POINT ( 'NONE',  ( -48.22247103062156270, 206.6499508600178672, 5.571401726697986057 ) ) ;
#34124 = FACE_BOUND ( 'NONE', #11079, .T. ) ;
#34125 =( NAMED_UNIT ( * ) SI_UNIT ( $, .STERADIAN. ) SOLID_ANGLE_UNIT ( ) );
#34126 = CARTESIAN_POINT ( 'NONE',  ( -13.23911966647218463, 103.8476862821014493, 8.632099005475506459 ) ) ;
#34127 = CARTESIAN_POINT ( 'NONE',  ( 11.61527771782819940, 16.73518628210143788, -4.622313124798573369 ) ) ;
#34128 = FACE_OUTER_BOUND ( 'NONE', #25947, .T. ) ;
#34129 = CARTESIAN_POINT ( 'NONE',  ( 5.233372021372432847, 129.1476862821014322, 8.152565276336710909 ) ) ;
#34130 = EDGE_CURVE ( 'NONE', #6556, #35189, #24681, .T. ) ;
#34131 = CARTESIAN_POINT ( 'NONE',  ( 22.80587116629411071, 3.604726614523238837, -0.7781249993855585689 ) ) ;
#34132 = CARTESIAN_POINT ( 'NONE',  ( 10.56230152254410726, 0.000000000000000000, -8.887499998771003717 ) ) ;
#34133 = ORIENTED_EDGE ( 'NONE', *, *, #36505, .T. ) ;
#34134 = CYLINDRICAL_SURFACE ( 'NONE', #19775, 27.00000000000000355 ) ;
#34135=STYLED_ITEM('',(#37556),#7452);
#34136 = CARTESIAN_POINT ( 'NONE',  ( -8.710071997420127943, 59.28518628210144925, -3.796722387233380402 ) ) ;
#34137 =( GEOMETRIC_REPRESENTATION_CONTEXT ( 3 ) GLOBAL_UNCERTAINTY_ASSIGNED_CONTEXT ( ( #3567 ) ) GLOBAL_UNIT_ASSIGNED_CONTEXT ( ( #34263, #33570, #1346 ) ) REPRESENTATION_CONTEXT ( 'NONE', 'WORKASPACE' ) );
#34138 = CARTESIAN_POINT ( 'NONE',  ( 22.56230152254531518, 3.464101615137058943, -2.324999998771022813 ) ) ;
#34139 = CARTESIAN_POINT ( 'NONE',  ( 13.62178482187501416, 197.2531250006145456, 23.59362340125806767 ) ) ;
#34140 = CARTESIAN_POINT ( 'NONE',  ( 19.39230484541324628, 246.8138461906613372, -5.999999999999989342 ) ) ;
#34141 = CARTESIAN_POINT ( 'NONE',  ( 13.62178482187501416, 195.0593750006145513, 23.59362340125806767 ) ) ;
#34142 = CARTESIAN_POINT ( 'NONE',  ( 0.000000000000000000, 200.0000000000000000, 0.000000000000000000 ) ) ;
#34143 = CARTESIAN_POINT ( 'NONE',  ( 22.56230152254353527, -3.464101615138088786, -5.549999998771012244 ) ) ;
#34144 = CARTESIAN_POINT ( 'NONE',  ( 9.534712964251900402, 48.17731371789854222, 1.715153634034445540 ) ) ;
#34145 = CARTESIAN_POINT ( 'NONE',  ( 18.00000000000000355, -5.196152422706632912, -8.924999999999988276 ) ) ;
#34146 = ORIENTED_EDGE ( 'NONE', *, *, #31242, .F. ) ;
#34147 = CARTESIAN_POINT ( 'NONE',  ( 26.99999999999999645, 242.6687500012290570, -3.464101615137755275 ) ) ;
#34148 = CARTESIAN_POINT ( 'NONE',  ( -11.61527771782809282, 71.46481371789856496, -4.622313124798832717 ) ) ;
#34149 = CARTESIAN_POINT ( 'NONE',  ( 10.31873187879410736, -3.604726614523244610, -6.909374999385495819 ) ) ;
#34150 = CARTESIAN_POINT ( 'NONE',  ( 26.75643035624999655, 7.049594010296217766E-16, -6.328124999385481786 ) ) ;
#34151 = CARTESIAN_POINT ( 'NONE',  ( -8.715434833792127023, 23.73981371789854578, 8.962234695871568846 ) ) ;
#34152 = EDGE_CURVE ( 'NONE', #33087, #11055, #31123, .T. ) ;
#34153 = ORIENTED_EDGE ( 'NONE', *, *, #6580, .F. ) ;
#34154 = CARTESIAN_POINT ( 'NONE',  ( 22.80587116629412492, 3.604726614523243278, -1.284374999385501370 ) ) ;
#34155 = EDGE_CURVE ( 'NONE', #20388, #23009, #21851, .T. ) ;
#34156 = CARTESIAN_POINT ( 'NONE',  ( 21.00000000000000000, 246.1187500012290457, 5.999999999999998224 ) ) ;
#34157 = CARTESIAN_POINT ( 'NONE',  ( -30.79836230271183695, 204.3130714775002446, -3.149950860017828091 ) ) ;
#34158 = EDGE_CURVE ( 'NONE', #35111, #19498, #462, .T. ) ;
#34159 = CARTESIAN_POINT ( 'NONE',  ( -46.82961230271183695, 211.8571965466040297, 6.469044688360755302 ) ) ;
#34160 = CARTESIAN_POINT ( 'NONE',  ( 34.39171143809891618, -5.196152422706629359, 168.6468224239574454 ) ) ;
#34161 = AXIS2_PLACEMENT_3D ( 'NONE', #27191, #24539, #16205 ) ;
#34162 = SHAPE_REPRESENTATION_RELATIONSHIP ( 'NONE' , 'NONE' ,  #2638, #27800 ) ;
#34163 = CARTESIAN_POINT ( 'NONE',  ( -9.014689842941500331, 195.0000000000000000, 25.72782777481439709 ) ) ;
#34164 = CARTESIAN_POINT ( 'NONE',  ( -66.42336230271182274, 213.9548777149308023, 2.149950860017852960 ) ) ;
#34165 = CARTESIAN_POINT ( 'NONE',  ( -41.88913769728823411, 206.8500491399821044, -5.686928522499717253 ) ) ;
#34166 = ORIENTED_EDGE ( 'NONE', *, *, #9030, .T. ) ;
#34167 = CARTESIAN_POINT ( 'NONE',  ( -26.99999999999999645, 196.8875000000000171, 15.58845726811991561 ) ) ;
#34168 = CARTESIAN_POINT ( 'NONE',  ( 16.56230152254411792, 6.928203230275514990, -1.462500000000010125 ) ) ;
#34169 = CARTESIAN_POINT ( 'NONE',  ( -3.257655550456946880, 45.30231371789854933, -15.46528703574811736 ) ) ;
#34170 = CARTESIAN_POINT ( 'NONE',  ( -30.20461230271183339, 207.6069050685336492, -8.469044688360751749 ) ) ;
#34171 = CARTESIAN_POINT ( 'NONE',  ( -10.69584247140444866, 11.84768628210144925, 6.932735513423972762 ) ) ;
#34172 =( BOUNDED_CURVE ( )  B_SPLINE_CURVE ( 2, ( #35439, #9487, #4170, #32791, #7030, #24455, #6640, #944, #24082 ),
 .UNSPECIFIED., .F., .F. ) 
 B_SPLINE_CURVE_WITH_KNOTS ( ( 3, 2, 2, 2, 3 ),
 ( 0.7065217391304348116, 0.7101449275362319291, 0.7173913043478260532, 0.7246376811594202882, 0.7282608695652174058 ),
 .UNSPECIFIED. ) 
 CURVE ( )  GEOMETRIC_REPRESENTATION_ITEM ( )  RATIONAL_B_SPLINE_CURVE ( ( 0.9330127018922194093, 0.9330127018922194093, 1.000000000000000000, 0.8660254037844387076, 1.000000000000000000, 0.8660254037844387076, 1.000000000000000000, 0.9330127018922194093, 0.9330127018922194093 ) ) 
 REPRESENTATION_ITEM ( '' )  );
#34173 = CARTESIAN_POINT ( 'NONE',  ( -10.49813415415989581, 50.37268628210145494, -7.228626920339068285 ) ) ;
#34174 = CARTESIAN_POINT ( 'NONE',  ( -15.46528703574804986, 12.99768628210143362, -3.257655550457287497 ) ) ;
#34175 = CARTESIAN_POINT ( 'NONE',  ( 13.56230152254411436, -5.196152422706638241, -3.075000000000049916 ) ) ;
#34176 = CARTESIAN_POINT ( 'NONE',  ( 15.00000000000000000, 247.8062500012290457, 0.000000000000000000 ) ) ;
#34177 = ORIENTED_EDGE ( 'NONE', *, *, #29538, .F. ) ;
#34178 = CARTESIAN_POINT ( 'NONE',  ( 0.1745138560725837118, 5.810186282101448718, -15.50000000000000533 ) ) ;
#34179 = CARTESIAN_POINT ( 'NONE',  ( 5.778771075727756162E-15, 196.3156250006145171, 31.45816453501076637 ) ) ;
#34180 = ADVANCED_FACE ( 'NONE', ( #27714 ), #11022, .T. ) ;
#34181 = CARTESIAN_POINT ( 'NONE',  ( 13.62178482187499640, 197.9093750006145456, -23.59362340125807123 ) ) ;
#34182 = CARTESIAN_POINT ( 'NONE',  ( -100.7560012262353411, 61.79101779669657191, -5.000000000000000000 ) ) ;
#34183 = CARTESIAN_POINT ( 'NONE',  ( 27.00000000000001421, 195.6875000000000000, 15.58845726811988897 ) ) ;
#34184 = CARTESIAN_POINT ( 'NONE',  ( 13.50000000000001421, 196.2125000012290172, 23.38268590217984055 ) ) ;
#34185 = CARTESIAN_POINT ( 'NONE',  ( 15.24356964374999990, 248.9218750006145058, -3.323476615752268604 ) ) ;
#34186 = CARTESIAN_POINT ( 'NONE',  ( 9.500000000000005329, 112.2898137178985678, -0.1745138560723090149 ) ) ;
#34187 = CARTESIAN_POINT ( 'NONE',  ( 23.87821517812499650, 242.0593750006145228, -4.985214923628404904 ) ) ;
#34188 = ORIENTED_EDGE ( 'NONE', *, *, #5656, .T. ) ;
#34189 = CARTESIAN_POINT ( 'NONE',  ( -69.59747103062156270, 213.3500491399821328, -5.571401726697985168 ) ) ;
#34190 = CARTESIAN_POINT ( 'NONE',  ( 18.00000000000000000, 248.1812500012290457, -5.196152422706630247 ) ) ;
#34191 = CARTESIAN_POINT ( 'NONE',  ( -11.61527771782809282, 126.6648137178985678, -4.622313124798832717 ) ) ;
#34192 = EDGE_CURVE ( 'NONE', #12159, #12005, #24869, .T. ) ;
#34193 = CARTESIAN_POINT ( 'NONE',  ( 10.31873187879411091, 0.000000000000000000, -9.140624999385559946 ) ) ;
#34194 = CARTESIAN_POINT ( 'NONE',  ( 24.59910052939444824, 0.000000000000000000, 162.7748350156397521 ) ) ;
#34195 = CARTESIAN_POINT ( 'NONE',  ( 21.00000000000000000, 240.7187500012290400, 5.999999999999998224 ) ) ;
#34196 = CARTESIAN_POINT ( 'NONE',  ( 27.00000000000000355, 195.2750000000000057, -3.306546357697854128E-15 ) ) ;
#34197 = ORIENTED_EDGE ( 'NONE', *, *, #31562, .T. ) ;
#34198 = EDGE_LOOP ( 'NONE', ( #33201, #36193, #7088, #29075, #24235 ) ) ;
#34199 =( BOUNDED_CURVE ( )  B_SPLINE_CURVE ( 2, ( #2362, #32098, #6130, #26786, #23766, #12388, #29630 ),
 .UNSPECIFIED., .F., .F. ) 
 B_SPLINE_CURVE_WITH_KNOTS ( ( 3, 2, 2, 3 ),
 ( 0.08695652173912893357, 0.09420289855072321028, 0.1014492753623174870, 0.1086956521739117498 ),
 .UNSPECIFIED. ) 
 CURVE ( )  GEOMETRIC_REPRESENTATION_ITEM ( )  RATIONAL_B_SPLINE_CURVE ( ( 1.000000000000027534, 0.8660254037844109520, 1.000000000000000000, 0.8660254037844387076, 1.000000000000000000, 0.8660254037844625774, 0.9999999999999761302 ) ) 
 REPRESENTATION_ITEM ( '' )  );
#34200 = EDGE_LOOP ( 'NONE', ( #28046, #6764, #30040, #19445, #17300, #20275, #7642, #6227 ) ) ;
#34201 = CARTESIAN_POINT ( 'NONE',  ( 26.99999999999999645, -3.464101615137751278, -4.706249998770958953 ) ) ;
#34202 = CARTESIAN_POINT ( 'NONE',  ( 18.12178482187499640, 4.985214923628404904, -3.365624999385474769 ) ) ;
#34203 = CARTESIAN_POINT ( 'NONE',  ( 23.99999999999999645, 5.196152422706631135, -6.450000000000011724 ) ) ;
#34204 = CARTESIAN_POINT ( 'NONE',  ( 34.26424616422337266, -5.196152422706635576, 167.1898876767739353 ) ) ;
#34205 = CARTESIAN_POINT ( 'NONE',  ( 26.75643035624999655, 248.6218750006145228, -7.049594010296217766E-16 ) ) ;
#34206 = EDGE_CURVE ( 'NONE', #20737, #8598, #23774, .T. ) ;
#34207 = CARTESIAN_POINT ( 'NONE',  ( 7.228626920339068285, 52.67268628210144499, -10.49813415415989581 ) ) ;
#34208 = CARTESIAN_POINT ( 'NONE',  ( -57.31919563604516554, 216.5000000000000000, -0.1155267958017906493 ) ) ;
#34209 = CARTESIAN_POINT ( 'NONE',  ( 15.31535524866699483, 225.1590526702200634, -1.929602858955059341 ) ) ;
#34210 = CARTESIAN_POINT ( 'NONE',  ( -46.23586230271182984, 207.8500491399821613, 3.954877714930852495 ) ) ;
#34211 = CARTESIAN_POINT ( 'NONE',  ( 33.97336387291019122, 5.196152422706631135, 163.8650878731170906 ) ) ;
#34212 = CARTESIAN_POINT ( 'NONE',  ( 12.50000000000000355, 130.6898137178985735, -0.1745138560722771515 ) ) ;
#34213 = CARTESIAN_POINT ( 'NONE',  ( -69.99330436395489130, 210.1155267958017703, -4.499999999999996447 ) ) ;
#34214 = CARTESIAN_POINT ( 'NONE',  ( -46.24330436395489841, 210.1155267958016850, -8.500000000000003553 ) ) ;
#34215 = CONTEXT_DEPENDENT_SHAPE_REPRESENTATION ( #4223, #8647 ) ;
#34216 = CARTESIAN_POINT ( 'NONE',  ( 23.87821517812499650, 4.985214923628404904, -4.003124999385487826 ) ) ;
#34217 = CARTESIAN_POINT ( 'NONE',  ( 13.62178482187501416, 197.2531250006145456, 23.59362340125806767 ) ) ;
#34218 = CARTESIAN_POINT ( 'NONE',  ( -10.83675517735179028, 88.13981371789856212, 11.08355503943118947 ) ) ;
#34219 = CARTESIAN_POINT ( 'NONE',  ( -36.53794563604517265, 205.3262412349647832, 4.842901733360250205 ) ) ;
#34220 = ORIENTED_EDGE ( 'NONE', *, *, #29725, .F. ) ;
#34221 = LINE ( 'NONE', #22859, #24101 ) ;
#34222 = CARTESIAN_POINT ( 'NONE',  ( -4.944772684328673229, 121.3851862821014578, 11.48171059495397728 ) ) ;
#34223 = CARTESIAN_POINT ( 'NONE',  ( 2.908627838312118019, 56.12268628210142651, 15.53471296425195369 ) ) ;
#34224 = AXIS2_PLACEMENT_3D ( 'NONE', #3931, #30090, #35766 ) ;
#34225 = LINE ( 'NONE', #5226, #12619 ) ;
#34226 = CARTESIAN_POINT ( 'NONE',  ( 24.59419801886489054, 0.000000000000000000, 162.7187990638720976 ) ) ;
#34227 = CARTESIAN_POINT ( 'NONE',  ( -14.25334919248782306, 77.68518628210145494, -6.092822981423979378 ) ) ;
#34228 = EDGE_CURVE ( 'NONE', #31223, #31993, #11053, .T. ) ;
#34229 = CARTESIAN_POINT ( 'NONE',  ( 22.80587116629411071, 3.604726614523238837, -6.178124999385540050 ) ) ;
#34230 = CARTESIAN_POINT ( 'NONE',  ( -6.594114490232312775, 23.06018628210144783, -6.840914352312096547 ) ) ;
#34231 = CARTESIAN_POINT ( 'NONE',  ( 18.00000000000000000, 5.196152422706630247, -4.124999999999989342 ) ) ;
#34232 = CARTESIAN_POINT ( 'NONE',  ( -65.83705436395487709, 205.3262412349647263, -4.842901733360204020 ) ) ;
#34233 = LINE ( 'NONE', #13595, #23869 ) ;
#34234 = CARTESIAN_POINT ( 'NONE',  ( 12.53471296425194836, 53.82268628210144357, -2.311890736173178418 ) ) ;
#34235 = CARTESIAN_POINT ( 'NONE',  ( 27.00000000000000355, 198.8750000000000284, -3.306546357697854128E-15 ) ) ;
#34236 = CARTESIAN_POINT ( 'NONE',  ( 20.99999999999999645, 185.0294372515228645, 0.000000000000000000 ) ) ;
#34238 = CARTESIAN_POINT ( 'NONE',  ( 19.68408634441912142, -5.407089921784861808, -2.746874999385529037 ) ) ;
#34237 = CARTESIAN_POINT ( 'NONE',  ( -8.152565276336710909, 21.04768628210144499, 5.233372021372435512 ) ) ;
#34239 = CARTESIAN_POINT ( 'NONE',  ( 20.99999999999999645, 249.0718750006145399, 6.646953231504538984 ) ) ;
#34240 = ORIENTED_EDGE ( 'NONE', *, *, #35989, .F. ) ;
#34241 = CARTESIAN_POINT ( 'NONE',  ( 23.99999999999999645, 5.196152422706631135, -4.200000000000009059 ) ) ;
#34242 =( BOUNDED_CURVE ( )  B_SPLINE_CURVE ( 2, ( #13261, #7574, #24995, #36920, #33532, #10593, #31069 ),
 .UNSPECIFIED., .F., .F. ) 
 B_SPLINE_CURVE_WITH_KNOTS ( ( 3, 2, 2, 3 ),
 ( 0.5652173913043474496, 0.5724637681159416847, 0.5797101449275359197, 0.5869565217391301548 ),
 .UNSPECIFIED. ) 
 CURVE ( )  GEOMETRIC_REPRESENTATION_ITEM ( )  RATIONAL_B_SPLINE_CURVE ( ( 1.000000000000006217, 0.8660254037844326014, 1.000000000000000000, 0.8660254037844387076, 1.000000000000000000, 0.8660254037844448138, 0.9999999999999938938 ) ) 
 REPRESENTATION_ITEM ( '' )  );
#34243 = CARTESIAN_POINT ( 'NONE',  ( 37.14824336730885079, -3.464101615137567869, 165.7329868120451692 ) ) ;
#34244 = CARTESIAN_POINT ( 'NONE',  ( 24.51575785039200284, 0.000000000000000000, 161.8222238355895399 ) ) ;
#34245 = CARTESIAN_POINT ( 'NONE',  ( 13.44051670066911264, -5.407089921784859143, -2.765624999385540850 ) ) ;
#34246 = CARTESIAN_POINT ( 'NONE',  ( 37.56819361912707222, 7.646167579472015790E-16, 167.7383919071516516 ) ) ;
#34247 = CARTESIAN_POINT ( 'NONE',  ( 15.00000000000000000, 243.2125000000000057, -3.464101615137752166 ) ) ;
#34248 = CARTESIAN_POINT ( 'NONE',  ( 0.000000000000000000, -20.00000000000000000, 4.899999999999999467 ) ) ;
#34249 = CARTESIAN_POINT ( 'NONE',  ( -12.50000000000000355, 77.11018628210145209, -0.1745138560725492671 ) ) ;
#34250 = ORIENTED_EDGE ( 'NONE', *, *, #19844, .F. ) ;
#34251 = ORIENTED_EDGE ( 'NONE', *, *, #21488, .T. ) ;
#34252 = CARTESIAN_POINT ( 'NONE',  ( -13.49999999999998401, 197.0375000012290627, 23.38268590217985476 ) ) ;
#34253 = CARTESIAN_POINT ( 'NONE',  ( 3.037124061885436328E-15, 148.0000000000000000, 24.80000000000000426 ) ) ;
#34254 = CARTESIAN_POINT ( 'NONE',  ( 0.1745138560722461762, 40.98981371789854933, 15.50000000000000533 ) ) ;
#34255 = CARTESIAN_POINT ( 'NONE',  ( 26.75643035624999655, 7.049594010296217766E-16, -8.128124999385477167 ) ) ;
#34256 = AXIS2_PLACEMENT_3D ( 'NONE', #6947, #9963, #7315 ) ;
#34257 = CARTESIAN_POINT ( 'NONE',  ( 15.24356964374999990, 241.7218750006145171, -3.323476615752268604 ) ) ;
#34258 = CARTESIAN_POINT ( 'NONE',  ( -44.26413769728823411, 212.1499508600178387, 3.954877714930865817 ) ) ;
#34259 = CARTESIAN_POINT ( 'NONE',  ( 23.99999999999999645, 5.196152422706631135, -6.393749998770958953 ) ) ;
#34260 = CARTESIAN_POINT ( 'NONE',  ( 37.09591843811324452, 3.604726614523243278, 162.3402618868670118 ) ) ;
#34261 = CARTESIAN_POINT ( 'NONE',  ( -0.1745138560723084320, 36.38981371789855501, -9.500000000000005329 ) ) ;
#34262 = FACE_OUTER_BOUND ( 'NONE', #31399, .T. ) ;
#34263 =( LENGTH_UNIT ( ) NAMED_UNIT ( * ) SI_UNIT ( .MILLI., .METRE. ) );
#34264 = CARTESIAN_POINT ( 'NONE',  ( 3.474262827703532341, 101.3648137178985706, -8.843639120294245259 ) ) ;
#34265 = CARTESIAN_POINT ( 'NONE',  ( 27.24356964374999635, 197.8718750006145513, -15.72908226750539029 ) ) ;
#34266 = CARTESIAN_POINT ( 'NONE',  ( 11.08355503943118769, 141.0398137178985678, 10.83675517735179028 ) ) ;
#34267 = EDGE_CURVE ( 'NONE', #19072, #26373, #22965, .T. ) ;
#34268 = CARTESIAN_POINT ( 'NONE',  ( 8.962234695871762469, 71.36018628210145209, -8.715434833791931624 ) ) ;
#34269 = CARTESIAN_POINT ( 'NONE',  ( 16.56230152254411436, -6.928203230275506996, -10.12499999877101864 ) ) ;
#34270 = DIRECTION ( 'NONE',  ( 0.000000000000000000, -0.9932091452657081376, -0.1163425707149433747 ) ) ;
#34271 = CARTESIAN_POINT ( 'NONE',  ( 37.64499961742345135, 3.604726614523243278, 168.6162884848450005 ) ) ;
#34272 = ADVANCED_FACE ( 'NONE', ( #8740 ), #11766, .T. ) ;
#34273 = CARTESIAN_POINT ( 'NONE',  ( 26.99999999999999645, 7.347880794884117764E-16, -0.6187499987709565996 ) ) ;
#34274 = CARTESIAN_POINT ( 'NONE',  ( 16.56230152254411436, 7.209453229046482114, -8.409374999385503813 ) ) ;
#34275 = CARTESIAN_POINT ( 'NONE',  ( 20.99999999999999289, 244.0374999999999943, -5.999999999999997335 ) ) ;
#34276 = CARTESIAN_POINT ( 'NONE',  ( 3.796722387233379514, 79.98518628210145209, -8.710071997420127943 ) ) ;
#34277 = FACE_BOUND ( 'NONE', #18885, .T. ) ;
#34278 = EDGE_CURVE ( 'NONE', #23622, #32985, #13725, .T. ) ;
#34279 = AXIS2_PLACEMENT_3D ( 'NONE', #36228, #31115, #25420 ) ;
#34280 = CARTESIAN_POINT ( 'NONE',  ( -12.46528703574805697, 114.1976862821014720, -2.660918448318280838 ) ) ;
#34281 = CARTESIAN_POINT ( 'NONE',  ( 21.00000000000000000, 248.7624999999999886, 5.999999999999998224 ) ) ;
#34282 = CARTESIAN_POINT ( 'NONE',  ( 10.56230152254383903, -3.464101615137600287, -0.4125000000000343392 ) ) ;
#34283 = VERTEX_POINT ( 'NONE', #25979 ) ;
#34284 = CARTESIAN_POINT ( 'NONE',  ( 30.76988640036921652, 7.209453229046475009, 161.6703125482654286 ) ) ;
#34285 = CARTESIAN_POINT ( 'NONE',  ( 15.24356964375000167, -3.323476615752272600, -7.753124999385476279 ) ) ;
#34286 = CARTESIAN_POINT ( 'NONE',  ( 27.24356964375000345, 196.0343750006145456, -3.336375036156643733E-15 ) ) ;
#34287 = CARTESIAN_POINT ( 'NONE',  ( 28.18128119854344860, -5.407089921784865361, 167.9008835610755455 ) ) ;
#34288 =( BOUNDED_CURVE ( )  B_SPLINE_CURVE ( 2, ( #6591, #21202, #29706, #333, #26673, #6403, #32178, #6214, #11711 ),
 .UNSPECIFIED., .F., .F. ) 
 B_SPLINE_CURVE_WITH_KNOTS ( ( 3, 2, 2, 2, 3 ),
 ( 0.02083333333333333565, 0.02777777777777777624, 0.04166666666666666435, 0.05555555555555555247, 0.06250000000000000000 ),
 .UNSPECIFIED. ) 
 CURVE ( )  GEOMETRIC_REPRESENTATION_ITEM ( )  RATIONAL_B_SPLINE_CURVE ( ( 0.9330127018922194093, 0.9330127018922194093, 1.000000000000000000, 0.8660254037844387076, 1.000000000000000000, 0.8660254037844387076, 1.000000000000000000, 0.9330127018922194093, 0.9330127018922194093 ) ) 
 REPRESENTATION_ITEM ( '' )  );
#34289 = CARTESIAN_POINT ( 'NONE',  ( 25.28868886033853158, -3.464101615137761048, 167.8622174579674606 ) ) ;
#34290 = CARTESIAN_POINT ( 'NONE',  ( 19.56230152254411792, 5.196152422706637353, -4.200000000000036593 ) ) ;
#34291 = CARTESIAN_POINT ( 'NONE',  ( 15.24356964374999990, 241.7218750006145171, -3.323476615752268604 ) ) ;
#34292 = CARTESIAN_POINT ( 'NONE',  ( 13.62178482187501416, 198.6031250006145399, 23.59362340125806767 ) ) ;
#34293 = CARTESIAN_POINT ( 'NONE',  ( 8.962234695871567070, 122.6398137178985621, 8.715434833792127023 ) ) ;
#34294 = CARTESIAN_POINT ( 'NONE',  ( 13.62178482187501416, 195.5093750006145399, 23.59362340125806767 ) ) ;
#34296 = ORIENTED_EDGE ( 'NONE', *, *, #33589, .T. ) ;
#34295 = ORIENTED_EDGE ( 'NONE', *, *, #5154, .T. ) ;
#34297 = CARTESIAN_POINT ( 'NONE',  ( 26.75643035624999655, 241.4218750006145058, -7.049594010296217766E-16 ) ) ;
#34298 = LINE ( 'NONE', #24831, #37095 ) ;
#34299 = CARTESIAN_POINT ( 'NONE',  ( -5.770363421894122880, 96.76481371789854791, 14.38691631536194393 ) ) ;
#34300 = CARTESIAN_POINT ( 'NONE',  ( 7.228626920339068285, 98.67268628210145209, -10.49813415415989581 ) ) ;
#34301 = CARTESIAN_POINT ( 'NONE',  ( 26.75643035624999655, -3.323476615752267715, -1.415624999385507232 ) ) ;
#34302 = CARTESIAN_POINT ( 'NONE',  ( 26.99999999999999645, 199.4750000012290343, -15.58845726811990495 ) ) ;
#34303 = CARTESIAN_POINT ( 'NONE',  ( -4.944772684328673229, 121.3851862821014578, 11.48171059495397728 ) ) ;
#34304 = CARTESIAN_POINT ( 'NONE',  ( 19.68408634441910721, -5.407089921784855591, -4.040624999385538985 ) ) ;
#34305 =( BOUNDED_CURVE ( )  B_SPLINE_CURVE ( 2, ( #24318, #27340, #21107, #26957, #21664, #15791, #30187 ),
 .UNSPECIFIED., .F., .F. ) 
 B_SPLINE_CURVE_WITH_KNOTS ( ( 3, 2, 2, 3 ),
 ( 0.5217391304347815950, 0.5289855072463750529, 0.5362318840579683998, 0.5434782608695617467 ),
 .UNSPECIFIED. ) 
 CURVE ( )  GEOMETRIC_REPRESENTATION_ITEM ( )  RATIONAL_B_SPLINE_CURVE ( ( 1.000000000000018430, 0.8660254037844202779, 1.000000000000000000, 0.8660254037844387076, 1.000000000000000000, 0.8660254037845023234, 0.9999999999999363842 ) ) 
 REPRESENTATION_ITEM ( '' )  );
#34306 = CARTESIAN_POINT ( 'NONE',  ( 20.99999999999999645, 244.9093750006145171, 6.646953231504538984 ) ) ;
#34307 = CARTESIAN_POINT ( 'NONE',  ( 13.56230152254411436, -5.196152422706632912, -1.612499998771027565 ) ) ;
#34308 = CARTESIAN_POINT ( 'NONE',  ( -54.74627896937848703, 203.4690446883607535, -1.626142955000504209 ) ) ;
#34309 = CARTESIAN_POINT ( 'NONE',  ( 4.622313124798573369, 120.2351862821014663, 11.61527771782819940 ) ) ;
#34310 = CARTESIAN_POINT ( 'NONE',  ( 19.56230152254410370, 5.196152422706631135, -2.737499998770986931 ) ) ;
#34311 = CARTESIAN_POINT ( 'NONE',  ( -42.28497103062156270, 204.4285982733020148, -3.350049139982115509 ) ) ;
#34312 = CARTESIAN_POINT ( 'NONE',  ( 0.000000000000000000, 210.0000000000000284, 0.000000000000000000 ) ) ;
#34313 = CARTESIAN_POINT ( 'NONE',  ( 2.999999999999997335, 244.5000000000000000, -10.00000000000000000 ) ) ;
#34314 = CARTESIAN_POINT ( 'NONE',  ( 10.83675517735155225, 101.2601862821014436, 11.08355503943142573 ) ) ;
#34315 = AXIS2_PLACEMENT_3D ( 'NONE', #34676, #7985, #8721 ) ;
#34316 = CARTESIAN_POINT ( 'NONE',  ( -10.49813415415989404, 22.77268628210143930, -7.228626920339069173 ) ) ;
#34317 = CARTESIAN_POINT ( 'NONE',  ( -9.465287035748065847, 123.3976862821014606, -2.064181346179273735 ) ) ;
#34318 = CARTESIAN_POINT ( 'NONE',  ( 13.44051670066911441, -5.407089921784859143, -2.315624999385534899 ) ) ;
#34319 = CARTESIAN_POINT ( 'NONE',  ( 27.88507211235645400, 5.196152422706630247, 163.1178740895360306 ) ) ;
#34320 = ORIENTED_EDGE ( 'NONE', *, *, #4942, .F. ) ;
#34321 = CARTESIAN_POINT ( 'NONE',  ( 37.61068204371655099, 3.604726614523238837, 168.2240368224713620 ) ) ;
#34322 = CARTESIAN_POINT ( 'NONE',  ( 2.064181346179272847, 61.29768628210142367, -9.465287035748065847 ) ) ;
#34323 = CARTESIAN_POINT ( 'NONE',  ( 15.24356964375000167, -3.323476615752272600, -0.5531249993854806535 ) ) ;
#34324 = CARTESIAN_POINT ( 'NONE',  ( -20.86978604919638869, 194.8026013911397740, -17.51182792271053046 ) ) ;
#34325 = DIRECTION ( 'NONE',  ( 0.000000000000000000, 0.000000000000000000, 1.000000000000000000 ) ) ;
#34326 = CARTESIAN_POINT ( 'NONE',  ( 13.62178482187499640, 196.5593750006145513, -23.59362340125807123 ) ) ;
#34327 = CARTESIAN_POINT ( 'NONE',  ( 13.56230152254411259, -5.196152422706632912, -8.812499998771039955 ) ) ;
#34328 = CYLINDRICAL_SURFACE ( 'NONE', #18806, 7.500000000000000000 ) ;
#34329 = EDGE_CURVE ( 'NONE', #22009, #13180, #13807, .T. ) ;
#34330 = CARTESIAN_POINT ( 'NONE',  ( -1.715153634034442431, 32.07731371789855501, 9.534712964251900402 ) ) ;
#34331 = CARTESIAN_POINT ( 'NONE',  ( 24.00000000000000000, -5.196152422706629359, -8.849999999999996092 ) ) ;
#34332 = ORIENTED_EDGE ( 'NONE', *, *, #751, .F. ) ;
#34333 = CARTESIAN_POINT ( 'NONE',  ( 21.00000000000000000, 240.0437500012290570, -6.928203230275506996 ) ) ;
#34334 = CARTESIAN_POINT ( 'NONE',  ( 10.49813415416005213, 65.42731371789855643, -7.228626920338837358 ) ) ;
#34335 = CARTESIAN_POINT ( 'NONE',  ( 13.44051670066911086, 5.407089921784862696, -8.371874999385548577 ) ) ;
#34336 = CARTESIAN_POINT ( 'NONE',  ( 15.24356964375000167, -3.323476615752272600, -10.11562499938547788 ) ) ;
#34337 = CARTESIAN_POINT ( 'NONE',  ( 11.48171059495408208, 38.11481371789854222, -4.944772684328420986 ) ) ;
#34338 = EDGE_LOOP ( 'NONE', ( #33737, #9738, #21351, #10097 ) ) ;
#34339 = CARTESIAN_POINT ( 'NONE',  ( 19.68408634441912142, -5.407089921784861808, -1.396874999385538940 ) ) ;
#34340 = AXIS2_PLACEMENT_3D ( 'NONE', #17041, #37112, #33722 ) ;
#34341 = CARTESIAN_POINT ( 'NONE',  ( 11.61527771782819940, 7.535186282101452804, -4.622313124798573369 ) ) ;
#34342 = ADVANCED_FACE ( 'NONE', ( #14243, #28447 ), #8923, .F. ) ;
#34343 = CARTESIAN_POINT ( 'NONE',  ( 31.23562490067698150, 7.209453229046482114, 166.9937279661931768 ) ) ;
#34344 = EDGE_CURVE ( 'NONE', #13979, #32302, #22474, .T. ) ;
#34345 = CARTESIAN_POINT ( 'NONE',  ( -38.31919563604516554, 216.5000000000000000, -0.1155267958017906493 ) ) ;
#34346 = CARTESIAN_POINT ( 'NONE',  ( 16.56230152254411436, 6.928203230275506996, -0.4499999987709982219 ) ) ;
#34347 =( NAMED_UNIT ( * ) PLANE_ANGLE_UNIT ( ) SI_UNIT ( $, .RADIAN. ) );
#34348 = CARTESIAN_POINT ( 'NONE',  ( -69.99330436395490551, 210.1155267958017134, -6.500000000000000888 ) ) ;
#34349 = CARTESIAN_POINT ( 'NONE',  ( -66.22544563604516554, 213.3788001182224718, 3.209657149897419348 ) ) ;
#34350 = CARTESIAN_POINT ( 'NONE',  ( -49.01413769728823411, 213.1499508600178672, 5.686928522499718142 ) ) ;
#34351 = CARTESIAN_POINT ( 'NONE',  ( -20.68320042480036491, 194.9994763866750134, -17.35526491262920246 ) ) ;
#34352 = ORIENTED_EDGE ( 'NONE', *, *, #7286, .T. ) ;
#34353 = CYLINDRICAL_SURFACE ( 'NONE', #5230, 27.00000000000000355 ) ;
#34354 = CARTESIAN_POINT ( 'NONE',  ( -11.08355503943118592, 16.83981371789855430, -10.83675517735179383 ) ) ;
#34355 = CARTESIAN_POINT ( 'NONE',  ( -38.12127896937850835, 218.5309553116392465, 2.162041339862725842 ) ) ;
#34356 = CARTESIAN_POINT ( 'NONE',  ( 8.962234695871762469, 6.960186282101432198, -8.715434833791931624 ) ) ;
#34357 = CARTESIAN_POINT ( 'NONE',  ( -12.53471296425194836, 49.22268628210144215, 2.311890736173176641 ) ) ;
#34358 = CARTESIAN_POINT ( 'NONE',  ( 22.56230152254412147, -3.464101615137755275, -4.312500000000036415 ) ) ;
#34359 = ORIENTED_EDGE ( 'NONE', *, *, #17481, .T. ) ;
#34360 = CARTESIAN_POINT ( 'NONE',  ( -8.927990412390661490, 11.27268628210142865, 13.04141134922759804 ) ) ;
#34361 = CARTESIAN_POINT ( 'NONE',  ( -26.99999999999999645, 196.1000000012290627, 15.58845726811991561 ) ) ;
#34362 = AXIS2_PLACEMENT_3D ( 'NONE', #35137, #26991, #23974 ) ;
#34363 = CARTESIAN_POINT ( 'NONE',  ( 13.62178482187501416, 197.3093750006145513, 23.59362340125806767 ) ) ;
#34364 = CARTESIAN_POINT ( 'NONE',  ( 36.87043443719270641, 3.464101615138096335, 162.5576162106535492 ) ) ;
#34365 = CARTESIAN_POINT ( 'NONE',  ( -7.234628195640289583, 198.5575961894323029, -27.00000000000001421 ) ) ;
#34366 = CARTESIAN_POINT ( 'NONE',  ( 0.000000000000000000, 200.0000000000000000, 0.000000000000000000 ) ) ;
#34367 = EDGE_CURVE ( 'NONE', #2166, #36568, #27727, .T. ) ;
#34368 = CARTESIAN_POINT ( 'NONE',  ( 26.99999999999999645, 246.2312500012290570, -7.347880794884117764E-16 ) ) ;
#34369 = CARTESIAN_POINT ( 'NONE',  ( 26.75643035624999655, 244.2343750006145342, -7.049594010296217766E-16 ) ) ;
#34370 = CARTESIAN_POINT ( 'NONE',  ( -8.710071997420207879, 97.91481371789856780, 3.796722387233182339 ) ) ;
#34371 = CARTESIAN_POINT ( 'NONE',  ( 18.12178482187499640, 242.5843750006145285, -4.985214923628404904 ) ) ;
#34372 = AXIS2_PLACEMENT_3D ( 'NONE', #8552, #32037, #385 ) ;
#34373 = ORIENTED_EDGE ( 'NONE', *, *, #16773, .F. ) ;
#34374 = CARTESIAN_POINT ( 'NONE',  ( -68.01413769728823411, 213.1499508600178672, 5.686928522499718142 ) ) ;
#34375 = CARTESIAN_POINT ( 'NONE',  ( -6.000000000000000888, -30.00000000000000000, -19.99999999999999289 ) ) ;
#34376 = CARTESIAN_POINT ( 'NONE',  ( 23.99999999999999645, 247.6562500012290400, -5.196152422706631135 ) ) ;
#34377 = ORIENTED_EDGE ( 'NONE', *, *, #14339, .F. ) ;
#34378 = CARTESIAN_POINT ( 'NONE',  ( 7.228626920338837358, 113.7273137178985820, 10.49813415416005036 ) ) ;
#34379 = CARTESIAN_POINT ( 'NONE',  ( 22.80587116629411071, -3.604726614523238837, -1.359374999385495775 ) ) ;
#34380 = CARTESIAN_POINT ( 'NONE',  ( 36.98316069593346356, 3.604726614523238837, 161.0514349962108156 ) ) ;
#34381 = CARTESIAN_POINT ( 'NONE',  ( 33.91126540609537443, -5.196152422706635576, 163.1552991495023548 ) ) ;
#34382 = CARTESIAN_POINT ( 'NONE',  ( -27.24356964374999990, 199.3718750006145513, -15.72908226750537786 ) ) ;
#34383 = EDGE_LOOP ( 'NONE', ( #9215, #23594, #29139, #4319 ) ) ;
#34384 = ORIENTED_EDGE ( 'NONE', *, *, #13611, .T. ) ;
#34385 = EDGE_LOOP ( 'NONE', ( #1139, #9214, #25838, #16299 ) ) ;
#34386 = CARTESIAN_POINT ( 'NONE',  ( 23.99999999999999645, 5.196152422706631135, -7.293749998770943321 ) ) ;
#34387 = CARTESIAN_POINT ( 'NONE',  ( 15.24356964374999990, 0.000000000000000000, -3.740624999385461003 ) ) ;
#34388 = CARTESIAN_POINT ( 'NONE',  ( 33.58116303054575269, 5.196152422706631135, 159.3822117317042455 ) ) ;
#34389 = CARTESIAN_POINT ( 'NONE',  ( 26.75643035624999655, 248.1718750006145342, -7.049594010296217766E-16 ) ) ;
#34390 = CARTESIAN_POINT ( 'NONE',  ( 8.715434833791931624, 55.26018628210144357, 8.962234695871760692 ) ) ;
#34391 = EDGE_CURVE ( 'NONE', #30763, #23933, #18612, .T. ) ;
#34392 = CARTESIAN_POINT ( 'NONE',  ( -44.45461230271182274, 208.1428034533958851, -6.469044688360754414 ) ) ;
#34393 = CARTESIAN_POINT ( 'NONE',  ( 15.53186252112518417, 224.5816999436668482, 2.477503916096319703 ) ) ;
#34394 = CLOSED_SHELL ( 'NONE', ( #21929, #17111, #29084, #21190, #15140, #8902, #21889, #21285, #30273, #37390, #15907, #2707, #27640, #11008, #2308, #9384, #10779, #10109, #33690, #31866, #2051, #20809, #9509, #34828, #20375, #25903 ) ) ;
#34395 = AXIS2_PLACEMENT_3D ( 'NONE', #28997, #6064, #31664 ) ;
#34396 = CARTESIAN_POINT ( 'NONE',  ( -43.06919563604516554, 214.5000000000000284, -0.1155267958017627827 ) ) ;
#34397 =( NAMED_UNIT ( * ) SI_UNIT ( $, .STERADIAN. ) SOLID_ANGLE_UNIT ( ) );
#34398 = CARTESIAN_POINT ( 'NONE',  ( 30.92921799263331906, -6.928203230275506996, 163.4914809813265606 ) ) ;
#34399 = CARTESIAN_POINT ( 'NONE',  ( -12.50000000000000355, 107.6898137178985735, 0.1745138560722786503 ) ) ;
#34400 = CARTESIAN_POINT ( 'NONE',  ( -32.38913769728823411, 206.8500491399821044, -5.686928522499717253 ) ) ;
#34401 =( BOUNDED_CURVE ( )  B_SPLINE_CURVE ( 2, ( #14844, #424, #11990, #23562, #35107, #9155, #20722 ),
 .UNSPECIFIED., .F., .F. ) 
 B_SPLINE_CURVE_WITH_KNOTS ( ( 3, 2, 2, 3 ),
 ( 0.000000000000000000, 0.007246376811594097168, 0.01449275362318819434, 0.02173913043478229237 ),
 .UNSPECIFIED. ) 
 CURVE ( )  GEOMETRIC_REPRESENTATION_ITEM ( )  RATIONAL_B_SPLINE_CURVE ( ( 1.000000000000000000, 0.8660254037844387076, 1.000000000000000000, 0.8660254037844387076, 1.000000000000000000, 0.8660254037844445918, 0.9999999999999941158 ) ) 
 REPRESENTATION_ITEM ( '' )  );
#34402 = CARTESIAN_POINT ( 'NONE',  ( -44.06622103062156270, 212.1620413398628671, 8.530955311639223382 ) ) ;
#34403 = CARTESIAN_POINT ( 'NONE',  ( 20.99999999999999645, 6.646953231504538984, -3.965624999385493510 ) ) ;
#34404 = CYLINDRICAL_SURFACE ( 'NONE', #5870, 5.999999999999994671 ) ;
#34405 = CARTESIAN_POINT ( 'NONE',  ( -13.23911966647199812, 71.75231371789854506, -8.632099005475788900 ) ) ;
#34406 = CARTESIAN_POINT ( 'NONE',  ( -36.93377896937850124, 208.3738570449995109, 6.530955311639247363 ) ) ;
#34407 = VERTEX_POINT ( 'NONE', #36007 ) ;
#34408 = CARTESIAN_POINT ( 'NONE',  ( 26.99999999999999645, 242.1437500012289945, 3.464101615137751278 ) ) ;
#34409 = CARTESIAN_POINT ( 'NONE',  ( -6.932735513423968321, 96.94768628210145778, -10.69584247140445221 ) ) ;
#34410 = CARTESIAN_POINT ( 'NONE',  ( 10.83675517735155225, 64.46018628210146062, 11.08355503943142573 ) ) ;
#34411 = CARTESIAN_POINT ( 'NONE',  ( 18.00000000000000355, 243.3250000000000171, 5.196152422706632912 ) ) ;
#34412 = CARTESIAN_POINT ( 'NONE',  ( 24.59746635921792546, -3.604726614523244610, 162.7561563650505150 ) ) ;
#34413 = CARTESIAN_POINT ( 'NONE',  ( -11.08355503943142573, 66.76018628210144357, 10.83675517735155402 ) ) ;
#34414 = EDGE_CURVE ( 'NONE', #9915, #13040, #15367, .T. ) ;
#34415 = CARTESIAN_POINT ( 'NONE',  ( 19.68408634441910721, -5.407089921784855591, -6.740624999385547156 ) ) ;
#34416 = CYLINDRICAL_SURFACE ( 'NONE', #32182, 5.999999999999998224 ) ;
#34417 = CARTESIAN_POINT ( 'NONE',  ( -66.23288769728823411, 203.5309553116391612, -1.857196546604028775 ) ) ;
#34418 = DIRECTION ( 'NONE',  ( 0.000000000000000000, 1.000000000000000000, 0.000000000000000000 ) ) ;
#34419 = CARTESIAN_POINT ( 'NONE',  ( -12.53471296425194836, 30.82268628210144001, 2.311890736173176641 ) ) ;
#34420 = CARTESIAN_POINT ( 'NONE',  ( 5.727106289114498080E-15, 196.9625000000000057, 31.17691453623979214 ) ) ;
#34421 = AXIS2_PLACEMENT_3D ( 'NONE', #22166, #16476, #13632 ) ;
#34422 = CARTESIAN_POINT ( 'NONE',  ( 15.06230152254410548, 0.000000000000000000, 10.00000000000000000 ) ) ;
#34423 = CARTESIAN_POINT ( 'NONE',  ( 9.534712964251941258, 17.02268628210144996, -1.715153634034235708 ) ) ;
#34424 = CARTESIAN_POINT ( 'NONE',  ( 26.75643035624999655, 248.2843750006145456, -7.049594010296217766E-16 ) ) ;
#34425 = VERTEX_POINT ( 'NONE', #26537 ) ;
#34426 = CARTESIAN_POINT ( 'NONE',  ( 26.99999999999999645, 3.464101615137755275, -3.787500000000015188 ) ) ;
#34427 = DIRECTION ( 'NONE',  ( 1.000000000000000000, 0.000000000000000000, 0.000000000000000000 ) ) ;
#34428 = CARTESIAN_POINT ( 'NONE',  ( 33.70166733926387082, -5.407089921784861808, 159.3622581591915548 ) ) ;
#34429 = CARTESIAN_POINT ( 'NONE',  ( 16.56230152254411081, -7.209453229046475009, -1.828124999385505989 ) ) ;
#34430 = CARTESIAN_POINT ( 'NONE',  ( 31.33857762179763995, -7.209453229046475009, 168.1704829533140355 ) ) ;
#34431 = CARTESIAN_POINT ( 'NONE',  ( 26.99999999999999645, 242.6125000000000114, -3.464101615137755275 ) ) ;
#34432 = CARTESIAN_POINT ( 'NONE',  ( 0.3500000000000065281, 244.5000000000000000, 5.000000000000000000 ) ) ;
#34433 = CARTESIAN_POINT ( 'NONE',  ( 2.311890736173175753, 65.32268628210144357, 12.53471296425194659 ) ) ;
#34434 = ORIENTED_EDGE ( 'NONE', *, *, #36268, .T. ) ;
#34435 = ORIENTED_EDGE ( 'NONE', *, *, #22237, .F. ) ;
#34436 = CARTESIAN_POINT ( 'NONE',  ( -1.909035429704832693E-15, 196.4000000012290457, -31.17691453623979214 ) ) ;
#34437 = DIRECTION ( 'NONE',  ( 0.000000000000000000, 0.000000000000000000, -1.000000000000000000 ) ) ;
#34438 = CARTESIAN_POINT ( 'NONE',  ( -8.927990412390371944, 44.72731371789853938, -13.04141134922778988 ) ) ;
#34439 = CARTESIAN_POINT ( 'NONE',  ( 15.24356964375000167, -3.323476615752272600, -9.215624999385486404 ) ) ;
#34440 = CARTESIAN_POINT ( 'NONE',  ( 26.75643035624999655, 243.7843750006145456, -7.049594010296217766E-16 ) ) ;
#34441 = CARTESIAN_POINT ( 'NONE',  ( -42.87872103062157692, 205.4690446883607535, 1.090244570138264368 ) ) ;
#34442 = CARTESIAN_POINT ( 'NONE',  ( 15.00000000000000000, 242.8562500012290286, 0.000000000000000000 ) ) ;
#34443 = EDGE_CURVE ( 'NONE', #805, #8055, #9304, .T. ) ;
#34444 = CARTESIAN_POINT ( 'NONE',  ( 36.97825818540390941, 3.604726614523243278, 160.9953990444431611 ) ) ;
#34445 = CARTESIAN_POINT ( 'NONE',  ( -9.465287035748106703, 15.40231371789854720, 2.064181346179061460 ) ) ;
#34446 = CARTESIAN_POINT ( 'NONE',  ( -69.20163769728823411, 215.6869285224996986, -3.149950860017881382 ) ) ;
#34447 = DIRECTION ( 'NONE',  ( 1.000000000000000000, 0.000000000000000000, 0.000000000000000000 ) ) ;
#34448 = CARTESIAN_POINT ( 'NONE',  ( 24.32002691557804397, 195.0000000000000284, -11.86068704861160938 ) ) ;
#34449 = CARTESIAN_POINT ( 'NONE',  ( -13.62178482187498396, 195.8843750006145399, 23.59362340125808188 ) ) ;
#34450 = CARTESIAN_POINT ( 'NONE',  ( -11.61527771782809282, 16.26481371789853370, -4.622313124798832717 ) ) ;
#34451 = EDGE_LOOP ( 'NONE', ( #15821, #9999 ) ) ;
#34452 = CARTESIAN_POINT ( 'NONE',  ( 0.1745138560725515708, 61.01018628210145067, -12.50000000000000355 ) ) ;
#34453 = CARTESIAN_POINT ( 'NONE',  ( 18.00000000000000355, 240.6250000000000000, 5.196152422706632912 ) ) ;
#34454 = DIRECTION ( 'NONE',  ( -0.000000000000000000, 1.000000000000000000, -0.000000000000000000 ) ) ;
#34455 = CARTESIAN_POINT ( 'NONE',  ( 33.75886329544200493, 5.407089921784857367, 160.0160109298142288 ) ) ;
#34456 = CARTESIAN_POINT ( 'NONE',  ( 15.00000000000000000, 0.000000000000000000, -2.193749998770949894 ) ) ;
#34457 =( BOUNDED_CURVE ( )  B_SPLINE_CURVE ( 2, ( #27283, #3780, #35620, #21243, #1313, #30320, #3600 ),
 .UNSPECIFIED., .F., .F. ) 
 B_SPLINE_CURVE_WITH_KNOTS ( ( 3, 2, 2, 3 ),
 ( 0.3695652173913039351, 0.3768115942028982257, 0.3840579710144925163, 0.3913043478260868069 ),
 .UNSPECIFIED. ) 
 CURVE ( )  GEOMETRIC_REPRESENTATION_ITEM ( )  RATIONAL_B_SPLINE_CURVE ( ( 1.000000000000007105, 0.8660254037844313801, 1.000000000000000000, 0.8660254037844387076, 1.000000000000000000, 0.8660254037844418162, 0.9999999999999968914 ) ) 
 REPRESENTATION_ITEM ( '' )  );
#34458 = CARTESIAN_POINT ( 'NONE',  ( 10.31873187879410736, 0.000000000000000000, -7.846874999385494931 ) ) ;
#34459 = CARTESIAN_POINT ( 'NONE',  ( -7.234628195640328663, 197.0549038117967484, 26.99999999999999289 ) ) ;
#34460 = CARTESIAN_POINT ( 'NONE',  ( -9.534712964251941258, 76.82268628210144357, 1.715153634034234154 ) ) ;
#34461 = LINE ( 'NONE', #2990, #35224 ) ;
#34462 = CARTESIAN_POINT ( 'NONE',  ( -12.53471296425194836, 104.4226862821014379, 2.311890736173176641 ) ) ;
#34463 = CARTESIAN_POINT ( 'NONE',  ( -13.50000000000000533, 197.2250000000000227, -23.38268590217984411 ) ) ;
#34464 = CARTESIAN_POINT ( 'NONE',  ( 2.999999999999997335, 244.5000000000000000, -10.00000000000000000 ) ) ;
#34465 = ORIENTED_EDGE ( 'NONE', *, *, #19913, .T. ) ;
#34466 = CARTESIAN_POINT ( 'NONE',  ( 24.63505227327785718, 3.604726614523236616, 163.1857653286025709 ) ) ;
#34467 = CARTESIAN_POINT ( 'NONE',  ( 23.87821517812499650, 4.985214923628404904, -7.040624999385459049 ) ) ;
#34468 = CARTESIAN_POINT ( 'NONE',  ( 27.24356964375000700, 196.4468750006145399, 15.72908226750537075 ) ) ;
#34469 = CARTESIAN_POINT ( 'NONE',  ( 37.48811928047767594, 3.604726614523243278, 166.8231380282798568 ) ) ;
#34470 = CARTESIAN_POINT ( 'NONE',  ( 31.27239372959508756, -6.928203230275514990, 167.4139976038384532 ) ) ;
#34471 = CYLINDRICAL_SURFACE ( 'NONE', #406, 5.999999999999999112 ) ;
#34472 = CARTESIAN_POINT ( 'NONE',  ( 26.75643035624999655, 241.5343750006145456, -7.049594010296217766E-16 ) ) ;
#34473 = CARTESIAN_POINT ( 'NONE',  ( -13.62178482187498396, 198.5281250006145228, 23.59362340125808188 ) ) ;
#34474 = CARTESIAN_POINT ( 'NONE',  ( -4.622313124798826500, 124.3648137178985706, 11.61527771782809637 ) ) ;
#34475 = CARTESIAN_POINT ( 'NONE',  ( 11.48171059495397728, 119.0851862821014606, 4.944772684328674117 ) ) ;
#34477 = ORIENTED_EDGE ( 'NONE', *, *, #30400, .F. ) ;
#34476 = ORIENTED_EDGE ( 'NONE', *, *, #6126, .F. ) ;
#34478 = CARTESIAN_POINT ( 'NONE',  ( -13.62178482187498396, 197.6281250006145171, 23.59362340125808188 ) ) ;
#34479 = CARTESIAN_POINT ( 'NONE',  ( 15.24356964375000167, 241.2343750006145058, 3.323476615752272600 ) ) ;
#34480 = CARTESIAN_POINT ( 'NONE',  ( 16.56230152254411436, -6.928203230275514990, -2.137500000000051692 ) ) ;
#34481 = EDGE_CURVE ( 'NONE', #22146, #2118, #35630, .T. ) ;
#34482 = CARTESIAN_POINT ( 'NONE',  ( -6.092822981423666739, 91.01481371789856212, -14.25334919248795096 ) ) ;
#34483 = CARTESIAN_POINT ( 'NONE',  ( -6.932735513423968321, 96.94768628210145778, -10.69584247140445221 ) ) ;
#34484 = CARTESIAN_POINT ( 'NONE',  ( 18.12178482187500350, -4.985214923628407568, -2.428124999385494753 ) ) ;
#34485 = CARTESIAN_POINT ( 'NONE',  ( -13.50000000000000533, 196.4375000012290400, -23.38268590217984411 ) ) ;
#34486 = EDGE_CURVE ( 'NONE', #28877, #32302, #12133, .T. ) ;
#34487 = CARTESIAN_POINT ( 'NONE',  ( 8.715434833791931624, 110.4601862821014606, 8.962234695871760692 ) ) ;
#34488 = CARTESIAN_POINT ( 'NONE',  ( 19.68408634441910721, 5.407089921784857367, -2.090624999385559679 ) ) ;
#34489 = EDGE_CURVE ( 'NONE', #3136, #9546, #5727, .T. ) ;
#34490 = CARTESIAN_POINT ( 'NONE',  ( 26.75643035624999655, 245.4718750006145171, -7.049594010296217766E-16 ) ) ;
#34491 = CARTESIAN_POINT ( 'NONE',  ( 21.00000000000000000, 240.2125000000000057, 5.999999999999998224 ) ) ;
#34492 = CARTESIAN_POINT ( 'NONE',  ( -8.962234695871760692, 112.7601862821014720, 8.715434833791933400 ) ) ;
#34493 = CARTESIAN_POINT ( 'NONE',  ( 13.56230152254410548, 5.196152422706630247, -3.562499998771007093 ) ) ;
#34494 = CARTESIAN_POINT ( 'NONE',  ( -39.11830436395489841, 209.8844732041982581, 6.500000000000000888 ) ) ;
#34495 = DIRECTION ( 'NONE',  ( -0.000000000000000000, -1.000000000000000000, -0.000000000000000000 ) ) ;
#34496 = CARTESIAN_POINT ( 'NONE',  ( 20.99999999999999645, 249.2687500012290513, 5.999999999999998224 ) ) ;
#34497 = CARTESIAN_POINT ( 'NONE',  ( -15.53471296425195369, 104.4226862821014521, 2.908627838312118019 ) ) ;
#34498 = CARTESIAN_POINT ( 'NONE',  ( -10.69584247140444866, 21.04768628210144854, 6.932735513423972762 ) ) ;
#34499 = CARTESIAN_POINT ( 'NONE',  ( 15.00000000000000000, 0.000000000000000000, -0.4500000000000059508 ) ) ;
#34500 =( BOUNDED_CURVE ( )  B_SPLINE_CURVE ( 2, ( #234, #12171, #34730, #29033, #32074, #9341, #6103, #17686, #26573 ),
 .UNSPECIFIED., .F., .F. ) 
 B_SPLINE_CURVE_WITH_KNOTS ( ( 3, 2, 2, 2, 3 ),
 ( 0.7282608695652174058, 0.7318840579710145233, 0.7391304347826086474, 0.7463768115942028825, 0.7500000000000000000 ),
 .UNSPECIFIED. ) 
 CURVE ( )  GEOMETRIC_REPRESENTATION_ITEM ( )  RATIONAL_B_SPLINE_CURVE ( ( 0.9330127018922194093, 0.9330127018922194093, 1.000000000000000000, 0.8660254037844387076, 1.000000000000000000, 0.8660254037844387076, 1.000000000000000000, 0.9330127018922194093, 0.9330127018922194093 ) ) 
 REPRESENTATION_ITEM ( '' )  );
#34501 = FACE_OUTER_BOUND ( 'NONE', #3523, .T. ) ;
#34502 = CARTESIAN_POINT ( 'NONE',  ( 1.715153634034233487, 138.9226862821014663, 9.534712964251941258 ) ) ;
#34503 = CARTESIAN_POINT ( 'NONE',  ( 24.00000000000000000, 245.7062500012290513, 5.196152422706629359 ) ) ;
#34505 = ORIENTED_EDGE ( 'NONE', *, *, #33218, .F. ) ;
#34504 = VECTOR ( 'NONE', #13072, 1000.000000000000000 ) ;
#34506 = CARTESIAN_POINT ( 'NONE',  ( 34.53019161875872101, -5.407089921784855591, 168.8323340079261925 ) ) ;
#34507 = CARTESIAN_POINT ( 'NONE',  ( -0.1745138560725182642, 65.61018628210146630, 9.500000000000005329 ) ) ;
#34508 = CARTESIAN_POINT ( 'NONE',  ( 18.12178482187500350, -4.985214923628407568, -0.5156249993854555846 ) ) ;
#34509 = CARTESIAN_POINT ( 'NONE',  ( 20.99999999999999645, 6.928203230275506996, -5.062500000000007994 ) ) ;
#34510 = DIRECTION ( 'NONE',  ( 1.000000000000000000, 0.000000000000000000, 0.000000000000000000 ) ) ;
#34511 = CARTESIAN_POINT ( 'NONE',  ( -13.62178482187498396, 194.9843750006145626, 23.59362340125808188 ) ) ;
#34512 = DIRECTION ( 'NONE',  ( 0.000000000000000000, 1.000000000000000000, 0.000000000000000000 ) ) ;
#34513 = CARTESIAN_POINT ( 'NONE',  ( -12.50000000000000355, 5.000000000000004441, -1.353084311261909534E-13 ) ) ;
#34514 = CARTESIAN_POINT ( 'NONE',  ( 8.152565276336593669, 30.35231371789855359, 5.233372021372610483 ) ) ;
#34515 = DIRECTION ( 'NONE',  ( -1.000000000000000000, 0.000000000000000000, 0.000000000000000000 ) ) ;
#34516 = ORIENTED_EDGE ( 'NONE', *, *, #15497, .F. ) ;
#34517 = ORIENTED_EDGE ( 'NONE', *, *, #24524, .F. ) ;
#34518 = CARTESIAN_POINT ( 'NONE',  ( 23.87821517812499650, 248.6968750006145115, -4.985214923628404904 ) ) ;
#34519 = AXIS2_PLACEMENT_3D ( 'NONE', #25627, #25443, #28286 ) ;
#34520 = CARTESIAN_POINT ( 'NONE',  ( 10.69584247140429589, 48.75231371789855217, 6.932735513424201024 ) ) ;
#34521 = CARTESIAN_POINT ( 'NONE',  ( 10.31873187879411091, 3.604726614523240613, -9.234374999385533300 ) ) ;
#34522 = CARTESIAN_POINT ( 'NONE',  ( 21.00000000000000000, 6.646953231504538984, -0.2531249993854407521 ) ) ;
#34523 = CARTESIAN_POINT ( 'NONE',  ( 2.311890736173452865, 9.077313717898549683, -12.53471296425189152 ) ) ;
#34524 =( BOUNDED_CURVE ( )  B_SPLINE_CURVE ( 2, ( #17853, #11083, #11271, #31360, #32426, #11961, #31182 ),
 .UNSPECIFIED., .F., .F. ) 
 B_SPLINE_CURVE_WITH_KNOTS ( ( 3, 2, 2, 3 ),
 ( 0.06521739130434729692, 0.07246376811594164302, 0.07971014492753598912, 0.08695652173913033522 ),
 .UNSPECIFIED. ) 
 CURVE ( )  GEOMETRIC_REPRESENTATION_ITEM ( )  RATIONAL_B_SPLINE_CURVE ( ( 1.000000000000009770, 0.8660254037844290487, 1.000000000000000000, 0.8660254037844387076, 1.000000000000000000, 0.8660254037844404840, 0.9999999999999982236 ) ) 
 REPRESENTATION_ITEM ( '' )  );
#34525 = ORIENTED_EDGE ( 'NONE', *, *, #26272, .F. ) ;
#34526 = CARTESIAN_POINT ( 'NONE',  ( 10.31873187879410914, 0.000000000000000000, -1.996874999385528371 ) ) ;
#34527 = CARTESIAN_POINT ( 'NONE',  ( 18.00000000000000000, 245.9312500012290457, -5.196152422706630247 ) ) ;
#34528 = CARTESIAN_POINT ( 'NONE',  ( 24.94717877699287811, 0.000000000000000000, 166.7533875911436780 ) ) ;
#34529 = AXIS2_PLACEMENT_3D ( 'NONE', #11762, #22961, #14983 ) ;
#34530 = CARTESIAN_POINT ( 'NONE',  ( -36.93377896937850124, 208.3738570449995109, 6.530955311639247363 ) ) ;
#34531 = CARTESIAN_POINT ( 'NONE',  ( 22.56230152254412502, 7.347880794884125653E-16, -3.375000000000044409 ) ) ;
#34532 = CARTESIAN_POINT ( 'NONE',  ( -26.99693289488239500, 195.0000000000001137, 2.389390116437581479 ) ) ;
#34533 = CARTESIAN_POINT ( 'NONE',  ( -53.36086230271183695, 212.1499508600178387, -3.954877714930852495 ) ) ;
#34534 = CARTESIAN_POINT ( 'NONE',  ( -47.23288769728823411, 203.5309553116391612, -1.857196546604028775 ) ) ;
#34535 = CARTESIAN_POINT ( 'NONE',  ( 37.60741370336351252, 7.646167579472015790E-16, 168.1866795212929446 ) ) ;
#34536 = ORIENTED_EDGE ( 'NONE', *, *, #14801, .F. ) ;
#34537 = FACE_OUTER_BOUND ( 'NONE', #27953, .T. ) ;
#34538 = CARTESIAN_POINT ( 'NONE',  ( 18.00000000000000355, -5.196152422706632912, -7.124999999999992895 ) ) ;
#34539 = CARTESIAN_POINT ( 'NONE',  ( -6.092822981423666739, 26.61481371789854933, -14.25334919248795096 ) ) ;
#34540 = CARTESIAN_POINT ( 'NONE',  ( -63.65997103062157692, 217.3034525342668815, 4.350049139982096413 ) ) ;
#34541 = CARTESIAN_POINT ( 'NONE',  ( 10.69584247140445221, 16.44768628210144001, -6.932735513423970097 ) ) ;
#34542 = CARTESIAN_POINT ( 'NONE',  ( -12.46528703574805697, 49.79768628210145209, -2.660918448318280838 ) ) ;
#34543 = CARTESIAN_POINT ( 'NONE',  ( 13.56230152254410548, 5.196152422706636465, -4.575000000000050804 ) ) ;
#34544 = ORIENTED_EDGE ( 'NONE', *, *, #21548, .T. ) ;
#34545 = CARTESIAN_POINT ( 'NONE',  ( 22.56230152254410370, 7.347880794884117764E-16, -5.512499998771014376 ) ) ;
#34546 = CARTESIAN_POINT ( 'NONE',  ( -13.62178482187500528, 195.7343750006145626, -23.59362340125807123 ) ) ;
#34547 = DIRECTION ( 'NONE',  ( 0.000000000000000000, -1.000000000000000000, 0.000000000000000000 ) ) ;
#34548 = FACE_OUTER_BOUND ( 'NONE', #16263, .T. ) ;
#34549 = DIRECTION ( 'NONE',  ( 0.000000000000000000, 0.000000000000000000, 1.000000000000000000 ) ) ;
#34550 = CYLINDRICAL_SURFACE ( 'NONE', #29923, 5.999999999999998224 ) ;
#34551 = CARTESIAN_POINT ( 'NONE',  ( 21.00000000000000000, 245.4718750006145456, 6.646953231504538984 ) ) ;
#34552 = CARTESIAN_POINT ( 'NONE',  ( 8.710071997420211432, 102.5148137178985621, -3.796722387233181895 ) ) ;
#34553 = CARTESIAN_POINT ( 'NONE',  ( 23.87821517812500005, 242.8093750006145228, 4.985214923628404016 ) ) ;
#34554 = AXIS2_PLACEMENT_3D ( 'NONE', #31461, #32015, #31829 ) ;
#34555 = ORIENTED_EDGE ( 'NONE', *, *, #26990, .T. ) ;
#34556 = CARTESIAN_POINT ( 'NONE',  ( -53.96205436395489130, 214.6737587650352168, 4.842901733360204908 ) ) ;
#34557 = CARTESIAN_POINT ( 'NONE',  ( -7.234628195640263826, 195.8575961894323711, -27.00000000000003553 ) ) ;
#34558 = CARTESIAN_POINT ( 'NONE',  ( 15.00000000000000000, 246.4187500012290286, -3.464101615137752166 ) ) ;
#34559 = ORIENTED_EDGE ( 'NONE', *, *, #7804, .T. ) ;
#34560 = CARTESIAN_POINT ( 'NONE',  ( 11.61527771782809637, 94.46481371789855075, 4.622313124798827388 ) ) ;
#34561 = CARTESIAN_POINT ( 'NONE',  ( 10.31873187879411091, -3.604726614523244610, -1.059374999385519933 ) ) ;
#34562 = CARTESIAN_POINT ( 'NONE',  ( 24.52392870127459545, -3.604726614523240613, 161.9156170885356403 ) ) ;
#34563 = CARTESIAN_POINT ( 'NONE',  ( 26.75643035624999655, -3.323476615752267715, -1.865624999385470772 ) ) ;
#34564 = CARTESIAN_POINT ( 'NONE',  ( -8.715434833792127023, 60.53981371789856070, 8.962234695871568846 ) ) ;
#34565 = CARTESIAN_POINT ( 'NONE',  ( 27.24356964374999635, 199.2218750006145456, -15.72908226750539029 ) ) ;
#34566 = ORIENTED_EDGE ( 'NONE', *, *, #34344, .T. ) ;
#34567 = ORIENTED_EDGE ( 'NONE', *, *, #7462, .T. ) ;
#34568 = ORIENTED_EDGE ( 'NONE', *, *, #1070, .T. ) ;
#34569 = CARTESIAN_POINT ( 'NONE',  ( 15.00000000000000178, -3.464101615137757051, -6.656249998770961795 ) ) ;
#34570 = CARTESIAN_POINT ( 'NONE',  ( 20.99999999999999645, -6.646953231504538984, -1.828124999385473792 ) ) ;
#34571 = CARTESIAN_POINT ( 'NONE',  ( 9.184850993605147944E-16, 143.0000000000000000, -7.500000000000000000 ) ) ;
#34572 = CARTESIAN_POINT ( 'NONE',  ( 21.00000000000000000, 247.3843750006145399, -6.646953231504538984 ) ) ;
#34573 = CARTESIAN_POINT ( 'NONE',  ( -8.715434833791929847, 50.66018628210144925, -8.962234695871762469 ) ) ;
#34574 = CARTESIAN_POINT ( 'NONE',  ( -56.13169563604517265, 210.1155267958017703, 6.500000000000000888 ) ) ;
#34575 = SURFACE_STYLE_USAGE ( .BOTH. , #25860 ) ;
#34576 = CARTESIAN_POINT ( 'NONE',  ( -47.22544563604517265, 213.3788001182224718, 3.209657149897419348 ) ) ;
#34577 = SURFACE_SIDE_STYLE ('',( #5951 ) ) ;
#34578 = CARTESIAN_POINT ( 'NONE',  ( 27.76741185964712244, 5.196152422706630247, 161.7730112471121799 ) ) ;
#34579 = CARTESIAN_POINT ( 'NONE',  ( 10.69584247140429589, 103.9523137178985621, 6.932735513424201024 ) ) ;
#34580 = CARTESIAN_POINT ( 'NONE',  ( -58.71205436395490551, 213.2096571498974242, 3.378800118222489601 ) ) ;
#34581 = CARTESIAN_POINT ( 'NONE',  ( -41.88913769728823411, 205.8500491399820760, -7.418979330068584233 ) ) ;
#34582 = CARTESIAN_POINT ( 'NONE',  ( 20.99999999999999645, -6.646953231504538984, -5.090624999385466865 ) ) ;
#34583 = CARTESIAN_POINT ( 'NONE',  ( 19.56230152254412147, -5.196152422706635576, -5.250000000000060396 ) ) ;
#34584 = CARTESIAN_POINT ( 'NONE',  ( -15.46528703574811736, 79.80231371789852801, 3.257655550456946436 ) ) ;
#34585 = CARTESIAN_POINT ( 'NONE',  ( -36.14211230271182984, 203.5309553116391612, 1.857196546604092280 ) ) ;
#34586 = ORIENTED_EDGE ( 'NONE', *, *, #8705, .T. ) ;
#34587 = CARTESIAN_POINT ( 'NONE',  ( 20.99999999999999289, 242.2937500012290570, -5.999999999999997335 ) ) ;
#34588 = CARTESIAN_POINT ( 'NONE',  ( -2.311890736173176641, 106.7226862821014635, -12.53471296425194836 ) ) ;
#34589 = CARTESIAN_POINT ( 'NONE',  ( 6.092822981423978490, 43.18518628210144072, -14.25334919248782306 ) ) ;
#34590 = CARTESIAN_POINT ( 'NONE',  ( 26.99999999999962341, 3.464101615137969770, -5.981249998770948650 ) ) ;
#34591 = CARTESIAN_POINT ( 'NONE',  ( 34.01542801315541453, -5.407089921784861808, 162.9485590723218422 ) ) ;
#34592 = CARTESIAN_POINT ( 'NONE',  ( -11.08355503943142573, 75.96018628210144641, 10.83675517735155402 ) ) ;
#34593 = CARTESIAN_POINT ( 'NONE',  ( 10.31873187879411091, 0.000000000000000000, -9.140624999385559946 ) ) ;
#34594 = CARTESIAN_POINT ( 'NONE',  ( 22.56230152254412147, 7.347880794884125653E-16, -8.775000000000032330 ) ) ;
#34595 = CARTESIAN_POINT ( 'NONE',  ( -47.82663769728823411, 204.3130714775002730, 3.149950860017883603 ) ) ;
#34596 = EDGE_CURVE ( 'NONE', #34054, #972, #26323, .T. ) ;
#34597 = CARTESIAN_POINT ( 'NONE',  ( 10.83228649186779791, 2.189148559480569300, -9.999999999999998224 ) ) ;
#34598 = CARTESIAN_POINT ( 'NONE',  ( 12.50000000000000355, 44.91018628210144215, 0.1745138560725507937 ) ) ;
#34599 = CARTESIAN_POINT ( 'NONE',  ( 13.49999999999999645, 196.2500000000000000, -23.38268590217984766 ) ) ;
#34600 = CARTESIAN_POINT ( 'NONE',  ( 5.438367727407757144E-14, 197.7500000012290400, -27.00000000000000000 ) ) ;
#34601 = CARTESIAN_POINT ( 'NONE',  ( 0.1745138560725194299, 5.810186282101448718, -9.500000000000005329 ) ) ;
#34602 = CARTESIAN_POINT ( 'NONE',  ( 18.12178482187500350, 248.1343750006145399, 4.985214923628407568 ) ) ;
#34603 = ORIENTED_EDGE ( 'NONE', *, *, #8492, .F. ) ;
#34604 = CARTESIAN_POINT ( 'NONE',  ( 18.00000000000000000, 5.196152422706630247, -4.574999999999995737 ) ) ;
#34605 = DIRECTION ( 'NONE',  ( 0.8083506638593009885, 0.5887012860850800999, 0.000000000000000000 ) ) ;
#34606 = CARTESIAN_POINT ( 'NONE',  ( 33.74088742350031822, -5.407089921784861808, 159.8105457733328478 ) ) ;
#34607 = CARTESIAN_POINT ( 'NONE',  ( 22.80587116629411781, 3.604726614523238837, -4.378124999385524241 ) ) ;
#34608 = CARTESIAN_POINT ( 'NONE',  ( 31.41701779027052766, -7.209453229046475009, 169.0670581815966216 ) ) ;
#34609 = CARTESIAN_POINT ( 'NONE',  ( 21.00000000000000000, 240.6625000000000227, 6.928203230275506996 ) ) ;
#34610 = CARTESIAN_POINT ( 'NONE',  ( 0.000000000000000000, 141.0000000000000000, 0.000000000000000000 ) ) ;
#34611 = EDGE_CURVE ( 'NONE', #483, #7130, #30210, .T. ) ;
#34612 = CARTESIAN_POINT ( 'NONE',  ( -12.50000000000000355, 67.91018628210144925, -0.1745138560725492671 ) ) ;
#34613 = EDGE_LOOP ( 'NONE', ( #36452, #33030, #26286, #861 ) ) ;
#34614 = EDGE_LOOP ( 'NONE', ( #10059, #860, #28371, #10972 ) ) ;
#34615 = CARTESIAN_POINT ( 'NONE',  ( -1.909035429704832693E-15, 195.5000000012290400, -31.17691453623979214 ) ) ;
#34616 = CARTESIAN_POINT ( 'NONE',  ( 26.99999999999999645, 7.347880794884117764E-16, -5.118749998770960374 ) ) ;
#34617 = CARTESIAN_POINT ( 'NONE',  ( 14.25334919248795451, 38.11481371789853512, -6.092822981423661410 ) ) ;
#34618 = CARTESIAN_POINT ( 'NONE',  ( 19.00081547855239350, 5.492723509887031952, -10.23957780870842882 ) ) ;
#34619 = CARTESIAN_POINT ( 'NONE',  ( 15.24356964375000167, 240.8968750006145001, 3.323476615752272600 ) ) ;
#34620 = CARTESIAN_POINT ( 'NONE',  ( -41.29538769728824121, 211.3212981617418222, -4.469044688360751749 ) ) ;
#34621 = EDGE_CURVE ( 'NONE', #11581, #16861, #26771, .T. ) ;
#34622 = CARTESIAN_POINT ( 'NONE',  ( 19.39230484541323918, 242.7638461906614396, -5.999999999999987566 ) ) ;
#34623 = CARTESIAN_POINT ( 'NONE',  ( 24.51575785039200284, 0.000000000000000000, 161.8222238355895399 ) ) ;
#34624 = CARTESIAN_POINT ( 'NONE',  ( -6.594114490232462877, 23.73981371789854222, 6.840914352311949109 ) ) ;
#34625 = CARTESIAN_POINT ( 'NONE',  ( 19.68408634441910365, 5.407089921784857367, -9.740624999385548932 ) ) ;
#34626 = PRODUCT_CONTEXT ( 'NONE', #19249, 'mechanical' ) ;
#34627 = CARTESIAN_POINT ( 'NONE',  ( 17.12995869703641816, 195.0000000000000284, 21.16104912388787795 ) ) ;
#34628 = CARTESIAN_POINT ( 'NONE',  ( 27.24356964375000700, 196.4468750006145115, 15.72908226750537075 ) ) ;
#34629 = CARTESIAN_POINT ( 'NONE',  ( 0.1745138560722461762, 132.9898137178985564, 15.50000000000000533 ) ) ;
#34630 = EDGE_LOOP ( 'NONE', ( #3840, #25234, #20247, #7778 ) ) ;
#34631 = CARTESIAN_POINT ( 'NONE',  ( -8.962234695871760692, 48.36018628210145209, 8.715434833791933400 ) ) ;
#34632 = CARTESIAN_POINT ( 'NONE',  ( 22.56230152254410370, 7.347880794884117764E-16, -10.01249999877101793 ) ) ;
#34633 = CARTESIAN_POINT ( 'NONE',  ( 10.49999999999999645, 244.5000000000000000, 2.500000000000000000 ) ) ;
#34634 = CARTESIAN_POINT ( 'NONE',  ( 27.54558899987776144, 5.407089921784856479, 160.6348884818688418 ) ) ;
#34635 = CARTESIAN_POINT ( 'NONE',  ( 15.00000000000000178, -3.464101615137757051, -2.606249998770968190 ) ) ;
#34636 = CARTESIAN_POINT ( 'NONE',  ( 10.31873187879410736, 3.604726614523240613, -7.884374999385513227 ) ) ;
#34637 = LINE ( 'NONE', #37293, #25805 ) ;
#34638 = CARTESIAN_POINT ( 'NONE',  ( 8.152565276336714462, 80.84768628210143504, -5.233372021372432847 ) ) ;
#34639 = FACE_OUTER_BOUND ( 'NONE', #6791, .T. ) ;
#34640 = LINE ( 'NONE', #26671, #9334 ) ;
#34641 = CARTESIAN_POINT ( 'NONE',  ( -6.932735513423968321, 96.94768628210145778, -10.69584247140445221 ) ) ;
#34642 = DIRECTION ( 'NONE',  ( 0.000000000000000000, 0.000000000000000000, 1.000000000000000000 ) ) ;
#34643 = CARTESIAN_POINT ( 'NONE',  ( -1.045839947578415010E-13, 195.1625000000000512, 27.00000000000000355 ) ) ;
#34644 = ORIENTED_EDGE ( 'NONE', *, *, #30417, .F. ) ;
#34645 = CARTESIAN_POINT ( 'NONE',  ( 33.86345018673919327, -5.407089921784855591, 161.2114445675243530 ) ) ;
#34646 = CARTESIAN_POINT ( 'NONE',  ( 23.87821517812500005, -4.985214923628404016, -7.640624999385475569 ) ) ;
#34648 = EDGE_CURVE ( 'NONE', #2079, #3146, #9623, .T. ) ;
#34647 = CARTESIAN_POINT ( 'NONE',  ( 27.24356964374999279, 196.5218750006145569, -15.72908226750539207 ) ) ;
#34649 = CARTESIAN_POINT ( 'NONE',  ( 31.21601485855875779, -7.209453229046482114, 166.7695841591225587 ) ) ;
#34650 = CARTESIAN_POINT ( 'NONE',  ( 37.25936693920468201, 7.347880794884125653E-16, 167.0031350508878631 ) ) ;
#34651 = CARTESIAN_POINT ( 'NONE',  ( 20.99999999999999645, 185.0294372515228645, -5.999999999999999112 ) ) ;
#34652 = CARTESIAN_POINT ( 'NONE',  ( 18.00000000000000355, 249.1750000000000114, 5.196152422706632912 ) ) ;
#34653 = CARTESIAN_POINT ( 'NONE',  ( -13.62178482187500528, 197.9281250006145569, -23.59362340125807123 ) ) ;
#34654 = CARTESIAN_POINT ( 'NONE',  ( 11.61527771782809637, 122.0648137178985735, 4.622313124798827388 ) ) ;
#34655 = CARTESIAN_POINT ( 'NONE',  ( 8.715434833791931624, 128.8601862821014663, 8.962234695871760692 ) ) ;
#34657 = ORIENTED_EDGE ( 'NONE', *, *, #16103, .T. ) ;
#34656 = ORIENTED_EDGE ( 'NONE', *, *, #37146, .T. ) ;
#34658 = CARTESIAN_POINT ( 'NONE',  ( 5.778771075727756162E-15, 199.0156250006145342, 31.45816453501075927 ) ) ;
#34659 = CARTESIAN_POINT ( 'NONE',  ( 15.24356964374999990, 242.9593750006145001, -3.323476615752268604 ) ) ;
#34660 = CARTESIAN_POINT ( 'NONE',  ( 19.39230484541326049, 243.6075961894323143, -5.999999999999997335 ) ) ;
#34661 = EDGE_CURVE ( 'NONE', #35593, #24310, #29759, .T. ) ;
#34662 = CARTESIAN_POINT ( 'NONE',  ( -14.25334919248795096, 97.91481371789856780, 6.092822981423662299 ) ) ;
#34663 = AXIS2_PLACEMENT_3D ( 'NONE', #16222, #4643, #15661 ) ;
#34664 = CARTESIAN_POINT ( 'NONE',  ( 23.87821517812499650, 4.985214923628404904, -3.553124999385481875 ) ) ;
#34665 = PRODUCT_DEFINITION_SHAPE ( 'NONE', 'NONE',  #13673 ) ;
#34666 = CARTESIAN_POINT ( 'NONE',  ( -27.00000000000000355, 197.3750000012290400, -15.58845726811989429 ) ) ;
#34667 = CARTESIAN_POINT ( 'NONE',  ( 5.233372021372610483, 83.25231371789854506, -8.152565276336593669 ) ) ;
#34668 = CARTESIAN_POINT ( 'NONE',  ( 16.56230152254411081, 7.209453229046475009, -2.953124999385511096 ) ) ;
#34669 = CARTESIAN_POINT ( 'NONE',  ( 20.99999999999999645, 241.9843750006145058, -6.646953231504538984 ) ) ;
#34670 = CARTESIAN_POINT ( 'NONE',  ( 11.61527771782809637, 57.66481371789855359, 4.622313124798827388 ) ) ;
#34671 = VECTOR ( 'NONE', #32175, 1000.000000000000000 ) ;
#34672 = CARTESIAN_POINT ( 'NONE',  ( 20.99999999999997513, 246.7937500012290286, -5.999999999999999112 ) ) ;
#34673 = CARTESIAN_POINT ( 'NONE',  ( -12.53471296425194836, 104.4226862821014379, 2.311890736173176641 ) ) ;
#34674 = CARTESIAN_POINT ( 'NONE',  ( 22.56230152254410726, 7.347880794884117764E-16, -3.262499998771012599 ) ) ;
#34675 = CARTESIAN_POINT ( 'NONE',  ( -36.94122103062157692, 208.3738570449993404, -6.530955311639226935 ) ) ;
#34676 = CARTESIAN_POINT ( 'NONE',  ( 0.000000000000000000, -20.00000000000000000, 0.000000000000000000 ) ) ;
#34677 = DIRECTION ( 'NONE',  ( -0.000000000000000000, -1.000000000000000000, -0.000000000000000000 ) ) ;
#34678 = CARTESIAN_POINT ( 'NONE',  ( 6.092822981423978490, 107.5851862821014748, -14.25334919248782306 ) ) ;
#34679 = CARTESIAN_POINT ( 'NONE',  ( -2.311890736173176641, 23.92268628210143788, -12.53471296425194659 ) ) ;
#34680 = CARTESIAN_POINT ( 'NONE',  ( 22.56230152254289578, 3.464101615138464041, -8.287500000000052935 ) ) ;
#34681 = PLANE ( 'NONE',  #1193 ) ;
#34682 = CARTESIAN_POINT ( 'NONE',  ( -9.500000000000005329, 132.3101862821014549, -0.1745138560725176813 ) ) ;
#34683 = DIRECTION ( 'NONE',  ( -1.000000000000000000, 0.000000000000000000, -2.057406622567553763E-16 ) ) ;
#34684 = CARTESIAN_POINT ( 'NONE',  ( 18.12178482187499640, 243.3718750006145228, -4.985214923628404904 ) ) ;
#34685 = VERTEX_POINT ( 'NONE', #12522 ) ;
#34686 = CARTESIAN_POINT ( 'NONE',  ( 37.56492527877403376, -3.604726614523235284, 167.7010346059732058 ) ) ;
#34687 = CARTESIAN_POINT ( 'NONE',  ( 3.474262827703335166, 65.03518628210144925, 8.843639120294326972 ) ) ;
#34688 = CARTESIAN_POINT ( 'NONE',  ( 26.99999999999999645, 243.9812500012290570, -7.347880794884117764E-16 ) ) ;
#34689 = ADVANCED_FACE ( 'NONE', ( #24085 ), #18404, .F. ) ;
#34690 = FACE_OUTER_BOUND ( 'NONE', #25086, .T. ) ;
#34691 = CARTESIAN_POINT ( 'NONE',  ( 18.00000000000000000, 5.196152422706630247, -2.774999999999999467 ) ) ;
#34692 = CARTESIAN_POINT ( 'NONE',  ( 27.24356964375000345, 196.4843750006145626, -3.336375036156643733E-15 ) ) ;
#34693 = CARTESIAN_POINT ( 'NONE',  ( 26.99999999999999645, 246.1375000000000171, 3.464101615137751278 ) ) ;
#34694 = DIRECTION ( 'NONE',  ( 0.000000000000000000, -0.9932091452657081376, -0.1163425707149433747 ) ) ;
#34695 = CARTESIAN_POINT ( 'NONE',  ( -9.465287035748106703, 43.00231371789853796, 2.064181346179061460 ) ) ;
#34696 = CARTESIAN_POINT ( 'NONE',  ( -81.00000000000002842, 206.0000000000000000, 2.500000000000002220 ) ) ;
#34697 = ORIENTED_EDGE ( 'NONE', *, *, #1847, .T. ) ;
#34698 = VERTEX_POINT ( 'NONE', #28041 ) ;
#34699 = CARTESIAN_POINT ( 'NONE',  ( 15.24356964375000167, 249.3343750006145001, 3.323476615752272600 ) ) ;
#34700 = CARTESIAN_POINT ( 'NONE',  ( 4.622313124798831829, 46.16481371789854649, -11.61527771782809282 ) ) ;
#34701 = CARTESIAN_POINT ( 'NONE',  ( 19.68408634441911076, 5.407089921784862696, -7.996874999385533478 ) ) ;
#34702 = CARTESIAN_POINT ( 'NONE',  ( 15.24356964374999990, 3.323476615752268604, -9.290624999385480365 ) ) ;
#34703 = CARTESIAN_POINT ( 'NONE',  ( -12.50000000000000355, 15.68981371789854329, 0.1745138560722786503 ) ) ;
#34704 = ORIENTED_EDGE ( 'NONE', *, *, #19765, .T. ) ;
#34705 = CARTESIAN_POINT ( 'NONE',  ( 10.31873187879410914, 0.000000000000000000, -4.696874999385508787 ) ) ;
#34706 = CARTESIAN_POINT ( 'NONE',  ( -13.62178482187498396, 199.4281250006145569, 23.59362340125808188 ) ) ;
#34707 = CARTESIAN_POINT ( 'NONE',  ( 37.48811928047766884, 3.604726614523243278, 166.8231380282798568 ) ) ;
#34708 = APPLICATION_CONTEXT ( 'automotive_design' ) ;
#34709 = CARTESIAN_POINT ( 'NONE',  ( -66.22544563604516554, 216.3070033484980854, 6.137860380172893926 ) ) ;
#34710 = CARTESIAN_POINT ( 'NONE',  ( 23.87821517812500005, 248.0968750006144887, 4.985214923628404016 ) ) ;
#34711 =( NAMED_UNIT ( * ) SI_UNIT ( $, .STERADIAN. ) SOLID_ANGLE_UNIT ( ) );
#34712 = CARTESIAN_POINT ( 'NONE',  ( -26.89802933101758242, 194.9999999999999432, -3.124506137021467289 ) ) ;
#34713 = CARTESIAN_POINT ( 'NONE',  ( -62.26711230271183695, 214.4690446883608104, -1.321298161741814914 ) ) ;
#34714 =( BOUNDED_CURVE ( )  B_SPLINE_CURVE ( 2, ( #11010, #10635, #21840, #22397, #33765, #16522, #4578, #36406, #33946 ),
 .UNSPECIFIED., .F., .F. ) 
 B_SPLINE_CURVE_WITH_KNOTS ( ( 3, 2, 2, 2, 3 ),
 ( 0.6630434782608695121, 0.6666666666666666297, 0.6739130434782608647, 0.6811594202898550998, 0.6847826086956522174 ),
 .UNSPECIFIED. ) 
 CURVE ( )  GEOMETRIC_REPRESENTATION_ITEM ( )  RATIONAL_B_SPLINE_CURVE ( ( 0.9330127018922192983, 0.9330127018922182991, 1.000000000000000000, 0.8660254037844387076, 1.000000000000000000, 0.8660254037844387076, 1.000000000000000000, 0.9330127018922182991, 0.9330127018922192983 ) ) 
 REPRESENTATION_ITEM ( '' )  );
#34715 = CARTESIAN_POINT ( 'NONE',  ( -47.62872103062154849, 203.4690446883607535, 1.626142955000567936 ) ) ;
#34716 = CARTESIAN_POINT ( 'NONE',  ( 25.37039736927151878, 3.464101615137721524, 168.7961499886528713 ) ) ;
#34717 = VERTEX_POINT ( 'NONE', #1696 ) ;
#34718 = DIRECTION ( 'NONE',  ( 0.000000000000000000, 0.000000000000000000, 1.000000000000000000 ) ) ;
#34719 = CARTESIAN_POINT ( 'NONE',  ( 23.99999999999999645, 5.196152422706631135, -1.443749998770949006 ) ) ;
#34720 = CARTESIAN_POINT ( 'NONE',  ( 15.46528703574811736, 29.20231371789855501, -3.257655550456947768 ) ) ;
#34721 = CARTESIAN_POINT ( 'NONE',  ( -54.95163769728822700, 217.4189793300686233, -4.149950860017907139 ) ) ;
#34722 =( GEOMETRIC_REPRESENTATION_CONTEXT ( 3 ) GLOBAL_UNCERTAINTY_ASSIGNED_CONTEXT ( ( #15321 ) ) GLOBAL_UNIT_ASSIGNED_CONTEXT ( ( #32625, #23920, #18237 ) ) REPRESENTATION_CONTEXT ( 'NONE', 'WORKASPACE' ) );
#34723 = CARTESIAN_POINT ( 'NONE',  ( 10.69584247140445221, 7.247686282101428290, -6.932735513423970097 ) ) ;
#34724 = EDGE_CURVE ( 'NONE', #16035, #35447, #5927, .T. ) ;
#34725 = CARTESIAN_POINT ( 'NONE',  ( -0.1745138560725500443, 56.41018628210145636, 12.50000000000000355 ) ) ;
#34726 = VECTOR ( 'NONE', #22503, 1000.000000000000000 ) ;
#34727 = CARTESIAN_POINT ( 'NONE',  ( 10.56230152254410726, 0.000000000000000000, -5.400000000000043876 ) ) ;
#34728 = EDGE_LOOP ( 'NONE', ( #3510, #35865 ) ) ;
#34729 = CARTESIAN_POINT ( 'NONE',  ( -44.85788769728822700, 216.4690446883607535, 1.857196546604031662 ) ) ;
#34730 = CARTESIAN_POINT ( 'NONE',  ( 18.00000000000000355, 242.4250000000000114, 5.196152422706632912 ) ) ;
#34731 = CARTESIAN_POINT ( 'NONE',  ( -27.24356964374999990, 196.2218750006145456, -15.72908226750537786 ) ) ;
#34732 = CARTESIAN_POINT ( 'NONE',  ( 25.29522554115172639, 0.000000000000000000, 167.9369320615487311 ) ) ;
#34733 = LINE ( 'NONE', #29229, #32563 ) ;
#34734 = ADVANCED_FACE ( 'NONE', ( #7772 ), #28228, .T. ) ;
#34735 = CYLINDRICAL_SURFACE ( 'NONE', #17064, 7.500000000000000000 ) ;
#34736 = CARTESIAN_POINT ( 'NONE',  ( 52.59268362704444399, 124.7349959275252615, -0.5000000000000000000 ) ) ;
#34737 =( BOUNDED_CURVE ( )  B_SPLINE_CURVE ( 2, ( #11142, #10953, #28747, #16656, #25176, #8306, #31235 ),
 .UNSPECIFIED., .F., .F. ) 
 B_SPLINE_CURVE_WITH_KNOTS ( ( 3, 2, 2, 3 ),
 ( 0.3913043478260864738, 0.3985507246376804869, 0.4057971014492746109, 0.4130434782608686239 ),
 .UNSPECIFIED. ) 
 CURVE ( )  GEOMETRIC_REPRESENTATION_ITEM ( )  RATIONAL_B_SPLINE_CURVE ( ( 1.000000000000009326, 0.8660254037844296038, 1.000000000000000000, 0.8660254037844387076, 1.000000000000000000, 0.8660254037844561381, 0.9999999999999825695 ) ) 
 REPRESENTATION_ITEM ( '' )  );
#34738 = CARTESIAN_POINT ( 'NONE',  ( 21.00000000000000000, 245.0218750006145285, 6.646953231504538984 ) ) ;
#34739 = CARTESIAN_POINT ( 'NONE',  ( -2.064181346179062349, 100.5023137178985451, -9.465287035748106703 ) ) ;
#34740 = CARTESIAN_POINT ( 'NONE',  ( 24.81804784950163878, -3.464101615138005741, 162.4827660882720295 ) ) ;
#34741 = ORIENTED_EDGE ( 'NONE', *, *, #14005, .F. ) ;
#34742 = CARTESIAN_POINT ( 'NONE',  ( -56.53497103062156270, 204.4285982733020148, -3.350049139982115509 ) ) ;
#34743 = CARTESIAN_POINT ( 'NONE',  ( 13.49999999999999645, 197.2625000012290286, -23.38268590217984766 ) ) ;
#34744 = CARTESIAN_POINT ( 'NONE',  ( 26.99999999999999645, 247.1687500012290570, -3.464101615137755275 ) ) ;
#34745 = EDGE_LOOP ( 'NONE', ( #35624, #6127, #35098, #29021 ) ) ;
#34746 = CARTESIAN_POINT ( 'NONE',  ( 12.46528703574811558, 102.8023137178985564, -2.660918448318005947 ) ) ;
#34747 = CARTESIAN_POINT ( 'NONE',  ( 16.56230152254411436, -7.209453229046482114, -1.884374999385517446 ) ) ;
#34748 = CARTESIAN_POINT ( 'NONE',  ( 36.89818384675449892, -3.604726614523235284, 160.0801451655713663 ) ) ;
#34749 = CARTESIAN_POINT ( 'NONE',  ( 18.12178482187499640, 4.985214923628404904, -1.678124999385494087 ) ) ;
#34750 = CARTESIAN_POINT ( 'NONE',  ( -11.48171059495408208, 70.31481371789854506, 4.944772684328421875 ) ) ;
#34751 = CARTESIAN_POINT ( 'NONE',  ( -13.49999999999998401, 195.1250000000000284, 23.38268590217985476 ) ) ;
#34752 = ORIENTED_EDGE ( 'NONE', *, *, #22237, .T. ) ;
#34753 = ORIENTED_EDGE ( 'NONE', *, *, #5250, .T. ) ;
#34754 = ORIENTED_EDGE ( 'NONE', *, *, #19779, .T. ) ;
#34755 = CARTESIAN_POINT ( 'NONE',  ( 15.24356964374999990, 0.000000000000000000, -4.640624999385472904 ) ) ;
#34756 = DIRECTION ( 'NONE',  ( -0.000000000000000000, -0.000000000000000000, 1.000000000000000000 ) ) ;
#34757 = AXIS2_PLACEMENT_3D ( 'NONE', #11694, #26655, #28939 ) ;
#34758 = CARTESIAN_POINT ( 'NONE',  ( 23.87821517812500005, 246.2968750006145058, 4.985214923628404016 ) ) ;
#34759 = CARTESIAN_POINT ( 'NONE',  ( 8.715434833791931624, 36.86018628210144499, 8.962234695871760692 ) ) ;
#34760 = VECTOR ( 'NONE', #35260, 1000.000000000000114 ) ;
#34761 = CARTESIAN_POINT ( 'NONE',  ( -51.18377896937849414, 208.3738570449995109, 6.530955311639247363 ) ) ;
#34762 = CARTESIAN_POINT ( 'NONE',  ( 19.55576478543629193, 211.4442352145561586, -5.894939585092063616 ) ) ;
#34763 = CARTESIAN_POINT ( 'NONE',  ( -40.49627896937850835, 205.4690446883607535, -1.090244570138286351 ) ) ;
#34764 =( NAMED_UNIT ( * ) PLANE_ANGLE_UNIT ( ) SI_UNIT ( $, .RADIAN. ) );
#34765 = CARTESIAN_POINT ( 'NONE',  ( 30.88999790839687876, -6.928203230275506996, 163.0431933671852676 ) ) ;
#34766 = CARTESIAN_POINT ( 'NONE',  ( 6.932735513424201024, 110.8523137178985394, -10.69584247140429412 ) ) ;
#34767 = CARTESIAN_POINT ( 'NONE',  ( -53.96205436395491262, 213.2096571498974242, 3.378800118222489601 ) ) ;
#34768 = CARTESIAN_POINT ( 'NONE',  ( -46.83705436395489130, 203.8621396198270475, -6.307003348497942419 ) ) ;
#34769 = CARTESIAN_POINT ( 'NONE',  ( 15.24356964374999990, 0.000000000000000000, -3.403124999385470417 ) ) ;
#34770 = CARTESIAN_POINT ( 'NONE',  ( 18.00000000000000355, -5.196152422706632912, -1.725000000000004308 ) ) ;
#34771 = CARTESIAN_POINT ( 'NONE',  ( 0.1745138560722461762, 77.78981371789853938, 15.50000000000000533 ) ) ;
#34772 = CARTESIAN_POINT ( 'NONE',  ( -55.14211230271182984, 201.5309553116392181, 2.393094931466368980 ) ) ;
#34773 = EDGE_LOOP ( 'NONE', ( #4321, #5253, #7764, #37032 ) ) ;
#34774 = CARTESIAN_POINT ( 'NONE',  ( 23.99999999999999645, 240.8500000000000227, -5.196152422706631135 ) ) ;
#34775 = CARTESIAN_POINT ( 'NONE',  ( 12.50000000000000355, 109.3101862821014549, 0.1745138560725507937 ) ) ;
#34776 = CARTESIAN_POINT ( 'NONE',  ( -0.1745138560725817967, 38.01018628210144357, 15.50000000000000533 ) ) ;
#34777 = CARTESIAN_POINT ( 'NONE',  ( 36.93576976081443775, 7.646167579472024665E-16, 160.5097541291234506 ) ) ;
#34778 = CARTESIAN_POINT ( 'NONE',  ( 3.257655550457285720, 70.49768628210145494, -15.46528703574804986 ) ) ;
#34779 = CARTESIAN_POINT ( 'NONE',  ( -27.24356964374999279, 198.9406250006145171, 15.72908226750539384 ) ) ;
#34780 = CARTESIAN_POINT ( 'NONE',  ( 13.44051670066911086, 5.407089921784856479, -9.665624999385530103 ) ) ;
#34781 = CARTESIAN_POINT ( 'NONE',  ( 22.56230152254321197, 3.464101615138280632, -8.737500000000023803 ) ) ;
#34782 = CARTESIAN_POINT ( 'NONE',  ( -46.44122103062156270, 208.3738570449993404, -6.530955311639226935 ) ) ;
#34783 = CARTESIAN_POINT ( 'NONE',  ( 15.02202517871450738, 5.832799451530069845, -10.00000000000000000 ) ) ;
#34784 = CARTESIAN_POINT ( 'NONE',  ( -12.50000000000000355, 40.31018628210144783, -0.1745138560725492671 ) ) ;
#34785 = CARTESIAN_POINT ( 'NONE',  ( 5.727106289114498080E-15, 195.1625000000000227, 31.17691453623979214 ) ) ;
#34786 = CARTESIAN_POINT ( 'NONE',  ( 23.99999999999999645, 5.196152422706631135, -7.743749998770948828 ) ) ;
#34787 = CARTESIAN_POINT ( 'NONE',  ( 9.500000000000005329, 139.8898137178985621, -0.1745138560723090149 ) ) ;
#34788 = CARTESIAN_POINT ( 'NONE',  ( 26.75643035624999655, 247.8343750006145285, -7.049594010296217766E-16 ) ) ;
#34789 = ORIENTED_EDGE ( 'NONE', *, *, #25867, .F. ) ;
#34790 = CARTESIAN_POINT ( 'NONE',  ( 23.99999999999999645, 5.196152422706631135, -5.549999999999998934 ) ) ;
#34791 = DIRECTION ( 'NONE',  ( -1.558072081575740353E-16, -1.134704379232807653E-16, -1.000000000000000000 ) ) ;
#34792 = DIRECTION ( 'NONE',  ( 1.000000000000000000, 0.000000000000000000, 0.000000000000000000 ) ) ;
#34793 = CARTESIAN_POINT ( 'NONE',  ( 22.80587116629411071, -3.604726614523235284, -4.453124999385550176 ) ) ;
#34794 = CARTESIAN_POINT ( 'NONE',  ( 34.33409119757650529, -5.407089921784855591, 166.5908959372197558 ) ) ;
#34795 = CARTESIAN_POINT ( 'NONE',  ( 24.00000000000000000, 242.0499999999999829, 5.196152422706629359 ) ) ;
#34796 = CARTESIAN_POINT ( 'NONE',  ( 27.00000000000041567, 3.464101615137513690, -1.031249998770972454 ) ) ;
#34797 = CARTESIAN_POINT ( 'NONE',  ( -2.660918448318275509, 75.09768628210144925, 12.46528703574805874 ) ) ;
#34798 = VERTEX_POINT ( 'NONE', #16681 ) ;
#34799 = ORIENTED_EDGE ( 'NONE', *, *, #17122, .T. ) ;
#34800 = FACE_OUTER_BOUND ( 'NONE', #2959, .T. ) ;
#34801 = CARTESIAN_POINT ( 'NONE',  ( 27.00000000000001066, 194.9000000012290457, 15.58845726811988897 ) ) ;
#34802 = CARTESIAN_POINT ( 'NONE',  ( 23.87821517812500005, -4.985214923628404016, -7.190624999385470062 ) ) ;
#34803 = CARTESIAN_POINT ( 'NONE',  ( -0.1745138560722442889, 45.58981371789855785, -15.50000000000000533 ) ) ;
#34804 = CARTESIAN_POINT ( 'NONE',  ( 3.037124061885436328E-15, 143.0000000000000000, 24.80000000000000426 ) ) ;
#34805 = CARTESIAN_POINT ( 'NONE',  ( 23.87821517812500005, 240.1093750006145342, 4.985214923628404016 ) ) ;
#34806 = CARTESIAN_POINT ( 'NONE',  ( -47.82663769728823411, 206.0451222850691408, 2.149950860017832532 ) ) ;
#34807 = LINE ( 'NONE', #29113, #14955 ) ;
#34808 = CARTESIAN_POINT ( 'NONE',  ( 25.40961745350801948, 3.464101615137752166, 169.2444376027941360 ) ) ;
#34809 = CARTESIAN_POINT ( 'NONE',  ( -0.1745138560723084320, 27.18981371789855572, -9.500000000000005329 ) ) ;
#34810 = CARTESIAN_POINT ( 'NONE',  ( -56.53497103062156270, 204.4285982733020148, -3.350049139982115509 ) ) ;
#34811 = EDGE_CURVE ( 'NONE', #11818, #1984, #27483, .T. ) ;
#34812 = CARTESIAN_POINT ( 'NONE',  ( -37.72544563604516554, 216.3070033484980854, 6.137860380172893926 ) ) ;
#34813 = AXIS2_PLACEMENT_3D ( 'NONE', #26635, #20596, #35542 ) ;
#34814 = FACE_OUTER_BOUND ( 'NONE', #7870, .T. ) ;
#34815 = CARTESIAN_POINT ( 'NONE',  ( -27.24356964375001056, 194.8857344423495874, -9.915847621322177119 ) ) ;
#34816 = CARTESIAN_POINT ( 'NONE',  ( -5.770363421894122880, 133.5648137178985735, 14.38691631536194393 ) ) ;
#34817 = ORIENTED_EDGE ( 'NONE', *, *, #1028, .T. ) ;
#34818 = CARTESIAN_POINT ( 'NONE',  ( 4.944772684328679446, 43.18518628210144072, -11.48171059495397373 ) ) ;
#34819 = CARTESIAN_POINT ( 'NONE',  ( 10.56230152254294552, -3.464101615137081591, -8.399999998771011889 ) ) ;
#34820 = CARTESIAN_POINT ( 'NONE',  ( 7.234628195640309123, 198.9674038105676743, -27.00000000000000711 ) ) ;
#34821 = CARTESIAN_POINT ( 'NONE',  ( 25.14001085782205891, 3.604726614523240613, 168.9574683606716690 ) ) ;
#34822 = CARTESIAN_POINT ( 'NONE',  ( 18.00000000000000000, 5.196152422706630247, -1.818749998770963217 ) ) ;
#34823 = CARTESIAN_POINT ( 'NONE',  ( 22.80587116629411426, 7.646167579472024665E-16, -8.071874999385524774 ) ) ;
#34824 = CARTESIAN_POINT ( 'NONE',  ( -68.80580436395490551, 216.5000000000000000, 0.1155267958017343610 ) ) ;
#34825 = CARTESIAN_POINT ( 'NONE',  ( 6.840914352312096547, 62.16018628210144925, -6.594114490232313663 ) ) ;
#34826 = CYLINDRICAL_SURFACE ( 'NONE', #15268, 5.999999999999999112 ) ;
#34827 = DIRECTION ( 'NONE',  ( 0.000000000000000000, 1.000000000000000000, 0.000000000000000000 ) ) ;
#34828 = ADVANCED_FACE ( 'NONE', ( #13456 ), #24822, .F. ) ;
#34829 = CARTESIAN_POINT ( 'NONE',  ( 11.48171059495397728, 100.6851862821014691, 4.944772684328674117 ) ) ;
#34830 = CARTESIAN_POINT ( 'NONE',  ( 13.56230152254410548, 5.196152422706636465, -5.025000000000029665 ) ) ;
#34831 = CARTESIAN_POINT ( 'NONE',  ( 1.069080835302379631E-14, 198.4250000012290229, 27.00000000000000000 ) ) ;
#34832 = VERTEX_POINT ( 'NONE', #2074 ) ;
#34833 = CARTESIAN_POINT ( 'NONE',  ( 33.91574363238778034, 5.407089921784857367, 161.8091613863793725 ) ) ;
#34834 = CIRCLE ( 'NONE', #4485, 8.000000000000007105 ) ;
#34835 = CARTESIAN_POINT ( 'NONE',  ( 15.24356964374999990, 3.323476615752268604, -8.278124999385466865 ) ) ;
#34836 = CARTESIAN_POINT ( 'NONE',  ( -27.24356964374999279, 195.3968750006145285, 15.72908226750539384 ) ) ;
#34837 = CARTESIAN_POINT ( 'NONE',  ( 37.32470226282583781, -3.604726614523238837, 164.9552729693578215 ) ) ;
#34838 = CARTESIAN_POINT ( 'NONE',  ( 28.26746793355466281, 5.196152422706636465, 167.4886783261892162 ) ) ;
#34839 = CARTESIAN_POINT ( 'NONE',  ( 5.438367727407757144E-14, 198.0875000000000057, -27.00000000000000000 ) ) ;
#34840 = CARTESIAN_POINT ( 'NONE',  ( 26.99999999999999645, 248.4250000000000114, -7.347880794884117764E-16 ) ) ;
#34841 = CARTESIAN_POINT ( 'NONE',  ( 13.62178482187501416, 197.7031250006145342, 23.59362340125806767 ) ) ;
#34842 = EDGE_CURVE ( 'NONE', #4816, #941, #15934, .T. ) ;
#34843 = AXIS2_PLACEMENT_3D ( 'NONE', #11082, #16598, #25669 ) ;
#34844 = CARTESIAN_POINT ( 'NONE',  ( -0.1745138560722763466, 119.1898137178985593, -12.50000000000000355 ) ) ;
#34845 = CARTESIAN_POINT ( 'NONE',  ( 8.715434833791931624, 119.6601862821014493, 8.962234695871760692 ) ) ;
#34847 = ORIENTED_EDGE ( 'NONE', *, *, #33928, .F. ) ;
#34846 = ORIENTED_EDGE ( 'NONE', *, *, #29725, .T. ) ;
#34848 = CARTESIAN_POINT ( 'NONE',  ( 13.62178482187501416, 198.1531250006145228, 23.59362340125806767 ) ) ;
#34849 = CARTESIAN_POINT ( 'NONE',  ( 15.24356964375000167, 243.0343750006144887, 3.323476615752272600 ) ) ;
#34850 = CARTESIAN_POINT ( 'NONE',  ( -6.092822981423666739, 100.2148137178985650, -14.25334919248795096 ) ) ;
#34851 = CARTESIAN_POINT ( 'NONE',  ( 15.24356964374999990, 3.323476615752268604, -3.890624999385467575 ) ) ;
#34852 = CARTESIAN_POINT ( 'NONE',  ( 26.75643035624999655, 246.5218750006145285, -3.323476615752271712 ) ) ;
#34853 = CARTESIAN_POINT ( 'NONE',  ( 5.727106289114498080E-15, 196.6250000012290400, 31.17691453623979214 ) ) ;
#34854 = CARTESIAN_POINT ( 'NONE',  ( 2.064181346179061460, 77.50231371789855928, 9.465287035748106703 ) ) ;
#34855 = CARTESIAN_POINT ( 'NONE',  ( 13.44051670066911441, -5.407089921784859143, -5.915624999385554972 ) ) ;
#34856 = CARTESIAN_POINT ( 'NONE',  ( 15.24356964374999990, 241.1968750006145115, 0.000000000000000000 ) ) ;
#34857 = CARTESIAN_POINT ( 'NONE',  ( -6.932735513424201912, 41.85231371789855359, 10.69584247140429412 ) ) ;
#34858 = FACE_OUTER_BOUND ( 'NONE', #3412, .T. ) ;
#34859 = EDGE_CURVE ( 'NONE', #10453, #17469, #33168, .T. ) ;
#34860 = CARTESIAN_POINT ( 'NONE',  ( -2.660918448318275509, 93.49768628210145494, 12.46528703574805874 ) ) ;
#34861 = CARTESIAN_POINT ( 'NONE',  ( 16.56230152254411081, -6.928203230275506996, -2.924999998770990928 ) ) ;
#34862 = VECTOR ( 'NONE', #21844, 1000.000000000000000 ) ;
#34863 = CARTESIAN_POINT ( 'NONE',  ( -65.83705436395491972, 206.7903428501026042, -3.378800118222489157 ) ) ;
#34864 = CARTESIAN_POINT ( 'NONE',  ( 12.46528703574805874, 137.1976862821014720, 2.660918448318279950 ) ) ;
#34865 = CARTESIAN_POINT ( 'NONE',  ( 36.67433401601032017, 3.464101615138187817, 160.3161781399470840 ) ) ;
#34866 = CARTESIAN_POINT ( 'NONE',  ( 5.770363421893814682, 92.63518628210147199, 14.38691631536207183 ) ) ;
#34867 = CARTESIAN_POINT ( 'NONE',  ( 4.944772684328679446, 15.58518628210145351, -11.48171059495397373 ) ) ;
#34868 = CARTESIAN_POINT ( 'NONE',  ( -20.68320042480035426, 195.0000000000000000, -17.35526491262920956 ) ) ;
#34869 = EDGE_CURVE ( 'NONE', #18512, #28262, #16120, .T. ) ;
#34870 = CARTESIAN_POINT ( 'NONE',  ( 13.50000000000001421, 196.6625000012290343, 23.38268590217984055 ) ) ;
#34871 = CARTESIAN_POINT ( 'NONE',  ( 9.465287035748067623, 137.1976862821014436, 2.064181346179272847 ) ) ;
#34872 = CARTESIAN_POINT ( 'NONE',  ( 20.99999999999998579, 247.6937500012290059, -5.999999999999997335 ) ) ;
#34873 = CARTESIAN_POINT ( 'NONE',  ( 13.62178482187501416, 195.9593750006145569, 23.59362340125806767 ) ) ;
#34874 = CARTESIAN_POINT ( 'NONE',  ( 23.87821517812500005, 243.1468750006145285, 4.985214923628404016 ) ) ;
#34875 = ORIENTED_EDGE ( 'NONE', *, *, #25253, .F. ) ;
#34876 = CARTESIAN_POINT ( 'NONE',  ( 28.25155051613373658, 5.407089921784856479, 168.7040655364119743 ) ) ;
#34877 = CARTESIAN_POINT ( 'NONE',  ( 8.710071997420127943, 54.68518628210145494, 3.796722387233375073 ) ) ;
#34878 = CARTESIAN_POINT ( 'NONE',  ( 15.24356964375000167, -3.323476615752272600, -1.003124999385444527 ) ) ;
#34879 = AXIS2_PLACEMENT_3D ( 'NONE', #16188, #30401, #8022 ) ;
#34880 = EDGE_CURVE ( 'NONE', #21721, #36421, #25383, .T. ) ;
#34881 = CARTESIAN_POINT ( 'NONE',  ( 21.00000000000000000, 241.1125000000000114, 5.999999999999998224 ) ) ;
#34882 = DIRECTION ( 'NONE',  ( 0.000000000000000000, 0.000000000000000000, -1.000000000000000000 ) ) ;
#34883 = CARTESIAN_POINT ( 'NONE',  ( -27.24356964374999990, 196.6718750006145342, -15.72908226750537786 ) ) ;
#34884 = CARTESIAN_POINT ( 'NONE',  ( 20.99999999999999645, 185.0294372515228645, 0.000000000000000000 ) ) ;
#34885 = CARTESIAN_POINT ( 'NONE',  ( 2.064181346179061460, 40.70231371789854791, 9.465287035748106703 ) ) ;
#34886 = PLANE ( 'NONE',  #16986 ) ;
#34887 = EDGE_LOOP ( 'NONE', ( #26783, #24100, #10138, #25447 ) ) ;
#34888 = ORIENTED_EDGE ( 'NONE', *, *, #1759, .F. ) ;
#34889 = CARTESIAN_POINT ( 'NONE',  ( 15.24356964374999990, 249.7093750006145285, -3.323476615752268604 ) ) ;
#34890 = CARTESIAN_POINT ( 'NONE',  ( -4.944772684328424539, 45.01481371789854791, -11.48171059495408031 ) ) ;
#34891 = CARTESIAN_POINT ( 'NONE',  ( 19.68408634441911076, 5.407089921784862696, -7.546874999385555505 ) ) ;
#34892 = CARTESIAN_POINT ( 'NONE',  ( 26.75643035624999655, 7.049594010296217766E-16, -8.578124999385483562 ) ) ;
#34893 = CARTESIAN_POINT ( 'NONE',  ( 12.50000000000000355, 20.28981371789855004, -0.1745138560722771515 ) ) ;
#34894 = EDGE_CURVE ( 'NONE', #27300, #9547, #18658, .T. ) ;
#34895 = VERTEX_POINT ( 'NONE', #30710 ) ;
#34896 = CARTESIAN_POINT ( 'NONE',  ( 19.68408634441911431, 5.407089921784862696, -4.846874999385547333 ) ) ;
#34897 = VERTEX_POINT ( 'NONE', #30330 ) ;
#34898 = CARTESIAN_POINT ( 'NONE',  ( 25.06810737005524459, -3.604726614523244610, 168.1356077347459461 ) ) ;
#34899 = CARTESIAN_POINT ( 'NONE',  ( -63.45461230271184405, 207.6069050685336492, -8.469044688360751749 ) ) ;
#34900 = CARTESIAN_POINT ( 'NONE',  ( 26.75643035624999655, 249.5218750006145001, -7.049594010296217766E-16 ) ) ;
#34901 = AXIS2_PLACEMENT_3D ( 'NONE', #3582, #9459, #3763 ) ;
#34902 = CARTESIAN_POINT ( 'NONE',  ( -25.24001216047315310, 194.9999999999999716, 9.971080493324555150 ) ) ;
#34903 = EDGE_CURVE ( 'NONE', #20369, #18467, #34080, .T. ) ;
#34904 = CARTESIAN_POINT ( 'NONE',  ( -54.54836230271183695, 206.0451222850691977, -2.149950860017851184 ) ) ;
#34905 = CARTESIAN_POINT ( 'NONE',  ( -33.18080436395490551, 203.5000000000000000, -0.1155267958017335561 ) ) ;
#34906 = CARTESIAN_POINT ( 'NONE',  ( 31.31896757967941625, 7.209453229046475009, 167.9463391462434174 ) ) ;
#34907 = ORIENTED_EDGE ( 'NONE', *, *, #15614, .F. ) ;
#34908 = DIRECTION ( 'NONE',  ( -0.000000000000000000, 1.000000000000000000, -0.000000000000000000 ) ) ;
#34909 = CARTESIAN_POINT ( 'NONE',  ( -10.83675517735179028, 14.53981371789855892, 11.08355503943118947 ) ) ;
#34910 = CARTESIAN_POINT ( 'NONE',  ( -60.09747103062157692, 214.3500491399821044, -7.303452534266878793 ) ) ;
#34911 = CARTESIAN_POINT ( 'NONE',  ( -1.715153634034234598, 134.3226862821014436, -9.534712964251941258 ) ) ;
#34912 = CARTESIAN_POINT ( 'NONE',  ( -8.715434833791929847, 50.66018628210144925, -8.962234695871762469 ) ) ;
#34913 = CARTESIAN_POINT ( 'NONE',  ( 10.56230152254410903, 3.464101615137757051, -3.637500000000027267 ) ) ;
#34914 = ORIENTED_EDGE ( 'NONE', *, *, #34206, .F. ) ;
#34915 = CARTESIAN_POINT ( 'NONE',  ( -41.88913769728823411, 206.8500491399821044, -5.686928522499717253 ) ) ;
#34916 = CARTESIAN_POINT ( 'NONE',  ( 16.56230152254411081, 6.928203230275506996, -5.399999998770983467 ) ) ;
#34917 = CARTESIAN_POINT ( 'NONE',  ( 7.954856959092191815, 18.17268628210144499, 5.529263428287477744 ) ) ;
#34918 = CARTESIAN_POINT ( 'NONE',  ( -27.24356964374999990, 197.1218750006145228, -15.72908226750537786 ) ) ;
#34919 = CARTESIAN_POINT ( 'NONE',  ( 26.99999999999967670, 3.464101615137938683, -1.537500000000000311 ) ) ;
#34920 = CARTESIAN_POINT ( 'NONE',  ( 7.234628195640269155, 196.1950961906613600, 27.00000000000003197 ) ) ;
#34921 = CARTESIAN_POINT ( 'NONE',  ( 34.20868437832884013, 5.196152422706631135, 166.5548135579648488 ) ) ;
#34922 = CARTESIAN_POINT ( 'NONE',  ( 37.30512370425449120, -3.464101615137641144, 167.5261372686103698 ) ) ;
#34923 = CARTESIAN_POINT ( 'NONE',  ( 15.24356964374999990, 244.4218750006145058, -3.323476615752268604 ) ) ;
#34924 = CARTESIAN_POINT ( 'NONE',  ( -7.954856959092309943, 88.42731371789855643, 5.529263428287300108 ) ) ;
#34925 = DIRECTION ( 'NONE',  ( -0.1219804832088915297, -0.9925324990730154395, 0.000000000000000000 ) ) ;
#34926 = ORIENTED_EDGE ( 'NONE', *, *, #9709, .F. ) ;
#34927 = CARTESIAN_POINT ( 'NONE',  ( -59.70163769728823411, 215.6869285224996986, -3.149950860017881382 ) ) ;
#34928 = CARTESIAN_POINT ( 'NONE',  ( 18.00000000000000355, 246.0812500012290513, 5.196152422706632912 ) ) ;
#34929 = CARTESIAN_POINT ( 'NONE',  ( 2.660918448318003282, 95.90231371789856496, 12.46528703574811558 ) ) ;
#34930 = CARTESIAN_POINT ( 'NONE',  ( 16.56230152254411436, -7.209453229046482114, -2.334374999385512961 ) ) ;
#34931 = CARTESIAN_POINT ( 'NONE',  ( 13.49999999999999645, 198.1625000012290343, -23.38268590217984766 ) ) ;
#34932 = CARTESIAN_POINT ( 'NONE',  ( 23.87821517812500005, -4.985214923628404016, -2.803124999385481431 ) ) ;
#34933 = CARTESIAN_POINT ( 'NONE',  ( 10.49813415416005213, 74.62731371789855928, -7.228626920338837358 ) ) ;
#34934 = CARTESIAN_POINT ( 'NONE',  ( 27.24356964375000345, 196.9343750006145228, -3.336375036156643733E-15 ) ) ;
#34935 = ORIENTED_EDGE ( 'NONE', *, *, #1776, .T. ) ;
#34936 = ORIENTED_EDGE ( 'NONE', *, *, #5307, .T. ) ;
#34937 = CARTESIAN_POINT ( 'NONE',  ( 26.75643035624999655, 7.049594010296217766E-16, -5.315624999385482496 ) ) ;
#34938 = CARTESIAN_POINT ( 'NONE',  ( 10.49999999999999467, 244.5000000000000000, -2.500000000000000000 ) ) ;
#34939 = CARTESIAN_POINT ( 'NONE',  ( 18.12178482187499640, 246.9718750006145171, -4.985214923628404904 ) ) ;
#34940 = CARTESIAN_POINT ( 'NONE',  ( -8.715434833791929847, 32.26018628210145067, -8.962234695871762469 ) ) ;
#34941 = ADVANCED_FACE ( 'NONE', ( #18789 ), #22367, .F. ) ;
#34942 =( BOUNDED_CURVE ( )  B_SPLINE_CURVE ( 2, ( #16044, #36295, #15476, #21914, #32712, #4094, #868 ),
 .UNSPECIFIED., .F., .F. ) 
 B_SPLINE_CURVE_WITH_KNOTS ( ( 3, 2, 2, 3 ),
 ( 0.5434782608695617467, 0.5507246376811569810, 0.5579710144927523263, 0.5652173913043474496 ),
 .UNSPECIFIED. ) 
 CURVE ( )  GEOMETRIC_REPRESENTATION_ITEM ( )  RATIONAL_B_SPLINE_CURVE ( ( 1.000000000000063727, 0.8660254037843750918, 1.000000000000000000, 0.8660254037844387076, 1.000000000000000000, 0.8660254037844448138, 0.9999999999999938938 ) ) 
 REPRESENTATION_ITEM ( '' )  );
#34943 = CARTESIAN_POINT ( 'NONE',  ( -50.59002896937850124, 204.4285982733020433, 3.350049139982171020 ) ) ;
#34944 = CARTESIAN_POINT ( 'NONE',  ( 20.60729646369627943, 211.0472094301501045, -5.999999999999998224 ) ) ;
#34945 = CARTESIAN_POINT ( 'NONE',  ( -66.62127896937846572, 216.5309553116391612, 1.626142955000506873 ) ) ;
#34946 = CARTESIAN_POINT ( 'NONE',  ( 30.83116778204221475, 6.928203230275506996, 162.3707619459733564 ) ) ;
#34947 = CARTESIAN_POINT ( 'NONE',  ( 12.50000000000000355, 112.2898137178985678, -0.1745138560722771515 ) ) ;
#34948 = CARTESIAN_POINT ( 'NONE',  ( -64.64955436395490551, 213.3788001182225003, -3.209657149897400252 ) ) ;
#34950 = EDGE_CURVE ( 'NONE', #6148, #20636, #17604, .T. ) ;
#34949 = CARTESIAN_POINT ( 'NONE',  ( -65.83705436395487709, 205.3262412349647263, -4.842901733360204020 ) ) ;
#34951 = CARTESIAN_POINT ( 'NONE',  ( 20.99999999999999645, 6.646953231504538984, -3.515624999385498217 ) ) ;
#34952 = CARTESIAN_POINT ( 'NONE',  ( 13.62178482187501416, 195.0031250006145456, 23.59362340125806767 ) ) ;
#34953 = CARTESIAN_POINT ( 'NONE',  ( 15.46528703574811736, 75.20231371789854791, -3.257655550456947768 ) ) ;
#34954 = CARTESIAN_POINT ( 'NONE',  ( -58.70461230271184405, 207.6069050685336492, -8.469044688360751749 ) ) ;
#34955 = ORIENTED_EDGE ( 'NONE', *, *, #5536, .T. ) ;
#34956 = CARTESIAN_POINT ( 'NONE',  ( 26.99999999999999645, 7.347880794884117764E-16, -0.6187499987709565996 ) ) ;
#34957 = CARTESIAN_POINT ( 'NONE',  ( 8.962234695871762469, 98.96018628210146062, -8.715434833791931624 ) ) ;
#34958 = CARTESIAN_POINT ( 'NONE',  ( 11.08355503943142750, 52.96018628210144641, -10.83675517735155225 ) ) ;
#34959 = FACE_OUTER_BOUND ( 'NONE', #6692, .T. ) ;
#34960 =( BOUNDED_SURFACE ( )  B_SPLINE_SURFACE ( 1, 2, ( 
 ( #19440, #33640, #14109, #25661, #36844, #10887, #22833, #13550, #25103, #13746, #4821, #22276, #7679, #16402, #27948, #2163, #33829, #30990, #22460, #34007, #31535, #26212, #6319, #2720, #14478, #8422, #37396, #3472, #3282, #59, #23572, #17891, #20364, #29050, #23013, #31721, #17328, #19991, #34749, #11446, #15041, #14854, #29436, #34563, #3094, #11626, #14662, #31907, #26589, #35117, #5937, #17701, #9166, #249, #5560, #619, #20548, #28681, #29241, #8977, #5749, #23201, #17516, #12188, #25848, #17145, #11813, #23383, #34932, #26403, #23760, #32091, #14295, #8603, #20173, #6123, #26031, #28871, #436, #2906, #20733, #12001, #8792, #32276, #29812, #35493, #4221, #18268, #18654, #24328, #32656, #15607, #26969, #6697, #35870, #1186, #35683, #9735, #21496, #24511, #3846, #24141, #18840, #12950, #27349, #12760, #33226, #30005, #21307, #9543, #9912, #18464, #15423, #35299, #30386, #12381, #23951, #15990, #32843, #998, #10103, #21117, #6508, #20926, #12574, #7265, #27163, #6888, #27538, #4035, #33037, #7086, #30195, #15799, #1563, #36059, #4407, #1379, #21672, #13135, #9355, #32465, #18083, #29624, #15230, #3659, #26780, #810, #13700, #31132, #5338, #10844, #33412, #16174, #19024, #22418, #4783, #27724, #33786, #22605, #25435, #7824, #34150, #30581, #19215, #24878, #5149, #7638, #8007, #25251, #22048, #4963, #16357, #33599, #36801, #28091, #25062, #36615, #33965, #13886, #30761, #13504, #8197, #2312, #16730, #2123, #19773, #19401, #10656, #36427, #19580, #30945, #27905, #24690, #31310, #1754, #13320, #16916, #22235, #1936, #36987, #10470, #7450, #10285, #16545, #28457, #28276, #11030, #2493, #36243, #21859, #4597, #20320, #8562, #32235, #3239, #23528, #17662, #392, #14253, #14622, #17101, #34892, #11585, #29390, #6274, #25989, #19, #37174, #31861, #11958, #8381, #20129, #14068, #5516, #9123, #8932, #5705, #29197, #35074, #23160, #34702, #28640, #37351, #22974, #25617, #2861, #2678, #20690, #20509, #17851, #25802, #8749, #17285, #5895, #17473, #11215, #14811, #29008, #23341, #26356, #3052, #22787, #34336, #26173, #19952, #32046, #209, #11775 ),
 ( #6077, #31493, #11403, #34522, #31676, #28826, #14435, #35828, #21262, #9312, #9868, #12141, #21075, #36016, #1335, #18037, #7226, #18415, #10055, #29767, #18799, #15753, #23908, #21631, #3426, #33182, #23717, #32613, #14994, #21449, #12713, #30153, #9498, #26545, #27120, #29581, #18227, #4181, #15185, #574, #24469, #35257, #20883, #27304, #35639, #26732, #12905, #32989, #32422, #6467, #7042, #29961, #3798, #955, #15376, #3619, #766, #26925, #12334, #35450, #6651, #9685, #32801, #24283, #12530, #24093, #6837, #3989, #15563, #1143, #18609, #10431, #8159, #1894, #4365, #36762, #36573, #19359, #10615, #33741, #27497, #10988, #19171, #10804, #34107, #19541, #2085, #36197, #30719, #30340, #25017, #7781, #15944, #1518, #31088, #13092, #5112, #24647, #7595, #16130, #10241, #30535, #16691, #25211, #13465, #21817, #30900, #33369, #4921, #7406, #13278, #18978, #2268, #16502, #28050, #4555, #22560, #24832, #28239, #13845, #36384, #27680, #13658, #1706, #4739, #25393, #22004, #33556, #36943, #16315, #27862, #22194, #22377, #33925, #7967, #673, #17388, #32517, #12244, #9219, #9033, #17757, #32144, #28928, #29677, #20604, #11684, #15282, #26836, #26455, #12055, #29490, #14721, #3151, #14905, #31962, #26268, #303, #6184, #11868, #35551, #29298, #31271, #26643, #489, #20790, #23627, #35171, #2965, #865, #3336, #23815, #24005, #9408, #3528, #26089, #32334, #19733, #6372, #17945, #5806, #14533, #20984, #119, #6561, #23258, #34989, #5994, #34802, #20419, #18136, #15094, #35357, #8847, #3712, #17574, #12436, #29107, #23437, #1051, #19077, #10153, #21728, #13372, #27775, #30057, #10340, #27397, #35923, #24378, #29867, #9965, #18890, #33091, #27589, #9781, #7136, #15473, #24189, #33278, #32897, #18708, #7317, #4462, #1428, #27027, #16040, #18323, #27214, #4645, #7502, #35734, #24927, #24561, #16225, #21545, #9596, #21910, #4091, #1805, #21169, #32708, #3901, #1237, #6749, #1618, #30441, #12625, #33460, #21357, #30248, #6949, #18518, #15663, #36292, #13188, #4275, #12808, #36111, #15849, #24743, #13005, #30629, #27958, #8431, #37037, #11084, #2730, #17154 ) ),
 .UNSPECIFIED., .F., .F., .F. ) 
 B_SPLINE_SURFACE_WITH_KNOTS ( ( 2, 2 ),
 ( 3, 2, 2, 2, 2, 2, 2, 2, 2, 2, 2, 2, 2, 2, 2, 2, 2, 2, 2, 2, 2, 2, 2, 2, 2, 2, 2, 2, 2, 2, 2, 2, 2, 2, 2, 2, 2, 2, 2, 2, 2, 2, 2, 2, 2, 2, 2, 2, 2, 2, 2, 2, 2, 2, 2, 2, 2, 2, 2, 2, 2, 2, 2, 2, 2, 2, 2, 2, 2, 2, 2, 2, 2, 2, 2, 2, 2, 2, 2, 2, 2, 2, 2, 2, 2, 2, 2, 2, 2, 2, 2, 2, 2, 2, 2, 2, 2, 2, 2, 2, 2, 2, 2, 2, 2, 2, 2, 2, 2, 2, 2, 2, 2, 2, 2, 2, 2, 2, 2, 2, 2, 2, 2, 2, 2, 2, 2, 2, 2, 2, 2, 2, 2, 2, 3 ),
 ( 0.000000000000000000, 1.000000000000000000 ),
 ( 0.000000000000000000, 0.007246376811594202987, 0.01449275362318840597, 0.02173913043478260809, 0.02898550724637681195, 0.03623188405797101580, 0.04347826086956521618, 0.05072463768115942351, 0.05797101449275362389, 0.06521739130434782428, 0.07246376811594203160, 0.07971014492753622505, 0.08695652173913043237, 0.09420289855072463969, 0.1014492753623188470, 0.1086956521739130405, 0.1159420289855072478, 0.1231884057971014551, 0.1304347826086956486, 0.1376811594202898559, 0.1449275362318840632, 0.1521739130434782705, 0.1594202898550724501, 0.1666666666666666574, 0.1739130434782608647, 0.1811594202898550721, 0.1884057971014492794, 0.1956521739130434867, 0.2028985507246376940, 0.2101449275362318736, 0.2173913043478260809, 0.2246376811594202882, 0.2318840579710144956, 0.2391304347826087029, 0.2463768115942029102, 0.2536231884057971175, 0.2608695652173912971, 0.2681159420289855322, 0.2753623188405797118, 0.2826086956521738913, 0.2898550724637681264, 0.2971014492753623060, 0.3043478260869565410, 0.3115942028985507206, 0.3188405797101449002, 0.3260869565217391353, 0.3333333333333333148, 0.3405797101449275499, 0.3478260869565217295, 0.3550724637681159646, 0.3623188405797101441, 0.3695652173913043237, 0.3768115942028985588, 0.3840579710144927383, 0.3913043478260869734, 0.3985507246376811530, 0.4057971014492753881, 0.4130434782608695676, 0.4202898550724637472, 0.4275362318840579823, 0.4347826086956521618, 0.4420289855072463969, 0.4492753623188405765, 0.4565217391304347561, 0.4637681159420289911, 0.4710144927536231707, 0.4782608695652174058, 0.4855072463768115854, 0.4927536231884058204, 0.5000000000000000000, 0.5072463768115942351, 0.5144927536231883591, 0.5217391304347825942, 0.5289855072463768293, 0.5362318840579710644, 0.5434782608695651884, 0.5507246376811594235, 0.5579710144927536586, 0.5652173913043477826, 0.5724637681159420177, 0.5797101449275362528, 0.5869565217391304879, 0.5942028985507246119, 0.6014492753623188470, 0.6086956521739130821, 0.6159420289855072062, 0.6231884057971014412, 0.6304347826086956763, 0.6376811594202898004, 0.6449275362318840354, 0.6521739130434782705, 0.6594202898550725056, 0.6666666666666666297, 0.6739130434782608647, 0.6811594202898550998, 0.6884057971014492239, 0.6956521739130434590, 0.7028985507246376940, 0.7101449275362319291, 0.7173913043478260532, 0.7246376811594202882, 0.7318840579710145233, 0.7391304347826086474, 0.7463768115942028825, 0.7536231884057971175, 0.7608695652173913526, 0.7681159420289854767, 0.7753623188405797118, 0.7826086956521739468, 0.7898550724637680709, 0.7971014492753623060, 0.8043478260869565410, 0.8115942028985507761, 0.8188405797101449002, 0.8260869565217391353, 0.8333333333333333703, 0.8405797101449274944, 0.8478260869565217295, 0.8550724637681159646, 0.8623188405797101996, 0.8695652173913043237, 0.8768115942028985588, 0.8840579710144927938, 0.8913043478260869179, 0.8985507246376811530, 0.9057971014492753881, 0.9130434782608695121, 0.9202898550724637472, 0.9275362318840579823, 0.9347826086956522174, 0.9420289855072463414, 0.9492753623188405765, 0.9565217391304348116, 0.9637681159420289356, 0.9662082973083875315 ),
 .UNSPECIFIED. ) 
 GEOMETRIC_REPRESENTATION_ITEM ( )  RATIONAL_B_SPLINE_SURFACE ( (
 ( 1.000000000000000000, 0.8660254037844387076, 1.000000000000000000, 0.8660254037844387076, 1.000000000000000000, 0.8660254037844387076, 1.000000000000000000, 0.8660254037844387076, 1.000000000000000000, 0.8660254037844387076, 1.000000000000000000, 0.8660254037844387076, 1.000000000000000000, 0.8660254037844387076, 1.000000000000000000, 0.8660254037844387076, 1.000000000000000000, 0.8660254037844387076, 1.000000000000000000, 0.8660254037844387076, 1.000000000000000000, 0.8660254037844387076, 1.000000000000000000, 0.8660254037844387076, 1.000000000000000000, 0.8660254037844387076, 1.000000000000000000, 0.8660254037844387076, 1.000000000000000000, 0.8660254037844387076, 1.000000000000000000, 0.8660254037844387076, 1.000000000000000000, 0.8660254037844387076, 1.000000000000000000, 0.8660254037844387076, 1.000000000000000000, 0.8660254037844387076, 1.000000000000000000, 0.8660254037844387076, 1.000000000000000000, 0.8660254037844387076, 1.000000000000000000, 0.8660254037844387076, 1.000000000000000000, 0.8660254037844387076, 1.000000000000000000, 0.8660254037844387076, 1.000000000000000000, 0.8660254037844387076, 1.000000000000000000, 0.8660254037844387076, 1.000000000000000000, 0.8660254037844387076, 1.000000000000000000, 0.8660254037844387076, 1.000000000000000000, 0.8660254037844387076, 1.000000000000000000, 0.8660254037844387076, 1.000000000000000000, 0.8660254037844387076, 1.000000000000000000, 0.8660254037844387076, 1.000000000000000000, 0.8660254037844387076, 1.000000000000000000, 0.8660254037844387076, 1.000000000000000000, 0.8660254037844387076, 1.000000000000000000, 0.8660254037844387076, 1.000000000000000000, 0.8660254037844387076, 1.000000000000000000, 0.8660254037844387076, 1.000000000000000000, 0.8660254037844387076, 1.000000000000000000, 0.8660254037844387076, 1.000000000000000000, 0.8660254037844387076, 1.000000000000000000, 0.8660254037844387076, 1.000000000000000000, 0.8660254037844387076, 1.000000000000000000, 0.8660254037844387076, 1.000000000000000000, 0.8660254037844387076, 1.000000000000000000, 0.8660254037844387076, 1.000000000000000000, 0.8660254037844387076, 1.000000000000000000, 0.8660254037844387076, 1.000000000000000000, 0.8660254037844387076, 1.000000000000000000, 0.8660254037844387076, 1.000000000000000000, 0.8660254037844387076, 1.000000000000000000, 0.8660254037844387076, 1.000000000000000000, 0.8660254037844387076, 1.000000000000000000, 0.8660254037844387076, 1.000000000000000000, 0.8660254037844387076, 1.000000000000000000, 0.8660254037844387076, 1.000000000000000000, 0.8660254037844387076, 1.000000000000000000, 0.8660254037844387076, 1.000000000000000000, 0.8660254037844387076, 1.000000000000000000, 0.8660254037844387076, 1.000000000000000000, 0.8660254037844387076, 1.000000000000000000, 0.8660254037844387076, 1.000000000000000000, 0.8660254037844387076, 1.000000000000000000, 0.8660254037844387076, 1.000000000000000000, 0.8660254037844387076, 1.000000000000000000, 0.8660254037844387076, 1.000000000000000000, 0.8660254037844387076, 1.000000000000000000, 0.8660254037844387076, 1.000000000000000000, 0.8660254037844387076, 1.000000000000000000, 0.8660254037844387076, 1.000000000000000000, 0.8660254037844387076, 1.000000000000000000, 0.8660254037844387076, 1.000000000000000000, 0.8660254037844387076, 1.000000000000000000, 0.8660254037844387076, 1.000000000000000000, 0.8660254037844387076, 1.000000000000000000, 0.8660254037844387076, 1.000000000000000000, 0.8660254037844387076, 1.000000000000000000, 0.8660254037844387076, 1.000000000000000000, 0.8660254037844387076, 1.000000000000000000, 0.8660254037844387076, 1.000000000000000000, 0.8660254037844387076, 1.000000000000000000, 0.8660254037844387076, 1.000000000000000000, 0.8660254037844387076, 1.000000000000000000, 0.8660254037844387076, 1.000000000000000000, 0.8660254037844387076, 1.000000000000000000, 0.8660254037844387076, 1.000000000000000000, 0.8660254037844387076, 1.000000000000000000, 0.8660254037844387076, 1.000000000000000000, 0.8660254037844387076, 1.000000000000000000, 0.8660254037844387076, 1.000000000000000000, 0.8660254037844387076, 1.000000000000000000, 0.8660254037844387076, 1.000000000000000000, 0.8660254037844387076, 1.000000000000000000, 0.8660254037844387076, 1.000000000000000000, 0.8660254037844387076, 1.000000000000000000, 0.8660254037844387076, 1.000000000000000000, 0.8660254037844387076, 1.000000000000000000, 0.8660254037844387076, 1.000000000000000000, 0.8660254037844387076, 1.000000000000000000, 0.8660254037844387076, 1.000000000000000000, 0.8660254037844387076, 1.000000000000000000, 0.8660254037844387076, 1.000000000000000000, 0.8660254037844387076, 1.000000000000000000, 0.8660254037844387076, 1.000000000000000000, 0.8660254037844387076, 1.000000000000000000, 0.8660254037844387076, 1.000000000000000000, 0.8660254037844387076, 1.000000000000000000, 0.8660254037844387076, 1.000000000000000000, 0.8660254037844387076, 1.000000000000000000, 0.8660254037844387076, 1.000000000000000000, 0.8660254037844387076, 1.000000000000000000, 0.8660254037844387076, 1.000000000000000000, 0.8660254037844387076, 1.000000000000000000, 0.8660254037844387076, 1.000000000000000000, 0.8660254037844387076, 1.000000000000000000, 0.8660254037844387076, 1.000000000000000000, 0.8660254037844387076, 1.000000000000000000, 0.8660254037844387076, 1.000000000000000000, 0.8660254037844387076, 1.000000000000000000, 0.8660254037844387076, 1.000000000000000000, 0.8660254037844387076, 1.000000000000000000, 0.8660254037844387076, 1.000000000000000000, 0.8660254037844387076, 1.000000000000000000, 0.8660254037844387076, 1.000000000000000000, 0.8660254037844387076, 1.000000000000000000, 0.8660254037844387076, 1.000000000000000000, 0.8660254037844387076, 1.000000000000000000, 0.8660254037844387076, 1.000000000000000000, 0.8660254037844387076, 1.000000000000000000, 0.8660254037844387076, 1.000000000000000000, 0.8660254037844387076, 1.000000000000000000, 0.8660254037844387076, 1.000000000000000000, 0.8660254037844387076, 1.000000000000000000, 0.9548847207714133978, 0.9401541335272454170),
 ( 1.000000000000000000, 0.8660254037844387076, 1.000000000000000000, 0.8660254037844387076, 1.000000000000000000, 0.8660254037844387076, 1.000000000000000000, 0.8660254037844387076, 1.000000000000000000, 0.8660254037844387076, 1.000000000000000000, 0.8660254037844387076, 1.000000000000000000, 0.8660254037844387076, 1.000000000000000000, 0.8660254037844387076, 1.000000000000000000, 0.8660254037844387076, 1.000000000000000000, 0.8660254037844387076, 1.000000000000000000, 0.8660254037844387076, 1.000000000000000000, 0.8660254037844387076, 1.000000000000000000, 0.8660254037844387076, 1.000000000000000000, 0.8660254037844387076, 1.000000000000000000, 0.8660254037844387076, 1.000000000000000000, 0.8660254037844387076, 1.000000000000000000, 0.8660254037844387076, 1.000000000000000000, 0.8660254037844387076, 1.000000000000000000, 0.8660254037844387076, 1.000000000000000000, 0.8660254037844387076, 1.000000000000000000, 0.8660254037844387076, 1.000000000000000000, 0.8660254037844387076, 1.000000000000000000, 0.8660254037844387076, 1.000000000000000000, 0.8660254037844387076, 1.000000000000000000, 0.8660254037844387076, 1.000000000000000000, 0.8660254037844387076, 1.000000000000000000, 0.8660254037844387076, 1.000000000000000000, 0.8660254037844387076, 1.000000000000000000, 0.8660254037844387076, 1.000000000000000000, 0.8660254037844387076, 1.000000000000000000, 0.8660254037844387076, 1.000000000000000000, 0.8660254037844387076, 1.000000000000000000, 0.8660254037844387076, 1.000000000000000000, 0.8660254037844387076, 1.000000000000000000, 0.8660254037844387076, 1.000000000000000000, 0.8660254037844387076, 1.000000000000000000, 0.8660254037844387076, 1.000000000000000000, 0.8660254037844387076, 1.000000000000000000, 0.8660254037844387076, 1.000000000000000000, 0.8660254037844387076, 1.000000000000000000, 0.8660254037844387076, 1.000000000000000000, 0.8660254037844387076, 1.000000000000000000, 0.8660254037844387076, 1.000000000000000000, 0.8660254037844387076, 1.000000000000000000, 0.8660254037844387076, 1.000000000000000000, 0.8660254037844387076, 1.000000000000000000, 0.8660254037844387076, 1.000000000000000000, 0.8660254037844387076, 1.000000000000000000, 0.8660254037844387076, 1.000000000000000000, 0.8660254037844387076, 1.000000000000000000, 0.8660254037844387076, 1.000000000000000000, 0.8660254037844387076, 1.000000000000000000, 0.8660254037844387076, 1.000000000000000000, 0.8660254037844387076, 1.000000000000000000, 0.8660254037844387076, 1.000000000000000000, 0.8660254037844387076, 1.000000000000000000, 0.8660254037844387076, 1.000000000000000000, 0.8660254037844387076, 1.000000000000000000, 0.8660254037844387076, 1.000000000000000000, 0.8660254037844387076, 1.000000000000000000, 0.8660254037844387076, 1.000000000000000000, 0.8660254037844387076, 1.000000000000000000, 0.8660254037844387076, 1.000000000000000000, 0.8660254037844387076, 1.000000000000000000, 0.8660254037844387076, 1.000000000000000000, 0.8660254037844387076, 1.000000000000000000, 0.8660254037844387076, 1.000000000000000000, 0.8660254037844387076, 1.000000000000000000, 0.8660254037844387076, 1.000000000000000000, 0.8660254037844387076, 1.000000000000000000, 0.8660254037844387076, 1.000000000000000000, 0.8660254037844387076, 1.000000000000000000, 0.8660254037844387076, 1.000000000000000000, 0.8660254037844387076, 1.000000000000000000, 0.8660254037844387076, 1.000000000000000000, 0.8660254037844387076, 1.000000000000000000, 0.8660254037844387076, 1.000000000000000000, 0.8660254037844387076, 1.000000000000000000, 0.8660254037844387076, 1.000000000000000000, 0.8660254037844387076, 1.000000000000000000, 0.8660254037844387076, 1.000000000000000000, 0.8660254037844387076, 1.000000000000000000, 0.8660254037844387076, 1.000000000000000000, 0.8660254037844387076, 1.000000000000000000, 0.8660254037844387076, 1.000000000000000000, 0.8660254037844387076, 1.000000000000000000, 0.8660254037844387076, 1.000000000000000000, 0.8660254037844387076, 1.000000000000000000, 0.8660254037844387076, 1.000000000000000000, 0.8660254037844387076, 1.000000000000000000, 0.8660254037844387076, 1.000000000000000000, 0.8660254037844387076, 1.000000000000000000, 0.8660254037844387076, 1.000000000000000000, 0.8660254037844387076, 1.000000000000000000, 0.8660254037844387076, 1.000000000000000000, 0.8660254037844387076, 1.000000000000000000, 0.8660254037844387076, 1.000000000000000000, 0.8660254037844387076, 1.000000000000000000, 0.8660254037844387076, 1.000000000000000000, 0.8660254037844387076, 1.000000000000000000, 0.8660254037844387076, 1.000000000000000000, 0.8660254037844387076, 1.000000000000000000, 0.8660254037844387076, 1.000000000000000000, 0.8660254037844387076, 1.000000000000000000, 0.8660254037844387076, 1.000000000000000000, 0.8660254037844387076, 1.000000000000000000, 0.8660254037844387076, 1.000000000000000000, 0.8660254037844387076, 1.000000000000000000, 0.8660254037844387076, 1.000000000000000000, 0.8660254037844387076, 1.000000000000000000, 0.8660254037844387076, 1.000000000000000000, 0.8660254037844387076, 1.000000000000000000, 0.8660254037844387076, 1.000000000000000000, 0.8660254037844387076, 1.000000000000000000, 0.8660254037844387076, 1.000000000000000000, 0.8660254037844387076, 1.000000000000000000, 0.8660254037844387076, 1.000000000000000000, 0.8660254037844387076, 1.000000000000000000, 0.8660254037844387076, 1.000000000000000000, 0.8660254037844387076, 1.000000000000000000, 0.8660254037844387076, 1.000000000000000000, 0.8660254037844387076, 1.000000000000000000, 0.8660254037844387076, 1.000000000000000000, 0.8660254037844387076, 1.000000000000000000, 0.8660254037844387076, 1.000000000000000000, 0.8660254037844387076, 1.000000000000000000, 0.8660254037844387076, 1.000000000000000000, 0.8660254037844387076, 1.000000000000000000, 0.8660254037844387076, 1.000000000000000000, 0.8660254037844387076, 1.000000000000000000, 0.8660254037844387076, 1.000000000000000000, 0.8660254037844387076, 1.000000000000000000, 0.8660254037844387076, 1.000000000000000000, 0.9548847207714133978, 0.9401541335272454170) ) ) 
 REPRESENTATION_ITEM ( '' )  SURFACE ( )  );
#34961 = CARTESIAN_POINT ( 'NONE',  ( 30.58849351077567036, -7.209453229046482114, 159.5969823328619555 ) ) ;
#34962 = AXIS2_PLACEMENT_3D ( 'NONE', #2257, #13647, #36375 ) ;
#34963 = CARTESIAN_POINT ( 'NONE',  ( -3.257655550457281723, 65.89768628210143220, 15.46528703574804986 ) ) ;
#34964 = CARTESIAN_POINT ( 'NONE',  ( -13.49999999999998401, 194.7875000012290343, 23.38268590217985476 ) ) ;
#34965 = CARTESIAN_POINT ( 'NONE',  ( 10.31873187879411091, 3.604726614523236616, -8.278124999385530813 ) ) ;
#34966 = LINE ( 'NONE', #31938, #29773 ) ;
#34967 = CARTESIAN_POINT ( 'NONE',  ( -47.03497103062156981, 204.4285982733020148, -3.350049139982115509 ) ) ;
#34968 = DIRECTION ( 'NONE',  ( -0.000000000000000000, 1.000000000000000000, -0.000000000000000000 ) ) ;
#34969 = CARTESIAN_POINT ( 'NONE',  ( -12.53471296425194836, 40.02268628210143930, 2.311890736173176641 ) ) ;
#34970 = CARTESIAN_POINT ( 'NONE',  ( -27.00000000000000355, 195.9500000000000171, 0.000000000000000000 ) ) ;
#34971 = CARTESIAN_POINT ( 'NONE',  ( 15.00000000000000000, 240.0625000000000000, -3.464101615137752610 ) ) ;
#34972 = CARTESIAN_POINT ( 'NONE',  ( 5.233372021372432847, 9.547686282101452093, 8.152565276336710909 ) ) ;
#34973 = CARTESIAN_POINT ( 'NONE',  ( 15.24356964374999990, 246.7093750006145569, 0.000000000000000000 ) ) ;
#34974 = ORIENTED_EDGE ( 'NONE', *, *, #9936, .T. ) ;
#34975 = CARTESIAN_POINT ( 'NONE',  ( 21.00000000000000000, 6.928203230275506996, -7.762500000000014388 ) ) ;
#34977 = CARTESIAN_POINT ( 'NONE',  ( 25.21024869186586059, -3.464101615137884060, 166.9656422296849030 ) ) ;
#34976 = PRODUCT ( 'follower spring', 'follower spring', '', ( #14918 ) ) ;
#34978 = CARTESIAN_POINT ( 'NONE',  ( 20.99999999999999645, 185.0294372515228645, 0.000000000000000000 ) ) ;
#34979 = CARTESIAN_POINT ( 'NONE',  ( 13.44051670066911086, 5.407089921784856479, -4.265624999385542182 ) ) ;
#34980 = CARTESIAN_POINT ( 'NONE',  ( 28.02930337212723089, -5.407089921784859143, 166.1637690562780278 ) ) ;
#34981 = CARTESIAN_POINT ( 'NONE',  ( 15.00000000000000178, 240.1374999999999886, 3.464101615137757051 ) ) ;
#34982 = CARTESIAN_POINT ( 'NONE',  ( 13.50000000000001421, 199.7000000000000171, 23.38268590217984055 ) ) ;
#34983 = CARTESIAN_POINT ( 'NONE',  ( 12.53471296425194659, 63.02268628210144641, -2.311890736173178418 ) ) ;
#34984 = ORIENTED_EDGE ( 'NONE', *, *, #26533, .F. ) ;
#34985 = AXIS2_PLACEMENT_3D ( 'NONE', #20678, #25606, #17842 ) ;
#34986 = VERTEX_POINT ( 'NONE', #27852 ) ;
#34987 = CARTESIAN_POINT ( 'NONE',  ( 28.51246655749191561, 5.725135026351853007, 159.7765254096146919 ) ) ;
#34988 = DIRECTION ( 'NONE',  ( 0.000000000000000000, 0.000000000000000000, 1.000000000000000000 ) ) ;
#34989 = CARTESIAN_POINT ( 'NONE',  ( 26.75643035624999655, 7.049594010296217766E-16, -7.115624999385477878 ) ) ;
#34990 = PRODUCT_DEFINITION_CONTEXT ( 'detailed design', #11249, 'design' ) ;
#34991 = CARTESIAN_POINT ( 'NONE',  ( 8.927990412390371944, 30.92731371789853867, 13.04141134922778811 ) ) ;
#34992 = CARTESIAN_POINT ( 'NONE',  ( 26.99999999999999645, 7.347880794884117764E-16, -5.118749998770960374 ) ) ;
#34993 = CARTESIAN_POINT ( 'NONE',  ( 26.75643035624999655, 240.6718750006145910, -3.323476615752271712 ) ) ;
#34994 = AXIS2_PLACEMENT_3D ( 'NONE', #23257, #118, #23069 ) ;
#34995 = CARTESIAN_POINT ( 'NONE',  ( -66.81919563604516554, 214.5000000000000284, -0.1155267958017627827 ) ) ;
#34996 = DIRECTION ( 'NONE',  ( 1.000000000000000000, 0.000000000000000000, 0.000000000000000000 ) ) ;
#34997 = CARTESIAN_POINT ( 'NONE',  ( 24.43404934156608022, 3.604726614523240613, 160.8882913061285080 ) ) ;
#34998 = CARTESIAN_POINT ( 'NONE',  ( 8.710071997420211432, 19.71481371789854720, -3.796722387233181895 ) ) ;
#34999 = CARTESIAN_POINT ( 'NONE',  ( -64.45163769728823411, 215.6869285224996986, -3.149950860017881382 ) ) ;
#35000 = CARTESIAN_POINT ( 'NONE',  ( -44.45461230271183695, 207.6069050685336492, -8.469044688360751749 ) ) ;
#35001 = SHAPE_DEFINITION_REPRESENTATION ( #9273, #36285 ) ;
#35002 = CARTESIAN_POINT ( 'NONE',  ( 24.79149224591586886, 195.0000000000000284, -10.85399214561028280 ) ) ;
#35003 = CARTESIAN_POINT ( 'NONE',  ( -1.926257025242585782E-15, 196.1468750006145285, -31.45816453501075927 ) ) ;
#35004 = CARTESIAN_POINT ( 'NONE',  ( 6.092822981423662299, 132.4148137178985678, 14.25334919248795096 ) ) ;
#35005 = CARTESIAN_POINT ( 'NONE',  ( -63.45461230271182274, 208.1428034533959135, -6.469044688360754414 ) ) ;
#35006 =( BOUNDED_CURVE ( )  B_SPLINE_CURVE ( 2, ( #36831, #10314, #13349, #4624, #21704, #12981, #7852 ),
 .UNSPECIFIED., .F., .F. ) 
 B_SPLINE_CURVE_WITH_KNOTS ( ( 3, 2, 2, 3 ),
 ( 0.3695652173913033800, 0.3768115942028977816, 0.3840579710144920722, 0.3913043478260864738 ),
 .UNSPECIFIED. ) 
 CURVE ( )  GEOMETRIC_REPRESENTATION_ITEM ( )  RATIONAL_B_SPLINE_CURVE ( ( 1.000000000000017319, 0.8660254037844211661, 1.000000000000000000, 0.8660254037844387076, 1.000000000000000000, 0.8660254037844479225, 0.9999999999999907851 ) ) 
 REPRESENTATION_ITEM ( '' )  );
#35007 = ORIENTED_EDGE ( 'NONE', *, *, #25622, .F. ) ;
#35008 = CARTESIAN_POINT ( 'NONE',  ( -8.715434833791929847, 50.66018628210144925, -8.962234695871762469 ) ) ;
#35009 = CARTESIAN_POINT ( 'NONE',  ( 26.99999999999999645, 7.347880794884117764E-16, -6.074999999999997513 ) ) ;
#35010 = CARTESIAN_POINT ( 'NONE',  ( 26.52314049301468657, 1.665113505852782616, -8.000000000000000000 ) ) ;
#35011 = CARTESIAN_POINT ( 'NONE',  ( 27.50636891564131759, 5.407089921784856479, 160.1866008677275772 ) ) ;
#35012 = CARTESIAN_POINT ( 'NONE',  ( 15.00000000000000000, 0.000000000000000000, -1.743749998770943721 ) ) ;
#35013 = CARTESIAN_POINT ( 'NONE',  ( 13.44051670066911086, 5.407089921784862696, -8.371874999385548577 ) ) ;
#35014 =( NAMED_UNIT ( * ) SI_UNIT ( $, .STERADIAN. ) SOLID_ANGLE_UNIT ( ) );
#35015 = CARTESIAN_POINT ( 'NONE',  ( 19.68408634441910721, 5.407089921784857367, -1.190624999385520022 ) ) ;
#35016 = CARTESIAN_POINT ( 'NONE',  ( -7.954856959092191815, 59.57268628210145067, -5.529263428287477744 ) ) ;
#35017 = DIRECTION ( 'NONE',  ( -0.000000000000000000, -0.000000000000000000, 1.000000000000000000 ) ) ;
#35018 = CARTESIAN_POINT ( 'NONE',  ( -8.962234695871760692, 103.5601862821014549, 8.715434833791933400 ) ) ;
#35019 = CARTESIAN_POINT ( 'NONE',  ( 25.01741661114323634, 3.464101615137552770, 164.7615614613813193 ) ) ;
#35020 = DIRECTION ( 'NONE',  ( 0.000000000000000000, 0.000000000000000000, 1.000000000000000000 ) ) ;
#35021 = ORIENTED_EDGE ( 'NONE', *, *, #14244, .T. ) ;
#35022 = DIRECTION ( 'NONE',  ( 0.000000000000000000, 0.000000000000000000, -1.000000000000000000 ) ) ;
#35023 = CARTESIAN_POINT ( 'NONE',  ( 21.00000000000000000, -6.646953231504538984, -8.578124999385442706 ) ) ;
#35024 = CARTESIAN_POINT ( 'NONE',  ( 5.778771075727756162E-15, 195.4718750006145171, 31.45816453501076637 ) ) ;
#35025 = CARTESIAN_POINT ( 'NONE',  ( 31.05913452161298949, -7.209453229046482114, 164.9764337025573866 ) ) ;
#35026 = CARTESIAN_POINT ( 'NONE',  ( 25.09258843915631587, -3.464101615137761048, 165.6207793872610523 ) ) ;
#35027 = DIRECTION ( 'NONE',  ( 0.000000000000000000, 0.000000000000000000, -1.000000000000000000 ) ) ;
#35028 = CARTESIAN_POINT ( 'NONE',  ( 26.99999999999999645, 248.0125000000000171, -3.464101615137755275 ) ) ;
#35029 = CARTESIAN_POINT ( 'NONE',  ( -27.24356964374999279, 197.5906250006144944, 15.72908226750539384 ) ) ;
#35030 = CARTESIAN_POINT ( 'NONE',  ( -7.228626920338836470, 109.1273137178985735, -10.49813415416005213 ) ) ;
#35031 = CARTESIAN_POINT ( 'NONE',  ( -11.61527771782819940, 131.7351862821014663, 4.622313124798574258 ) ) ;
#35033 = ORIENTED_EDGE ( 'NONE', *, *, #16847, .F. ) ;
#35032 = ORIENTED_EDGE ( 'NONE', *, *, #34869, .T. ) ;
#35034 = CARTESIAN_POINT ( 'NONE',  ( -27.24356964374999990, 196.6156250006145285, -15.72908226750537786 ) ) ;
#35035 = CARTESIAN_POINT ( 'NONE',  ( 26.75643035624999655, 242.7718750006145001, -7.049594010296217766E-16 ) ) ;
#35036 = CARTESIAN_POINT ( 'NONE',  ( 15.46528703574811736, 102.8023137178985422, -3.257655550456947768 ) ) ;
#35037 = CARTESIAN_POINT ( 'NONE',  ( 23.87821517812500005, -4.985214923628404016, -3.703124999385493332 ) ) ;
#35038 = CARTESIAN_POINT ( 'NONE',  ( 23.87821517812500005, 247.7593750006145399, 4.985214923628404016 ) ) ;
#35039 = CARTESIAN_POINT ( 'NONE',  ( 27.00000000000000355, 195.8375000012290457, -3.306546357697854128E-15 ) ) ;
#35040 = CARTESIAN_POINT ( 'NONE',  ( -8.843639120294245259, 80.66481371789856780, -3.474262827703533230 ) ) ;
#35041 = CARTESIAN_POINT ( 'NONE',  ( 13.44051670066911619, -5.407089921784859143, -5.015624999385570604 ) ) ;
#35042 = CARTESIAN_POINT ( 'NONE',  ( 15.24356964374999990, 241.6093750006145342, -3.323476615752268604 ) ) ;
#35043 = CARTESIAN_POINT ( 'NONE',  ( 7.228626920338837358, 40.12731371789853796, 10.49813415416005036 ) ) ;
#35044 = CARTESIAN_POINT ( 'NONE',  ( 22.56230152254345356, -3.464101615138130530, -1.499999998770985554 ) ) ;
#35045 = CARTESIAN_POINT ( 'NONE',  ( 2.311890736173175753, 102.1226862821014691, 12.53471296425194836 ) ) ;
#35046 = CARTESIAN_POINT ( 'NONE',  ( 22.56230152254410370, 3.464101615137755275, -5.924999998771004250 ) ) ;
#35047 = CARTESIAN_POINT ( 'NONE',  ( -63.65997103062157692, 213.8393509191290889, 2.350049139982164359 ) ) ;
#35048 = CARTESIAN_POINT ( 'NONE',  ( -2.660918448318275509, 139.4976862821014549, 12.46528703574805874 ) ) ;
#35049 = CARTESIAN_POINT ( 'NONE',  ( 25.00761158997698175, 3.464101615137542112, 164.6494895566216314 ) ) ;
#35050 = CARTESIAN_POINT ( 'NONE',  ( 6.092822981423978490, 89.18518628210145494, -14.25334919248782306 ) ) ;
#35051 = CARTESIAN_POINT ( 'NONE',  ( 26.99999999999999645, 248.3875000000000171, 3.464101615137751278 ) ) ;
#35052 = CARTESIAN_POINT ( 'NONE',  ( 21.00000000000000355, 0.000000000000000000, 50.00000000000001421 ) ) ;
#35053 = DIRECTION ( 'NONE',  ( 1.000000000000000000, 0.000000000000000000, 0.000000000000000000 ) ) ;
#35054 = CARTESIAN_POINT ( 'NONE',  ( -7.954856959092191815, 114.7726862821014322, -5.529263428287477744 ) ) ;
#35055 = CARTESIAN_POINT ( 'NONE',  ( 35.44346792208517627, 0.000000000000000000, 169.1947408000190194 ) ) ;
#35056 = CARTESIAN_POINT ( 'NONE',  ( 5.770363421893814682, 9.835186282101449962, 14.38691631536207183 ) ) ;
#35057 = CARTESIAN_POINT ( 'NONE',  ( -13.62178482187498396, 195.4343750006145228, 23.59362340125808188 ) ) ;
#35058 = CARTESIAN_POINT ( 'NONE',  ( 21.00000000000000000, 242.2093750006145285, 6.646953231504538984 ) ) ;
#35059 = ORIENTED_EDGE ( 'NONE', *, *, #4506, .T. ) ;
#35060 = CARTESIAN_POINT ( 'NONE',  ( 31.43662783238875136, 7.209453229046475009, 169.2912019886672681 ) ) ;
#35061 = CARTESIAN_POINT ( 'NONE',  ( -7.954856959092191815, 50.37268628210144783, -5.529263428287477744 ) ) ;
#35062 = CARTESIAN_POINT ( 'NONE',  ( 21.00000000000000000, 6.646953231504538984, -0.2531249993854407521 ) ) ;
#35063 = CARTESIAN_POINT ( 'NONE',  ( 22.60769515458671108, 241.5825961894323086, 6.000000000000010658 ) ) ;
#35064 = CARTESIAN_POINT ( 'NONE',  ( 18.00000000000000355, -5.196152422706632912, -4.818749998770965881 ) ) ;
#35065 = DIRECTION ( 'NONE',  ( 1.000000000000000000, 0.000000000000000000, 0.000000000000000000 ) ) ;
#35066 = CARTESIAN_POINT ( 'NONE',  ( -7.946041369334237991, 195.0000000000000000, 26.05901981062767092 ) ) ;
#35067 = ADVANCED_FACE ( 'NONE', ( #20457 ), #11720, .T. ) ;
#35068 = CARTESIAN_POINT ( 'NONE',  ( 15.00000000000000000, 0.000000000000000000, -0.4500000000000059508 ) ) ;
#35069 = CARTESIAN_POINT ( 'NONE',  ( -8.843639120294245259, 34.66481371789854649, -3.474262827703533230 ) ) ;
#35070 = CARTESIAN_POINT ( 'NONE',  ( 15.00000000000000355, 7.347880794884112834E-16, -8.000000000000000000 ) ) ;
#35071 = EDGE_LOOP ( 'NONE', ( #20368, #16570, #1748, #36796 ) ) ;
#35072 = CARTESIAN_POINT ( 'NONE',  ( 19.95811728174978228, 239.6067735352071679, -5.908847637349563087 ) ) ;
#35073 = CARTESIAN_POINT ( 'NONE',  ( -0.1745138560722763466, 45.58981371789855075, -12.50000000000000355 ) ) ;
#35074 = CARTESIAN_POINT ( 'NONE',  ( 15.24356964375000167, -3.323476615752272600, -9.215624999385486404 ) ) ;
#35075 = CARTESIAN_POINT ( 'NONE',  ( 6.932735513424201024, 9.652313717898541867, -10.69584247140429412 ) ) ;
#35076 = DIRECTION ( 'NONE',  ( 1.000000000000000000, 0.000000000000000000, 0.000000000000000000 ) ) ;
#35077 = VERTEX_POINT ( 'NONE', #37305 ) ;
#35078 = CARTESIAN_POINT ( 'NONE',  ( 16.56230152254411792, -7.209453229046482114, -4.584374999385491201 ) ) ;
#35079 = VERTEX_POINT ( 'NONE', #17049 ) ;
#35080 = CARTESIAN_POINT ( 'NONE',  ( 13.62178482187501416, 198.1531250006145228, 23.59362340125806767 ) ) ;
#35081 = CARTESIAN_POINT ( 'NONE',  ( 34.26382187998621731, 5.407089921784862696, 165.7877139618832985 ) ) ;
#35082 = CARTESIAN_POINT ( 'NONE',  ( -31.39211230271182984, 203.5309553116391612, 1.857196546604092280 ) ) ;
#35083 = CARTESIAN_POINT ( 'NONE',  ( 15.00000000000000000, 245.5562500012290457, 0.000000000000000000 ) ) ;
#35084 = SURFACE_SIDE_STYLE ('',( #3628 ) ) ;
#35085 = ADVANCED_FACE ( 'NONE', ( #22550 ), #34471, .F. ) ;
#35086 = CARTESIAN_POINT ( 'NONE',  ( -25.03348993865347438, 194.9999999999999432, 10.48541407139706649 ) ) ;
#35087 = CARTESIAN_POINT ( 'NONE',  ( -58.30877896937849414, 211.0902445701383101, -4.530955311639234040 ) ) ;
#35088 = CARTESIAN_POINT ( 'NONE',  ( -35.35788769728823411, 216.4690446883607535, 1.857196546604031662 ) ) ;
#35089 = CARTESIAN_POINT ( 'NONE',  ( 28.29077060037018043, 5.407089921784856479, 169.1523531505532674 ) ) ;
#35090 = ORIENTED_EDGE ( 'NONE', *, *, #18405, .F. ) ;
#35091 = CARTESIAN_POINT ( 'NONE',  ( 0.000000000000000000, 148.0000000000000000, 0.000000000000000000 ) ) ;
#35092 = AXIS2_PLACEMENT_3D ( 'NONE', #7987, #10265, #7805 ) ;
#35093 = CARTESIAN_POINT ( 'NONE',  ( 6.092822981423662299, 12.81481371789855217, 14.25334919248795096 ) ) ;
#35094 = CARTESIAN_POINT ( 'NONE',  ( -55.74330436395489841, 210.1155267958016850, -8.500000000000003553 ) ) ;
#35095 = CARTESIAN_POINT ( 'NONE',  ( 3.474262827703335166, 129.4351862821014549, 8.843639120294326972 ) ) ;
#35096 = CARTESIAN_POINT ( 'NONE',  ( -7.228626920339069173, 38.87268628210144072, 10.49813415415989581 ) ) ;
#35097 = CARTESIAN_POINT ( 'NONE',  ( 13.56230152254410726, 5.196152422706636465, -4.125000000000045297 ) ) ;
#35098 = ORIENTED_EDGE ( 'NONE', *, *, #18426, .F. ) ;
#35099 = CARTESIAN_POINT ( 'NONE',  ( -46.83705436395489841, 205.3262412349647548, -4.842901733360204908 ) ) ;
#35100 = CARTESIAN_POINT ( 'NONE',  ( 19.56230152254411081, 5.196152422706631135, -5.437499998771022192 ) ) ;
#35101 = CARTESIAN_POINT ( 'NONE',  ( -1.715153634034234598, 14.72268628210143859, -9.534712964251941258 ) ) ;
#35102 = AXIS2_PLACEMENT_3D ( 'NONE', #34884, #17277, #8924 ) ;
#35103 = CARTESIAN_POINT ( 'NONE',  ( -13.62178482187498396, 195.4343750006145228, 23.59362340125808188 ) ) ;
#35104 = CARTESIAN_POINT ( 'NONE',  ( 0.000000000000000000, 200.0000000000000000, 0.000000000000000000 ) ) ;
#35105 = CARTESIAN_POINT ( 'NONE',  ( 20.99999999999999289, 244.4874999999999829, -5.999999999999997335 ) ) ;
#35106 = CARTESIAN_POINT ( 'NONE',  ( 25.25273711656209841, 3.464101615137667789, 167.4512871462289638 ) ) ;
#35107 = CARTESIAN_POINT ( 'NONE',  ( 34.40478479951106294, 5.196152422706631135, 168.7962516286712571 ) ) ;
#35108 = CARTESIAN_POINT ( 'NONE',  ( 18.12178482187499640, 244.8343750006145285, -4.985214923628404904 ) ) ;
#35109 = CARTESIAN_POINT ( 'NONE',  ( 5.529263428287300108, 86.12731371789853085, 7.954856959092309943 ) ) ;
#35110 = LINE ( 'NONE', #20725, #20894 ) ;
#35111 = VERTEX_POINT ( 'NONE', #2625 ) ;
#35112 = CARTESIAN_POINT ( 'NONE',  ( -51.98288769728821990, 203.5309553116391612, -1.857196546604028775 ) ) ;
#35113 = CARTESIAN_POINT ( 'NONE',  ( 18.00000000000000000, 247.2812500012290400, -5.196152422706630247 ) ) ;
#35114 = CARTESIAN_POINT ( 'NONE',  ( -0.1745138560722763466, 100.7898137178985536, -12.50000000000000355 ) ) ;
#35115 = CARTESIAN_POINT ( 'NONE',  ( 22.80587116629411426, 7.646167579472024665E-16, -2.671874999385509319 ) ) ;
#35116 = CARTESIAN_POINT ( 'NONE',  ( 24.44222019244867283, 0.000000000000000000, 160.9816845590745800 ) ) ;
#35117 = CARTESIAN_POINT ( 'NONE',  ( 15.24356964374999990, 3.323476615752268604, -2.090624999385484628 ) ) ;
#35118 = CARTESIAN_POINT ( 'NONE',  ( -7.228626920338836470, 63.12731371789855217, -10.49813415416005213 ) ) ;
#35119 = CARTESIAN_POINT ( 'NONE',  ( -27.24356964375000345, 198.5093750006145399, 0.000000000000000000 ) ) ;
#35120 = EDGE_LOOP ( 'NONE', ( #34559, #12537, #15315, #22138 ) ) ;
#35121 = ORIENTED_EDGE ( 'NONE', *, *, #6712, .F. ) ;
#35122 = CARTESIAN_POINT ( 'NONE',  ( 18.12178482187500350, -4.985214923628407568, -5.465624999385465088 ) ) ;
#35123 = DIRECTION ( 'NONE',  ( -0.000000000000000000, -0.000000000000000000, 1.000000000000000000 ) ) ;
#35124 = CARTESIAN_POINT ( 'NONE',  ( 15.24356964374999990, 247.0093750006145115, -3.323476615752268604 ) ) ;
#35125 = CARTESIAN_POINT ( 'NONE',  ( 4.622313124798573369, 46.63518628210145067, 11.61527771782819940 ) ) ;
#35126 = CARTESIAN_POINT ( 'NONE',  ( -45.64211230271182984, 203.5309553116391896, 1.857196546604092724 ) ) ;
#35127 = CARTESIAN_POINT ( 'NONE',  ( -64.24627896937849414, 203.4690446883607535, -1.626142955000504209 ) ) ;
#35128 = CARTESIAN_POINT ( 'NONE',  ( 30.71350752933288675, 6.928203230275506996, 161.0258991035495058 ) ) ;
#35129 = CARTESIAN_POINT ( 'NONE',  ( -2.660918448318004614, 100.5023137178985593, -12.46528703574811558 ) ) ;
#35130 = CARTESIAN_POINT ( 'NONE',  ( -59.70163769728823411, 213.9548777149308592, -2.149950860017830756 ) ) ;
#35131 = CARTESIAN_POINT ( 'NONE',  ( -36.34747103062156981, 214.3500491399821044, -7.303452534266878793 ) ) ;
#35132 = CARTESIAN_POINT ( 'NONE',  ( 15.24356964375000167, -3.323476615752272600, -5.615624999385488536 ) ) ;
#35133 = CARTESIAN_POINT ( 'NONE',  ( 2.999999999999997335, 244.5000000000000000, 2.500000000000000000 ) ) ;
#35134 = CARTESIAN_POINT ( 'NONE',  ( -15.46528703574811736, 70.60231371789853938, 3.257655550456946436 ) ) ;
#35135 = CARTESIAN_POINT ( 'NONE',  ( -60.09002896937850124, 202.6965474657332038, 4.350049139982197666 ) ) ;
#35136 = ORIENTED_EDGE ( 'NONE', *, *, #1006, .F. ) ;
#35137 = CARTESIAN_POINT ( 'NONE',  ( -68.00669563604516554, 209.8844732041982013, -6.500000000000000888 ) ) ;
#35138 = CARTESIAN_POINT ( 'NONE',  ( -12.53471296425194836, 95.22268628210146346, 2.311890736173176641 ) ) ;
#35139 = CARTESIAN_POINT ( 'NONE',  ( 8.632099005475504683, 46.34768628210144925, 13.23911966647218996 ) ) ;
#35141 = EDGE_CURVE ( 'NONE', #28877, #1340, #13496, .T. ) ;
#35140 = CARTESIAN_POINT ( 'NONE',  ( 21.00000000000000000, 243.3624999999999829, 5.999999999999998224 ) ) ;
#35142 = CARTESIAN_POINT ( 'NONE',  ( 33.71474070067601048, 5.407089921784862696, 159.5116873639053097 ) ) ;
#35143 = VECTOR ( 'NONE', #1158, 1000.000000000000000 ) ;
#35144 = CARTESIAN_POINT ( 'NONE',  ( 13.23911966647218996, 62.44768628210144357, -8.632099005475504683 ) ) ;
#35145 = CARTESIAN_POINT ( 'NONE',  ( -56.70466238434235606, 244.2363183625454894, -7.500000000000000000 ) ) ;
#35146 = CARTESIAN_POINT ( 'NONE',  ( 19.68408634441910721, 5.407089921784857367, -8.840624999385537919 ) ) ;
#35147 = CARTESIAN_POINT ( 'NONE',  ( 27.00000000000031619, -3.464101615137567869, -2.006249998770949006 ) ) ;
#35148 = CARTESIAN_POINT ( 'NONE',  ( -49.80580436395490551, 216.5000000000000000, 0.1155267958017343610 ) ) ;
#35149 = CARTESIAN_POINT ( 'NONE',  ( 10.59851679596256702, -1.739360772546590050, -9.999999999999994671 ) ) ;
#35150 = CARTESIAN_POINT ( 'NONE',  ( 11.61527771782819940, 44.33518628210145351, -4.622313124798573369 ) ) ;
#35151 = CARTESIAN_POINT ( 'NONE',  ( 19.39230484541326760, 240.1924038105676686, 5.999999999999999112 ) ) ;
#35152 = CARTESIAN_POINT ( 'NONE',  ( -8.710071997420127943, 4.085186282101443744, -3.796722387233380402 ) ) ;
#35153 = CARTESIAN_POINT ( 'NONE',  ( 23.87821517812500005, 246.8593750006145342, 4.985214923628404016 ) ) ;
#35154 = ORIENTED_EDGE ( 'NONE', *, *, #30559, .F. ) ;
#35155 = CARTESIAN_POINT ( 'NONE',  ( 23.99999999999999645, 5.196152422706631135, -8.250000000000007105 ) ) ;
#35156 = CARTESIAN_POINT ( 'NONE',  ( -29.00000000000002487, 210.0000000000000000, 8.000000000000000000 ) ) ;
#35157 = EDGE_CURVE ( 'NONE', #6148, #7924, #20081, .T. ) ;
#35158 = CARTESIAN_POINT ( 'NONE',  ( 23.99999999999999645, 5.196152422706631135, -6.843749998770965348 ) ) ;
#35159 = CARTESIAN_POINT ( 'NONE',  ( 19.68408634441910721, -5.407089921784855591, -3.590624999385533478 ) ) ;
#35160 = CARTESIAN_POINT ( 'NONE',  ( 37.45053336641773711, 7.646167579472015790E-16, 166.3935290647278009 ) ) ;
#35161 =( BOUNDED_CURVE ( )  B_SPLINE_CURVE ( 2, ( #37332, #23320, #37153, #25969, #8726, #2842, #20108, #11194, #11382 ),
 .UNSPECIFIED., .F., .F. ) 
 B_SPLINE_CURVE_WITH_KNOTS ( ( 3, 2, 2, 2, 3 ),
 ( 0.7717391304347825942, 0.7753623188405797118, 0.7826086956521739468, 0.7898550724637680709, 0.7934782608695651884 ),
 .UNSPECIFIED. ) 
 CURVE ( )  GEOMETRIC_REPRESENTATION_ITEM ( )  RATIONAL_B_SPLINE_CURVE ( ( 0.9330127018922194093, 0.9330127018922194093, 1.000000000000000000, 0.8660254037844387076, 1.000000000000000000, 0.8660254037844387076, 1.000000000000000000, 0.9330127018922194093, 0.9330127018922194093 ) ) 
 REPRESENTATION_ITEM ( '' )  );
#35162 = CARTESIAN_POINT ( 'NONE',  ( 18.00000000000000000, 241.3750000000000000, -5.196152422706630247 ) ) ;
#35163 = CARTESIAN_POINT ( 'NONE',  ( -6.797719915734056428, 221.2600545691329330, 2.615526397346993992 ) ) ;
#35164 = EDGE_CURVE ( 'NONE', #7787, #12569, #24132, .T. ) ;
#35165 = CARTESIAN_POINT ( 'NONE',  ( 2.660918448318279950, 42.89768628210144641, -12.46528703574805874 ) ) ;
#35166 = EDGE_LOOP ( 'NONE', ( #10516, #3604, #6289, #35644 ) ) ;
#35167 = ORIENTED_EDGE ( 'NONE', *, *, #18419, .F. ) ;
#35168 = CARTESIAN_POINT ( 'NONE',  ( 21.00000000000016342, -4.000000000000002665, 50.00000000000000000 ) ) ;
#35169 = DIRECTION ( 'NONE',  ( 0.9961946980917462113, 0.000000000000000000, -0.08715574274765118534 ) ) ;
#35170 = CARTESIAN_POINT ( 'NONE',  ( -7.234628195640289583, 198.2200961906613372, -27.00000000000001421 ) ) ;
#35171 = CARTESIAN_POINT ( 'NONE',  ( 15.24356964375000167, -3.323476615752272600, -6.403124999385489069 ) ) ;
#35172 = CARTESIAN_POINT ( 'NONE',  ( -10.69584247140444866, 94.64768628210146062, 6.932735513423972762 ) ) ;
#35173 = CARTESIAN_POINT ( 'NONE',  ( -10.83675517735179028, 14.53981371789855892, 11.08355503943118947 ) ) ;
#35174 = EDGE_CURVE ( 'NONE', #29181, #15610, #21489, .T. ) ;
#35175 = CARTESIAN_POINT ( 'NONE',  ( 21.00000000000000000, 241.4218750006145626, 6.646953231504538984 ) ) ;
#35176 = AXIS2_PLACEMENT_3D ( 'NONE', #35052, #14413, #17264 ) ;
#35177 = CARTESIAN_POINT ( 'NONE',  ( -35.55580436395489130, 214.5000000000000284, 0.1155267958017899832 ) ) ;
#35178 = CARTESIAN_POINT ( 'NONE',  ( -4.914563035147740067, 224.9123314610253317, 2.500000000000000000 ) ) ;
#35179 = CARTESIAN_POINT ( 'NONE',  ( 24.44058602227215005, -3.604726614523244610, 160.9630059084853997 ) ) ;
#35180 = CARTESIAN_POINT ( 'NONE',  ( 0.1745138560723095977, 13.38981371789854613, 9.500000000000005329 ) ) ;
#35181 = CARTESIAN_POINT ( 'NONE',  ( -57.92038769728821990, 208.1428034533959703, 6.469044688360770401 ) ) ;
#35182 = CARTESIAN_POINT ( 'NONE',  ( -67.42038769728826253, 207.6069050685337913, 8.469044688360781947 ) ) ;
#35183 =( BOUNDED_CURVE ( )  B_SPLINE_CURVE ( 2, ( #11013, #7990, #14235, #16714, #28807, #22957, #34503, #28261, #28621 ),
 .UNSPECIFIED., .F., .F. ) 
 B_SPLINE_CURVE_WITH_KNOTS ( ( 3, 2, 2, 2, 3 ),
 ( 0.3586956521739130266, 0.3623188405797101441, 0.3695652173913043237, 0.3768115942028985588, 0.3804347826086956763 ),
 .UNSPECIFIED. ) 
 CURVE ( )  GEOMETRIC_REPRESENTATION_ITEM ( )  RATIONAL_B_SPLINE_CURVE ( ( 0.9330127018922191873, 0.9330127018922187432, 1.000000000000000000, 0.8660254037844387076, 1.000000000000000000, 0.8660254037844387076, 1.000000000000000000, 0.9330127018922188542, 0.9330127018922194093 ) ) 
 REPRESENTATION_ITEM ( '' )  );
#35184 = CARTESIAN_POINT ( 'NONE',  ( 0.000000000000000000, 0.000000000000000000, 0.000000000000000000 ) ) ;
#35185 = CARTESIAN_POINT ( 'NONE',  ( 19.20301275210649905, 194.9999999999999147, -19.02731729069157396 ) ) ;
#35186 = CARTESIAN_POINT ( 'NONE',  ( 5.778771075727756162E-15, 195.0218750006145569, 31.45816453501075927 ) ) ;
#35187 = CARTESIAN_POINT ( 'NONE',  ( -10.83675517735179028, 124.9398137178985451, 11.08355503943118947 ) ) ;
#35188 = CARTESIAN_POINT ( 'NONE',  ( -62.06919563604516554, 216.5000000000000000, -0.1155267958017906493 ) ) ;
#35189 = VERTEX_POINT ( 'NONE', #23107 ) ;
#35190 = CARTESIAN_POINT ( 'NONE',  ( 11.61527771782819940, 44.33518628210145351, -4.622313124798573369 ) ) ;
#35191 = CARTESIAN_POINT ( 'NONE',  ( 22.60769515458672885, 245.4236538117966973, -5.999999999999998224 ) ) ;
#35192 = CARTESIAN_POINT ( 'NONE',  ( 25.00000000000001421, -2.343145750507543035, 49.82535622836641664 ) ) ;
#35193 = CARTESIAN_POINT ( 'NONE',  ( 34.32918868704696536, -5.407089921784861808, 166.5348599854521296 ) ) ;
#35194 = CARTESIAN_POINT ( 'NONE',  ( 18.00000000000000355, -5.196152422706632912, -1.668749998770951981 ) ) ;
#35195 = CARTESIAN_POINT ( 'NONE',  ( 22.80587116629410360, 7.646167579472015790E-16, -2.165624999385551419 ) ) ;
#35196 = CARTESIAN_POINT ( 'NONE',  ( 8.843639120294328748, 62.73518628210145920, -3.474262827703334722 ) ) ;
#35197 = CARTESIAN_POINT ( 'NONE',  ( 18.00000000000000355, 240.6812500012290457, 5.196152422706632912 ) ) ;
#35198 = CARTESIAN_POINT ( 'NONE',  ( 20.99999999999999289, 244.9374999999999716, -5.999999999999997335 ) ) ;
#35199 = CARTESIAN_POINT ( 'NONE',  ( -2.311890736173176641, 97.52268628210144641, -12.53471296425194836 ) ) ;
#35200 = CARTESIAN_POINT ( 'NONE',  ( 13.50000000000001421, 199.3625000012290513, 23.38268590217984055 ) ) ;
#35201 = CARTESIAN_POINT ( 'NONE',  ( 10.56230152254410903, 0.000000000000000000, -4.950000000000037481 ) ) ;
#35202 = VERTEX_POINT ( 'NONE', #8333 ) ;
#35203 = CARTESIAN_POINT ( 'NONE',  ( 27.46714883140487373, 5.407089921784856479, 159.7383132535862842 ) ) ;
#35204 = VECTOR ( 'NONE', #35528, 1000.000000000000000 ) ;
#35205 = CARTESIAN_POINT ( 'NONE',  ( 18.12178482187500350, -4.985214923628407568, -9.065624999385457627 ) ) ;
#35206 = CARTESIAN_POINT ( 'NONE',  ( 25.41288579386105440, 0.000000000000000000, 169.2817949039725818 ) ) ;
#35207 = CARTESIAN_POINT ( 'NONE',  ( 27.89366724747619131, 5.407089921784862696, 164.6134410573727678 ) ) ;
#35208 = CARTESIAN_POINT ( 'NONE',  ( 33.95048549033182184, -5.196152422706635576, 163.6035867636436478 ) ) ;
#35209 = CARTESIAN_POINT ( 'NONE',  ( 7.234628195640269155, 196.5325961894323257, 27.00000000000003197 ) ) ;
#35210 = CARTESIAN_POINT ( 'NONE',  ( 23.99999999999999645, 249.4000000000000057, -5.196152422706631135 ) ) ;
#35211 = CARTESIAN_POINT ( 'NONE',  ( -27.24356964375000345, 196.6156250006145285, -15.72908226750537786 ) ) ;
#35212 = EDGE_CURVE ( 'NONE', #16024, #26922, #155, .T. ) ;
#35213 = CARTESIAN_POINT ( 'NONE',  ( 8.962234695871567070, 104.2398137178985564, 8.715434833792127023 ) ) ;
#35214 = CARTESIAN_POINT ( 'NONE',  ( -8.715434833791929847, 105.8601862821014521, -8.962234695871762469 ) ) ;
#35216 = VERTEX_POINT ( 'NONE', #31625 ) ;
#35215 = ORIENTED_EDGE ( 'NONE', *, *, #16456, .T. ) ;
#35217 = CARTESIAN_POINT ( 'NONE',  ( 13.62178482187499640, 196.0531250006145285, -23.59362340125807123 ) ) ;
#35218 = CARTESIAN_POINT ( 'NONE',  ( 10.56230152254411081, 0.000000000000000000, -9.337499998771036758 ) ) ;
#35219 = CARTESIAN_POINT ( 'NONE',  ( -11.08355503943118592, 81.23981371789855643, -10.83675517735179383 ) ) ;
#35220 = CARTESIAN_POINT ( 'NONE',  ( 21.00000000000000000, -6.646953231504538984, -3.290624999385483918 ) ) ;
#35221 = CARTESIAN_POINT ( 'NONE',  ( 26.75643035624999655, 246.9718750006145740, -3.323476615752271712 ) ) ;
#35222 = CARTESIAN_POINT ( 'NONE',  ( -1.715153634034234598, 97.52268628210144641, -9.534712964251941258 ) ) ;
#35224 = VECTOR ( 'NONE', #19892, 1000.000000000000000 ) ;
#35223 =( BOUNDED_CURVE ( )  B_SPLINE_CURVE ( 2, ( #7904, #13593, #13030, #34045, #10737, #1647, #16628 ),
 .UNSPECIFIED., .F., .F. ) 
 B_SPLINE_CURVE_WITH_KNOTS ( ( 3, 2, 2, 3 ),
 ( 0.3260869565217381361, 0.3333333333333324267, 0.3405797101449267172, 0.3478260869565210078 ),
 .UNSPECIFIED. ) 
 CURVE ( )  GEOMETRIC_REPRESENTATION_ITEM ( )  RATIONAL_B_SPLINE_CURVE ( ( 1.000000000000018430, 0.8660254037844202779, 1.000000000000000000, 0.8660254037844387076, 1.000000000000000000, 0.8660254037844520303, 0.9999999999999866773 ) ) 
 REPRESENTATION_ITEM ( '' )  );
#35225 = CARTESIAN_POINT ( 'NONE',  ( 5.727106289114498080E-15, 195.7250000012290343, 31.17691453623979214 ) ) ;
#35226 = CARTESIAN_POINT ( 'NONE',  ( 8.710071997420211432, 74.91481371789855359, -3.796722387233181895 ) ) ;
#35227 = CARTESIAN_POINT ( 'NONE',  ( 19.68408634441911076, 5.407089921784857367, -5.240624999385545379 ) ) ;
#35228 = CARTESIAN_POINT ( 'NONE',  ( 26.75643035624999655, 240.9343750006145228, 3.323476615752267271 ) ) ;
#35229 = CARTESIAN_POINT ( 'NONE',  ( -10.49813415416004858, 51.62731371789855217, 7.228626920338839135 ) ) ;
#35230 = CARTESIAN_POINT ( 'NONE',  ( 10.56230152254410903, 7.347880794884117764E-16, -10.00000000000000000 ) ) ;
#35231 = CARTESIAN_POINT ( 'NONE',  ( -11.48171059495397373, 105.2851862821014493, -4.944772684328680334 ) ) ;
#35232 = CARTESIAN_POINT ( 'NONE',  ( 16.56230152254411081, -6.928203230275506996, -6.524999998771020771 ) ) ;
#35233 = CARTESIAN_POINT ( 'NONE',  ( -36.34747103062156981, 213.3500491399821328, -5.571401726697985168 ) ) ;
#35234 = DIRECTION ( 'NONE',  ( 0.08715574274765143514, 0.000000000000000000, 0.9961946980917462113 ) ) ;
#35235 = CARTESIAN_POINT ( 'NONE',  ( 37.29365302947196881, 7.646167579472015790E-16, 164.6003786081626572 ) ) ;
#35236 = CARTESIAN_POINT ( 'NONE',  ( -8.632099005475501130, 87.74768628210144072, -13.23911966647218996 ) ) ;
#35237 = CARTESIAN_POINT ( 'NONE',  ( 19.68408634441911431, 5.407089921784862696, -4.846874999385547333 ) ) ;
#35238 = CARTESIAN_POINT ( 'NONE',  ( -12.46528703574805874, 3.797686282101447652, -2.660918448318280838 ) ) ;
#35239 = CARTESIAN_POINT ( 'NONE',  ( 3.551475717527324030E-15, 195.0000000000000000, 28.99999999999999645 ) ) ;
#35240 = CARTESIAN_POINT ( 'NONE',  ( -3.474262827703337830, 106.4351862821014691, -8.843639120294326972 ) ) ;
#35241 = CYLINDRICAL_SURFACE ( 'NONE', #20420, 5.999999999999998224 ) ;
#35242 = CARTESIAN_POINT ( 'NONE',  ( 13.04141134922759804, 8.972686282101431487, 8.927990412390657937 ) ) ;
#35243 = CARTESIAN_POINT ( 'NONE',  ( 27.24356964374999635, 195.6218750006145228, -15.72908226750539029 ) ) ;
#35244 = CARTESIAN_POINT ( 'NONE',  ( 15.24356964375000167, 242.5843750006145285, 3.323476615752272600 ) ) ;
#35245 = ORIENTED_EDGE ( 'NONE', *, *, #25170, .F. ) ;
#35246 = CARTESIAN_POINT ( 'NONE',  ( 28.17311034766084887, 5.407089921784856479, 167.8074903081294167 ) ) ;
#35247 = CARTESIAN_POINT ( 'NONE',  ( 21.00000000000000000, -6.646953231504538984, -4.078124999385484450 ) ) ;
#35248 = CARTESIAN_POINT ( 'NONE',  ( 27.24356964375000345, 199.1843750006145228, -3.336375036156643733E-15 ) ) ;
#35249 = CARTESIAN_POINT ( 'NONE',  ( 15.00000000000000000, 0.000000000000000000, -4.893749998770957177 ) ) ;
#35250 = FACE_OUTER_BOUND ( 'NONE', #2005, .T. ) ;
#35251 = CARTESIAN_POINT ( 'NONE',  ( -20.68320086892770604, 194.6619763917542798, -17.35526438333879540 ) ) ;
#35252 = CARTESIAN_POINT ( 'NONE',  ( 2.064181346179061460, 13.10231371789855181, 9.465287035748106703 ) ) ;
#35253 = CARTESIAN_POINT ( 'NONE',  ( -1.926257025242585782E-15, 198.8468750006145740, -31.45816453501076637 ) ) ;
#35254 = ORIENTED_EDGE ( 'NONE', *, *, #15502, .T. ) ;
#35255 = CARTESIAN_POINT ( 'NONE',  ( 18.12178482187499640, 247.4218750006145342, -4.985214923628404904 ) ) ;
#35256 = CARTESIAN_POINT ( 'NONE',  ( -11.61527771782809282, 43.86481371789854933, -4.622313124798832717 ) ) ;
#35257 = CARTESIAN_POINT ( 'NONE',  ( 26.75643035624999655, 3.323476615752271712, -1.678124999385453897 ) ) ;
#35258 = CARTESIAN_POINT ( 'NONE',  ( 15.50000000000000533, 130.6898137178985451, -0.1745138560722452326 ) ) ;
#35259 = CARTESIAN_POINT ( 'NONE',  ( 18.00000000000000355, -5.196152422706632912, -6.618749998770962151 ) ) ;
#35260 = DIRECTION ( 'NONE',  ( 0.1219804832088915297, 0.9925324990730154395, 0.000000000000000000 ) ) ;
#35261 = ORIENTED_EDGE ( 'NONE', *, *, #5154, .F. ) ;
#35262 = CARTESIAN_POINT ( 'NONE',  ( 16.56230152254411436, -7.209453229046482114, -3.684374999385500171 ) ) ;
#35263 = CARTESIAN_POINT ( 'NONE',  ( 27.24356964374999635, 197.8156250006145171, -15.72908226750539029 ) ) ;
#35264 = CARTESIAN_POINT ( 'NONE',  ( 37.25279877505902704, 3.604726614523243278, 164.1334123434321270 ) ) ;
#35265 = CARTESIAN_POINT ( 'NONE',  ( -32.77752896937850124, 213.3500491399821613, 5.571401726697954970 ) ) ;
#35266 = LINE ( 'NONE', #12345, #9512 ) ;
#35267 = CARTESIAN_POINT ( 'NONE',  ( -25.48128045151071319, 194.9999999999999432, -9.080314936885052646 ) ) ;
#35268 = CARTESIAN_POINT ( 'NONE',  ( -62.66294563604517265, 213.2096571498974527, -3.378800118222469617 ) ) ;
#35270 = EDGE_CURVE ( 'NONE', #9065, #5908, #5653, .T. ) ;
#35269 = CARTESIAN_POINT ( 'NONE',  ( 1.120210788295102201E-13, 197.1875000000000568, -27.00000000000000711 ) ) ;
#35271 = CARTESIAN_POINT ( 'NONE',  ( 24.87364111904954811, 0.000000000000000000, 165.9128483146287465 ) ) ;
#35272 = ORIENTED_EDGE ( 'NONE', *, *, #3200, .T. ) ;
#35273 = CARTESIAN_POINT ( 'NONE',  ( 21.00000000000000000, 248.7624999999999886, 5.999999999999998224 ) ) ;
#35274 = CARTESIAN_POINT ( 'NONE',  ( -3.257655550456946880, 8.502313717898553946, -15.46528703574811736 ) ) ;
#35275 = CARTESIAN_POINT ( 'NONE',  ( -64.05580436395490551, 218.5000000000000000, 0.1155267958017064944 ) ) ;
#35276 = CARTESIAN_POINT ( 'NONE',  ( 7.954856959092191815, 137.7726862821014606, 5.529263428287477744 ) ) ;
#35277 = CARTESIAN_POINT ( 'NONE',  ( 15.00000000000000000, 246.4562500012290513, 0.000000000000000000 ) ) ;
#35278 = CARTESIAN_POINT ( 'NONE',  ( -8.962234695871760692, 29.96018628210143930, 8.715434833791933400 ) ) ;
#35279 = CARTESIAN_POINT ( 'NONE',  ( 10.56230152254411259, 3.464101615137757051, -6.337500000000034106 ) ) ;
#35280 = VERTEX_POINT ( 'NONE', #14384 ) ;
#35281 = CARTESIAN_POINT ( 'NONE',  ( -33.97247103062156270, 206.6499508600178672, 5.571401726697986057 ) ) ;
#35282 = CARTESIAN_POINT ( 'NONE',  ( -14.38691631536207183, 122.5351862821014493, 5.770363421893814682 ) ) ;
#35283 = PLANE ( 'NONE',  #15748 ) ;
#35284 = CARTESIAN_POINT ( 'NONE',  ( -0.1745138560723084320, 137.5898137178985792, -9.500000000000005329 ) ) ;
#35285 = CARTESIAN_POINT ( 'NONE',  ( 13.62178482187501416, 198.1531250006145228, 23.59362340125806767 ) ) ;
#35286 = CARTESIAN_POINT ( 'NONE',  ( 7.234628195640322446, 197.9950961906613429, 26.99999999999999645 ) ) ;
#35287 = CARTESIAN_POINT ( 'NONE',  ( 20.96920819138947323, -4.251017401976773691, -9.999999999999996447 ) ) ;
#35288 = CARTESIAN_POINT ( 'NONE',  ( 27.00000000000000355, 197.5250000000000057, -3.306546357697854128E-15 ) ) ;
#35289 = EDGE_CURVE ( 'NONE', #18997, #24079, #31643, .T. ) ;
#35290 = CARTESIAN_POINT ( 'NONE',  ( 36.63838227223424582, -3.464101615138058143, 159.9052478282085588 ) ) ;
#35291 = CARTESIAN_POINT ( 'NONE',  ( 26.75643035624999655, 242.8468750006145456, 3.323476615752267715 ) ) ;
#35292 = CARTESIAN_POINT ( 'NONE',  ( -3.474262827703527901, 69.16481371789853938, 8.843639120294245259 ) ) ;
#35293 = LINE ( 'NONE', #11617, #37215 ) ;
#35294 = ORIENTED_EDGE ( 'NONE', *, *, #24986, .F. ) ;
#35295 = CARTESIAN_POINT ( 'NONE',  ( 21.00000000000000000, 245.4437500012290059, -6.928203230275506996 ) ) ;
#35296 = CARTESIAN_POINT ( 'NONE',  ( -2.660918448318005058, 100.5023137178985593, -12.46528703574811558 ) ) ;
#35297 = CARTESIAN_POINT ( 'NONE',  ( 10.31873187879410736, 0.000000000000000000, -3.796874999385524418 ) ) ;
#35298 = CARTESIAN_POINT ( 'NONE',  ( 36.81974367828161121, -3.604726614523235284, 159.1835699372887802 ) ) ;
#35299 = CARTESIAN_POINT ( 'NONE',  ( 26.75643035624999655, 3.323476615752271712, -4.490624999385484095 ) ) ;
#35300 = CARTESIAN_POINT ( 'NONE',  ( -8.962234695871565293, 62.83981371789855785, -8.715434833792128799 ) ) ;
#35301 = CARTESIAN_POINT ( 'NONE',  ( -13.62178482187500528, 197.9843750006145626, -23.59362340125807123 ) ) ;
#35302 = ADVANCED_FACE ( 'NONE', ( #28587 ), #19903, .T. ) ;
#35303 = VERTEX_POINT ( 'NONE', #712 ) ;
#35304 = CIRCLE ( 'NONE', #30495, 8.000000000000000000 ) ;
#35305 = ORIENTED_EDGE ( 'NONE', *, *, #2652, .F. ) ;
#35306 = CARTESIAN_POINT ( 'NONE',  ( 26.75643035624999655, 3.323476615752271268, -4.828124999385488003 ) ) ;
#35307 = CARTESIAN_POINT ( 'NONE',  ( 22.56230152254410370, 7.347880794884117764E-16, -6.412499998770998744 ) ) ;
#35308 = CARTESIAN_POINT ( 'NONE',  ( 26.75643035624999655, 246.3343750006145285, 3.323476615752267715 ) ) ;
#35309 = CARTESIAN_POINT ( 'NONE',  ( 2.660918448318279950, 33.69768628210145067, -12.46528703574805697 ) ) ;
#35310 = CARTESIAN_POINT ( 'NONE',  ( -39.11086230271183695, 213.1499508600178387, -5.686928522499747451 ) ) ;
#35311 = CARTESIAN_POINT ( 'NONE',  ( 18.34109276191939841, 217.0904193015636281, -5.392997762649389237 ) ) ;
#35312 = CARTESIAN_POINT ( 'NONE',  ( -35.54836230271182984, 206.0451222850691977, -2.149950860017851184 ) ) ;
#35313 = CARTESIAN_POINT ( 'NONE',  ( 36.75931086529713099, 7.347880794884117764E-16, 161.2874679718108553 ) ) ;
#35314 = CARTESIAN_POINT ( 'NONE',  ( -0.1745138560722763466, 91.58981371789856496, -12.50000000000000355 ) ) ;
#35315 = CARTESIAN_POINT ( 'NONE',  ( -55.54538769728824832, 211.3212981617418222, -4.469044688360751749 ) ) ;
#35316 = AXIS2_PLACEMENT_3D ( 'NONE', #23467, #35020, #20635 ) ;
#35317 = CARTESIAN_POINT ( 'NONE',  ( -68.21205436395489130, 214.6737587650352168, 4.842901733360204908 ) ) ;
#35318 = CARTESIAN_POINT ( 'NONE',  ( 26.75643035624999655, 7.049594010296217766E-16, -7.678124999385471661 ) ) ;
#35319 = FACE_OUTER_BOUND ( 'NONE', #13882, .T. ) ;
#35320 = CARTESIAN_POINT ( 'NONE',  ( 15.50000000000000533, 57.08981371789855075, -0.1745138560722452326 ) ) ;
#35321 = CARTESIAN_POINT ( 'NONE',  ( -53.16294563604516554, 216.1378603801729241, -6.307003348498026796 ) ) ;
#35322 = EDGE_CURVE ( 'NONE', #27062, #27666, #30446, .T. ) ;
#35323 = CARTESIAN_POINT ( 'NONE',  ( -3.253724281355068545E-15, 198.9874999999999829, -27.00000000000000355 ) ) ;
#35324 = CARTESIAN_POINT ( 'NONE',  ( 0.1745138560725515708, 88.61018628210146630, -12.50000000000000355 ) ) ;
#35325 = CARTESIAN_POINT ( 'NONE',  ( -5.770363421893818234, 51.23518628210143788, -14.38691631536207005 ) ) ;
#35326 = CARTESIAN_POINT ( 'NONE',  ( 13.56230152254411792, -5.196152422706638241, -0.8250000000000479172 ) ) ;
#35327 = CARTESIAN_POINT ( 'NONE',  ( 24.43404934156608022, 3.604726614523240613, 160.8882913061285080 ) ) ;
#35328 = CARTESIAN_POINT ( 'NONE',  ( -0.1745138560725817967, 47.21018628210144641, 15.50000000000000533 ) ) ;
#35329 = ADVANCED_FACE ( 'NONE', ( #16026 ), #26682, .T. ) ;
#35330 = CARTESIAN_POINT ( 'NONE',  ( 19.68408634441910721, -5.407089921784855591, -8.990624999385548932 ) ) ;
#35331 = CARTESIAN_POINT ( 'NONE',  ( 38.04237167757703020, 114.1383727779938511, 2.500000000000000000 ) ) ;
#35332 = CARTESIAN_POINT ( 'NONE',  ( -53.76413769728823411, 213.1499508600178672, 5.686928522499718142 ) ) ;
#35333 = CARTESIAN_POINT ( 'NONE',  ( 25.39981243234174002, 3.464101615137729517, 169.1323656980344481 ) ) ;
#35334 = CARTESIAN_POINT ( 'NONE',  ( 8.962234695871762469, 16.16018628210144570, -8.715434833791931624 ) ) ;
#35335 = CARTESIAN_POINT ( 'NONE',  ( 9.534712964251941258, 7.822686282101448896, -1.715153634034235708 ) ) ;
#35336 = CARTESIAN_POINT ( 'NONE',  ( 20.99999999999999645, 247.7218750006145456, 6.646953231504538984 ) ) ;
#35337 =( GEOMETRIC_REPRESENTATION_CONTEXT ( 3 ) GLOBAL_UNCERTAINTY_ASSIGNED_CONTEXT ( ( #25038 ) ) GLOBAL_UNIT_ASSIGNED_CONTEXT ( ( #33824, #28129, #13740 ) ) REPRESENTATION_CONTEXT ( 'NONE', 'WORKASPACE' ) );
#35338 = ORIENTED_EDGE ( 'NONE', *, *, #664, .F. ) ;
#35339 = CARTESIAN_POINT ( 'NONE',  ( 21.00000000000000000, -6.928203230275506996, -6.187500000000013323 ) ) ;
#35340 = CARTESIAN_POINT ( 'NONE',  ( 15.24356964375000167, 242.5843750006145285, 3.323476615752272600 ) ) ;
#35341 = CYLINDRICAL_SURFACE ( 'NONE', #12959, 8.000000000000000000 ) ;
#35342 = EDGE_CURVE ( 'NONE', #4247, #18435, #870, .T. ) ;
#35343 = CARTESIAN_POINT ( 'NONE',  ( 26.99999999999999645, 197.5625000000000000, -15.58845726811990495 ) ) ;
#35344 = CARTESIAN_POINT ( 'NONE',  ( 16.56230152254411436, 7.209453229046475009, -3.853124999385534988 ) ) ;
#35345 = VECTOR ( 'NONE', #34988, 1000.000000000000000 ) ;
#35346 = CARTESIAN_POINT ( 'NONE',  ( 28.18618370907300275, -5.407089921784859143, 167.9569195128432000 ) ) ;
#35347 = CARTESIAN_POINT ( 'NONE',  ( 24.00000000000000000, 241.1500000000000057, 5.196152422706629359 ) ) ;
#35348 = DIRECTION ( 'NONE',  ( -0.000000000000000000, 1.000000000000000000, -0.000000000000000000 ) ) ;
#35349 = CIRCLE ( 'NONE', #24471, 1.000000000000002220 ) ;
#35350 = CARTESIAN_POINT ( 'NONE',  ( -10.49813415415989404, 41.17268628210143788, -7.228626920339069173 ) ) ;
#35351 = ORIENTED_EDGE ( 'NONE', *, *, #5464, .T. ) ;
#35352 = ORIENTED_EDGE ( 'NONE', *, *, #4037, .F. ) ;
#35353 = CARTESIAN_POINT ( 'NONE',  ( 26.99999999999999645, 196.7750000012290172, -15.58845726811990495 ) ) ;
#35354 = DIRECTION ( 'NONE',  ( -1.000000000000000000, 0.000000000000000000, -0.000000000000000000 ) ) ;
#35355 = CARTESIAN_POINT ( 'NONE',  ( -20.68320086892770604, 194.6619763917542514, -17.35526438333879540 ) ) ;
#35356 = DIRECTION ( 'NONE',  ( 0.000000000000000000, 0.000000000000000000, -1.000000000000000000 ) ) ;
#35357 = CARTESIAN_POINT ( 'NONE',  ( 15.24356964374999990, 0.000000000000000000, -7.340624999385481075 ) ) ;
#35358 = CARTESIAN_POINT ( 'NONE',  ( -12.50000000000000355, 95.51018628210144357, -0.1745138560725492671 ) ) ;
#35359 = CARTESIAN_POINT ( 'NONE',  ( -3.257655550456946880, 26.90231371789854364, -15.46528703574811736 ) ) ;
#35360 = CYLINDRICAL_SURFACE ( 'NONE', #18196, 6.000000000000001776 ) ;
#35361 = CARTESIAN_POINT ( 'NONE',  ( 21.00000000000000000, 240.5218750006145285, 6.646953231504538984 ) ) ;
#35362 = CARTESIAN_POINT ( 'NONE',  ( -37.33705436395491262, 206.7903428501026042, -3.378800118222489157 ) ) ;
#35363 = DIRECTION ( 'NONE',  ( 0.000000000000000000, 1.000000000000000000, 0.000000000000000000 ) ) ;
#35364 = CARTESIAN_POINT ( 'NONE',  ( 37.35088046919680949, 3.464101615137755275, 168.0491394851085545 ) ) ;
#35365 = CARTESIAN_POINT ( 'NONE',  ( -6.932735513424201912, 143.0523137178985564, 10.69584247140429412 ) ) ;
#35366 = CARTESIAN_POINT ( 'NONE',  ( -61.87872103062154849, 203.4690446883607535, 1.626142955000567936 ) ) ;
#35367 = CARTESIAN_POINT ( 'NONE',  ( -32.18377896937850124, 207.8379586601372750, 8.530955311639258909 ) ) ;
#35368 = APPLICATION_PROTOCOL_DEFINITION ( 'draft international standard', 'automotive_design', 1998, #1065 ) ;
#35369 = CARTESIAN_POINT ( 'NONE',  ( 19.39230484541326760, 241.0924038105676743, 5.999999999999999112 ) ) ;
#35370 = CARTESIAN_POINT ( 'NONE',  ( 27.24356964375000700, 198.1906250006145740, 15.72908226750537075 ) ) ;
#35371 = CARTESIAN_POINT ( 'NONE',  ( -2.908627838312453306, 124.0773137178985621, 15.53471296425188797 ) ) ;
#35372 = CARTESIAN_POINT ( 'NONE',  ( -58.90252896937850124, 206.6499508600178387, -5.571401726697954970 ) ) ;
#35373 = EDGE_CURVE ( 'NONE', #18512, #25991, #21700, .T. ) ;
#35374 = ORIENTED_EDGE ( 'NONE', *, *, #9725, .F. ) ;
#35375 = CARTESIAN_POINT ( 'NONE',  ( -12.53471296425194836, 40.02268628210143930, 2.311890736173176641 ) ) ;
#35376 = CARTESIAN_POINT ( 'NONE',  ( 21.00000000000000000, 245.2187500012290116, 5.999999999999998224 ) ) ;
#35377 = CARTESIAN_POINT ( 'NONE',  ( -3.253724281355068545E-15, 198.9874999999999829, -27.00000000000000000 ) ) ;
#35378 = CARTESIAN_POINT ( 'NONE',  ( 34.30304196422265761, 5.407089921784862696, 166.2360015760246199 ) ) ;
#35379 = CARTESIAN_POINT ( 'NONE',  ( -14.38691631536207183, 94.93518628210146915, 5.770363421893814682 ) ) ;
#35380 = CARTESIAN_POINT ( 'NONE',  ( -69.99330436395490551, 210.1155267958017134, -6.500000000000000888 ) ) ;
#35381 = CARTESIAN_POINT ( 'NONE',  ( 16.56230152254411081, 7.209453229046475009, -0.7031249993855005487 ) ) ;
#35382 =( BOUNDED_CURVE ( )  B_SPLINE_CURVE ( 2, ( #6559, #17942, #17059, #8706, #23117, #18133, #11364 ),
 .UNSPECIFIED., .F., .F. ) 
 B_SPLINE_CURVE_WITH_KNOTS ( ( 3, 2, 2, 3 ),
 ( 0.2826086956521749460, 0.2898550724637684040, 0.2971014492753618064, 0.3043478260869552643 ),
 .UNSPECIFIED. ) 
 CURVE ( )  GEOMETRIC_REPRESENTATION_ITEM ( )  RATIONAL_B_SPLINE_CURVE ( ( 0.9999999999999804601, 0.8660254037844582475, 1.000000000000000000, 0.8660254037844387076, 1.000000000000000000, 0.8660254037844623554, 0.9999999999999763522 ) ) 
 REPRESENTATION_ITEM ( '' )  );
#35383 = CARTESIAN_POINT ( 'NONE',  ( -2.064181346179269738, 65.89768628210143220, 9.465287035748067623 ) ) ;
#35384 = CARTESIAN_POINT ( 'NONE',  ( 20.99999999999995381, 241.5625000000000000, 5.999999999999998224 ) ) ;
#35385 = CARTESIAN_POINT ( 'NONE',  ( 26.99999999999999645, 7.347880794884117764E-16, -5.175000000000013145 ) ) ;
#35386 = CARTESIAN_POINT ( 'NONE',  ( 4.622313124798573369, 101.8351862821014464, 11.61527771782819940 ) ) ;
#35387 = CARTESIAN_POINT ( 'NONE',  ( 16.56230152254411792, 6.928203230275514990, -5.062500000000007994 ) ) ;
#35388 = DIRECTION ( 'NONE',  ( 0.000000000000000000, 0.000000000000000000, 1.000000000000000000 ) ) ;
#35389 = CARTESIAN_POINT ( 'NONE',  ( 23.99999999999999645, 5.196152422706631135, -5.549999999999998934 ) ) ;
#35390 = CARTESIAN_POINT ( 'NONE',  ( 33.75886329544200493, 5.407089921784857367, 160.0160109298142288 ) ) ;
#35391 = CARTESIAN_POINT ( 'NONE',  ( 26.99999999999999645, -3.464101615137751278, -0.7125000000000065725 ) ) ;
#35392 = CARTESIAN_POINT ( 'NONE',  ( 28.39493320743021698, 5.196152422706630247, 168.9456130733727548 ) ) ;
#35393 = CARTESIAN_POINT ( 'NONE',  ( 24.94717877699287811, 0.000000000000000000, 166.7533875911436780 ) ) ;
#35394 = UNCERTAINTY_MEASURE_WITH_UNIT (LENGTH_MEASURE( 1.000000000000000082E-05 ), #31975, 'distance_accuracy_value', 'NONE');
#35395 = CARTESIAN_POINT ( 'NONE',  ( 36.94560626531313829, 7.347880794884125653E-16, 163.4168341377576041 ) ) ;
#35396 = CARTESIAN_POINT ( 'NONE',  ( -69.83334449017395684, 223.2245623293732706, 7.500000000000000000 ) ) ;
#35397 = CARTESIAN_POINT ( 'NONE',  ( 15.00000000000000000, 248.6125000000000114, -3.464101615137752166 ) ) ;
#35398 = CARTESIAN_POINT ( 'NONE',  ( 27.24356964375000345, 196.4281250006145569, -3.336375036156643733E-15 ) ) ;
#35399 = CARTESIAN_POINT ( 'NONE',  ( 6.932735513424201024, 110.8523137178985394, -10.69584247140429412 ) ) ;
#35400 = CARTESIAN_POINT ( 'NONE',  ( 8.962234695871762469, 108.1601862821014635, -8.715434833791931624 ) ) ;
#35401 = ORIENTED_EDGE ( 'NONE', *, *, #15360, .T. ) ;
#35402 = CARTESIAN_POINT ( 'NONE',  ( 27.24356964375000700, 196.8406250006145513, 15.72908226750537075 ) ) ;
#35403 = CARTESIAN_POINT ( 'NONE',  ( 18.12178482187499640, 240.2218750006145171, -4.985214923628404904 ) ) ;
#35404 = CARTESIAN_POINT ( 'NONE',  ( -8.632099005475794229, 69.45231371789853370, 13.23911966647199812 ) ) ;
#35405 = AXIS2_PLACEMENT_3D ( 'NONE', #31081, #16683, #25385 ) ;
#35406 = CARTESIAN_POINT ( 'NONE',  ( 26.75643035624999655, 7.049594010296217766E-16, -4.978124999385491023 ) ) ;
#35407 = CARTESIAN_POINT ( 'NONE',  ( 21.00000000000000000, 247.2718750006145569, 6.646953231504538984 ) ) ;
#35408 =( BOUNDED_CURVE ( )  B_SPLINE_CURVE ( 2, ( #6290, #32065, #27136, #1163, #6094, #24115, #23546 ),
 .UNSPECIFIED., .F., .F. ) 
 B_SPLINE_CURVE_WITH_KNOTS ( ( 3, 2, 2, 3 ),
 ( 0.1521739130434776321, 0.1594202898550719505, 0.1666666666666662966, 0.1739130434782606427 ),
 .UNSPECIFIED. ) 
 CURVE ( )  GEOMETRIC_REPRESENTATION_ITEM ( )  RATIONAL_B_SPLINE_CURVE ( ( 1.000000000000011768, 0.8660254037844269392, 1.000000000000000000, 0.8660254037844387076, 1.000000000000000000, 0.8660254037844428154, 0.9999999999999958922 ) ) 
 REPRESENTATION_ITEM ( '' )  );
#35409 = CARTESIAN_POINT ( 'NONE',  ( -8.843639120294326972, 104.1351862821014720, 3.474262827703335166 ) ) ;
#35410 = CARTESIAN_POINT ( 'NONE',  ( 26.99999999999999645, 243.0437500012290855, 3.464101615137751278 ) ) ;
#35411 = CARTESIAN_POINT ( 'NONE',  ( -9.534712964251895073, 61.97731371789853938, -1.715153634034446428 ) ) ;
#35412 = CARTESIAN_POINT ( 'NONE',  ( 16.56230152254410726, 7.209453229046475009, -5.203124999385489780 ) ) ;
#35413 = CARTESIAN_POINT ( 'NONE',  ( 3.796722387233182339, 104.8148137178985593, 8.710071997420207879 ) ) ;
#35414 = CARTESIAN_POINT ( 'NONE',  ( 10.56230152254410903, 0.000000000000000000, -2.700000000000063238 ) ) ;
#35415 = CARTESIAN_POINT ( 'NONE',  ( 6.932735513424201024, 46.45231371789855501, -10.69584247140429412 ) ) ;
#35416 = CARTESIAN_POINT ( 'NONE',  ( 37.38683221308021842, 7.347880794884117764E-16, 168.4600697980714017 ) ) ;
#35417 = CARTESIAN_POINT ( 'NONE',  ( 11.61527771782819940, 108.7351862821014663, -4.622313124798573369 ) ) ;
#35418 = CARTESIAN_POINT ( 'NONE',  ( 13.56230152254411614, -5.196152422706632912, -7.012499998771043686 ) ) ;
#35419 = EDGE_CURVE ( 'NONE', #27676, #30489, #23857, .T. ) ;
#35420 = CARTESIAN_POINT ( 'NONE',  ( -64.64955436395490551, 213.3788001182225003, -3.209657149897400252 ) ) ;
#35421 = CARTESIAN_POINT ( 'NONE',  ( 2.660918448318279950, 134.8976862821014890, -12.46528703574805697 ) ) ;
#35422 = CARTESIAN_POINT ( 'NONE',  ( 33.99418380086066804, 5.407089921784857367, 162.7057366146619586 ) ) ;
#35423 = CARTESIAN_POINT ( 'NONE',  ( 15.46528703574804986, 91.19768628210145778, 3.257655550457285720 ) ) ;
#35424 = VECTOR ( 'NONE', #16904, 1000.000000000000000 ) ;
#35425 = PRODUCT_RELATED_PRODUCT_CATEGORY ( 'part', '', ( #23177 ) ) ;
#35426 = CARTESIAN_POINT ( 'NONE',  ( 22.80587116629411781, 3.604726614523243278, -3.084374999385516514 ) ) ;
#35427 = DIRECTION ( 'NONE',  ( 0.8083506638593009885, 0.5887012860850802110, 0.000000000000000000 ) ) ;
#35428 = CARTESIAN_POINT ( 'NONE',  ( 5.438367727407757775E-14, 198.2000000012290002, -27.00000000000000355 ) ) ;
#35429 = CARTESIAN_POINT ( 'NONE',  ( -3.253724281355068545E-15, 198.9874999999999829, -27.00000000000000000 ) ) ;
#35430 = CARTESIAN_POINT ( 'NONE',  ( 8.152565276336714462, 108.4476862821014294, -5.233372021372432847 ) ) ;
#35431 = CARTESIAN_POINT ( 'NONE',  ( 26.99999999999999645, 7.347880794884117764E-16, -2.418749998770952647 ) ) ;
#35432 = CARTESIAN_POINT ( 'NONE',  ( 13.23911966647218996, 16.44768628210144001, -8.632099005475504683 ) ) ;
#35433 = CARTESIAN_POINT ( 'NONE',  ( -13.62178482187498396, 196.3343750006145285, 23.59362340125808188 ) ) ;
#35434 = CARTESIAN_POINT ( 'NONE',  ( 21.00000000000000000, 241.0843750006145285, -6.646953231504538984 ) ) ;
#35435 = EDGE_LOOP ( 'NONE', ( #13315, #11629, #25419, #27907 ) ) ;
#35436 = CARTESIAN_POINT ( 'NONE',  ( 31.20130732697009535, 7.209453229046475009, 166.6014763038195383 ) ) ;
#35437 = B_SPLINE_CURVE_WITH_KNOTS ( 'NONE', 3,
 ( #31933, #23228, #12029, #645 ),
 .UNSPECIFIED., .F., .F.,
 ( 4, 4 ),
 ( 0.000000000000000000, 1.000000000000000000 ),
 .UNSPECIFIED. ) ;
#35438 = CARTESIAN_POINT ( 'NONE',  ( 26.75643035624999655, 3.323476615752271712, -2.578124999385477345 ) ) ;
#35439 = CARTESIAN_POINT ( 'NONE',  ( 20.99999999999999289, 242.6875000000000000, -5.999999999999997335 ) ) ;
#35440 = FACE_OUTER_BOUND ( 'NONE', #4270, .T. ) ;
#35441 = FACE_OUTER_BOUND ( 'NONE', #17240, .T. ) ;
#35442 = CARTESIAN_POINT ( 'NONE',  ( 14.99999999999941380, -3.464101615137419543, -7.556249998770961263 ) ) ;
#35443 = CARTESIAN_POINT ( 'NONE',  ( 1.069080835302379631E-14, 198.3124999999999716, 27.00000000000000000 ) ) ;
#35444 = CARTESIAN_POINT ( 'NONE',  ( -6.594114490232462877, 23.73981371789854222, 6.840914352311949109 ) ) ;
#35445 = CARTESIAN_POINT ( 'NONE',  ( -13.62178482187500528, 197.9843750006145626, -23.59362340125807123 ) ) ;
#35447 = VERTEX_POINT ( 'NONE', #7303 ) ;
#35446 = ORIENTED_EDGE ( 'NONE', *, *, #21771, .F. ) ;
#35448 = CARTESIAN_POINT ( 'NONE',  ( 18.12178482187500350, 246.2218750006145171, 4.985214923628407568 ) ) ;
#35449 = CARTESIAN_POINT ( 'NONE',  ( 4.944772684328420986, 31.21481371789855430, 11.48171059495408208 ) ) ;
#35450 = CARTESIAN_POINT ( 'NONE',  ( 15.24356964375000167, -3.323476615752272600, -2.353124999385463489 ) ) ;
#35451 = CARTESIAN_POINT ( 'NONE',  ( -8.632099005475794229, 133.8523137178985394, 13.23911966647199812 ) ) ;
#35452 = CARTESIAN_POINT ( 'NONE',  ( 21.00000000000000000, -6.928203230275506996, -7.931249998770954157 ) ) ;
#35453 = CARTESIAN_POINT ( 'NONE',  ( -9.000000000000024869, 215.5000000000000000, 6.735557395310442023E-16 ) ) ;
#35454 = ORIENTED_EDGE ( 'NONE', *, *, #26449, .T. ) ;
#35455 = CARTESIAN_POINT ( 'NONE',  ( 19.68408634441911786, -5.407089921784861808, -4.546874999385525307 ) ) ;
#35456 = ORIENTED_EDGE ( 'NONE', *, *, #20976, .F. ) ;
#35457 = CARTESIAN_POINT ( 'NONE',  ( 27.24356964374999635, 195.5656250006145171, -15.72908226750539029 ) ) ;
#35458 = CARTESIAN_POINT ( 'NONE',  ( 34.18538171151332961, 5.407089921784862696, 164.8911387336007408 ) ) ;
#35459 = AXIS2_PLACEMENT_3D ( 'NONE', #14746, #18159, #17970 ) ;
#35460 = CARTESIAN_POINT ( 'NONE',  ( -33.56919563604517265, 216.5000000000000000, -0.1155267958017906493 ) ) ;
#35461 = CARTESIAN_POINT ( 'NONE',  ( 20.99999999999997868, 245.6687500012291139, 5.999999999999999112 ) ) ;
#35462 = DIRECTION ( 'NONE',  ( 0.000000000000000000, 0.000000000000000000, 1.000000000000000000 ) ) ;
#35463 = CARTESIAN_POINT ( 'NONE',  ( -47.42336230271184405, 213.9548777149308023, 2.149950860017852960 ) ) ;
#35464 = CARTESIAN_POINT ( 'NONE',  ( 1.069080835302379631E-14, 196.9624999999999773, 27.00000000000000000 ) ) ;
#35465 = CARTESIAN_POINT ( 'NONE',  ( 34.38638464322509947, 5.407089921784857367, 167.1886127560748321 ) ) ;
#35466 = ORIENTED_EDGE ( 'NONE', *, *, #22629, .F. ) ;
#35467 = DIRECTION ( 'NONE',  ( -0.000000000000000000, 1.000000000000000000, -0.000000000000000000 ) ) ;
#35468 = CARTESIAN_POINT ( 'NONE',  ( 15.53471296425195369, 136.6226862821014549, -2.908627838312120684 ) ) ;
#35469 = CARTESIAN_POINT ( 'NONE',  ( -50.59747103062156981, 214.3500491399821044, -7.303452534266878793 ) ) ;
#35470 = CIRCLE ( 'NONE', #16128, 4.000000000000000888 ) ;
#35471 = CARTESIAN_POINT ( 'NONE',  ( -1.715153634034234598, 125.1226862821014691, -9.534712964251941258 ) ) ;
#35472 = DIRECTION ( 'NONE',  ( -4.704570066849100051E-15, 0.000000000000000000, 1.000000000000000000 ) ) ;
#35473 = CARTESIAN_POINT ( 'NONE',  ( -10.49813415415989581, 31.97268628210143859, -7.228626920339068285 ) ) ;
#35475 = EDGE_CURVE ( 'NONE', #37126, #5600, #14936, .T. ) ;
#35474 = CARTESIAN_POINT ( 'NONE',  ( 22.56230152254411792, 7.347880794884125653E-16, -6.525000000000058975 ) ) ;
#35476 = ORIENTED_EDGE ( 'NONE', *, *, #34621, .F. ) ;
#35477 = DIRECTION ( 'NONE',  ( -1.000000000000000000, 0.000000000000000000, 0.000000000000000000 ) ) ;
#35478 = CARTESIAN_POINT ( 'NONE',  ( 13.04141134922759804, 119.3726862821014265, 8.927990412390657937 ) ) ;
#35479 = FACE_BOUND ( 'NONE', #18273, .T. ) ;
#35480 = CARTESIAN_POINT ( 'NONE',  ( -9.500000000000005329, 135.2898137178985394, 0.1745138560723101806 ) ) ;
#35481 = CARTESIAN_POINT ( 'NONE',  ( 5.778771075727756162E-15, 199.0156250006145342, 31.45816453501075927 ) ) ;
#35482 = LINE ( 'NONE', #605, #20201 ) ;
#35483 = CARTESIAN_POINT ( 'NONE',  ( 21.00000000000016342, -4.000000000000002665, 50.00000000000000000 ) ) ;
#35484 = DIRECTION ( 'NONE',  ( -1.000000000000000000, 0.000000000000000000, -0.000000000000000000 ) ) ;
#35485 = FACE_OUTER_BOUND ( 'NONE', #5054, .T. ) ;
#35486 = CARTESIAN_POINT ( 'NONE',  ( -6.594114490232462877, 69.73981371789855643, 6.840914352311949109 ) ) ;
#35487 = CARTESIAN_POINT ( 'NONE',  ( 26.97716818855048260, 0.000000000000000000, 49.47706554351410801 ) ) ;
#35488 = VERTEX_POINT ( 'NONE', #3569 ) ;
#35489 = CARTESIAN_POINT ( 'NONE',  ( 26.99999999999999645, 244.8437500012290400, 3.464101615137751278 ) ) ;
#35490 = CARTESIAN_POINT ( 'NONE',  ( 2.311890736173452421, 73.47731371789856780, -12.53471296425189152 ) ) ;
#35491 = CARTESIAN_POINT ( 'NONE',  ( 10.31873187879411091, 3.604726614523240613, -3.834374999385520066 ) ) ;
#35492 = CARTESIAN_POINT ( 'NONE',  ( 33.71964321120555752, 5.407089921784857367, 159.5677233156729642 ) ) ;
#35493 = CARTESIAN_POINT ( 'NONE',  ( 15.24356964374999990, 3.323476615752268604, -3.440624999385503813 ) ) ;
#35494 = CARTESIAN_POINT ( 'NONE',  ( 2.311890736173452865, 45.87731371789854506, -12.53471296425189152 ) ) ;
#35495 = CARTESIAN_POINT ( 'NONE',  ( 13.62178482187499640, 197.0093750006145399, -23.59362340125807123 ) ) ;
#35496 = EDGE_CURVE ( 'NONE', #32744, #28968, #36096, .T. ) ;
#35497 = EDGE_LOOP ( 'NONE', ( #14287, #34035, #204, #19596 ) ) ;
#35498 = ADVANCED_FACE ( 'NONE', ( #29715 ), #30616, .F. ) ;
#35499 = VERTEX_POINT ( 'NONE', #21023 ) ;
#35500 = CARTESIAN_POINT ( 'NONE',  ( 18.12178482187499640, 4.985214923628404904, -5.615624999385476990 ) ) ;
#35501 = CARTESIAN_POINT ( 'NONE',  ( 18.12178482187500350, 245.3218750006145115, 4.985214923628407568 ) ) ;
#35502 = AXIS2_PLACEMENT_3D ( 'NONE', #31970, #17395, #17205 ) ;
#35503 = CARTESIAN_POINT ( 'NONE',  ( -4.944772684328673229, 47.78518628210144925, 11.48171059495397728 ) ) ;
#35504 = CARTESIAN_POINT ( 'NONE',  ( -32.77752896937850124, 213.3500491399821613, 5.571401726697954970 ) ) ;
#35505 = CARTESIAN_POINT ( 'NONE',  ( 16.56230152254411436, -7.209453229046475009, -0.9281249993855145153 ) ) ;
#35506 = CARTESIAN_POINT ( 'NONE',  ( -34.16294563604517265, 213.2096571498974527, -3.378800118222469617 ) ) ;
#35507 = FILL_AREA_STYLE_COLOUR ( '', #23813 ) ;
#35508 = CARTESIAN_POINT ( 'NONE',  ( 36.64165061258780298, 7.347880794884117764E-16, 159.9426051293869477 ) ) ;
#35509 = CARTESIAN_POINT ( 'NONE',  ( -12.50000000000000355, 89.28981371789855359, 0.1745138560722786503 ) ) ;
#35510 = CARTESIAN_POINT ( 'NONE',  ( -52.57663769728824832, 206.0451222850691408, 2.149950860017832532 ) ) ;
#35511 = CARTESIAN_POINT ( 'NONE',  ( -38.32663769728823411, 202.5810206699313767, 4.149950860017909804 ) ) ;
#35512 = SHAPE_REPRESENTATION ( 'pusher', ( #17215 ), #27435 ) ;
#35513 = CARTESIAN_POINT ( 'NONE',  ( 23.87821517812500005, -4.985214923628404016, -6.853124999385479477 ) ) ;
#35514 = DIRECTION ( 'NONE',  ( -0.000000000000000000, 1.000000000000000000, -0.000000000000000000 ) ) ;
#35515 = CARTESIAN_POINT ( 'NONE',  ( 8.632099005475788900, 55.65231371789855785, -13.23911966647199812 ) ) ;
#35516 = CARTESIAN_POINT ( 'NONE',  ( -52.37127896937850835, 218.5309553116392465, 2.162041339862725842 ) ) ;
#35517 = VECTOR ( 'NONE', #26997, 1000.000000000000000 ) ;
#35518 = FACE_OUTER_BOUND ( 'NONE', #18338, .T. ) ;
#35519 = CARTESIAN_POINT ( 'NONE',  ( 10.49813415415989581, 82.57268628210145778, 7.228626920339068285 ) ) ;
#35520 = CARTESIAN_POINT ( 'NONE',  ( 14.25334919248782661, 27.08518628210144996, 6.092822981423971385 ) ) ;
#35521 = EDGE_CURVE ( 'NONE', #22884, #23722, #27575, .T. ) ;
#35522 = LINE ( 'NONE', #29650, #19886 ) ;
#35523 = CARTESIAN_POINT ( 'NONE',  ( 36.89981801693102170, 3.604726614523243278, 160.0988238161606034 ) ) ;
#35524 = CARTESIAN_POINT ( 'NONE',  ( -15.46528703574804986, 49.79768628210144499, -3.257655550457287497 ) ) ;
#35525 = VECTOR ( 'NONE', #35741, 1000.000000000000000 ) ;
#35526 = CARTESIAN_POINT ( 'NONE',  ( -27.24356964375000345, 196.6156250006145285, -15.72908226750537786 ) ) ;
#35527 = DIRECTION ( 'NONE',  ( -0.000000000000000000, -0.000000000000000000, 1.000000000000000000 ) ) ;
#35528 = DIRECTION ( 'NONE',  ( 0.000000000000000000, 0.000000000000000000, 1.000000000000000000 ) ) ;
#35529 = CARTESIAN_POINT ( 'NONE',  ( -34.36830436395490551, 209.8844732041982581, 6.500000000000000888 ) ) ;
#35530 = CARTESIAN_POINT ( 'NONE',  ( -13.49999999999998401, 195.5749999999999886, 23.38268590217985476 ) ) ;
#35531 = CARTESIAN_POINT ( 'NONE',  ( 11.48171059495397728, 27.08518628210144996, 4.944772684328674117 ) ) ;
#35532 = CARTESIAN_POINT ( 'NONE',  ( 15.00000000000000000, 247.3562500012290570, 0.000000000000000000 ) ) ;
#35533 = CARTESIAN_POINT ( 'NONE',  ( 9.500000000000005329, 121.4898137178985564, -0.1745138560723090149 ) ) ;
#35534 = CARTESIAN_POINT ( 'NONE',  ( 15.24356964374999990, 245.3593750006145342, 0.000000000000000000 ) ) ;
#35535 = VERTEX_POINT ( 'NONE', #6600 ) ;
#35536 = CARTESIAN_POINT ( 'NONE',  ( 15.00000000000000000, 3.464101615137752166, -6.337500000000001243 ) ) ;
#35537 = FACE_BOUND ( 'NONE', #7819, .T. ) ;
#35538 = CARTESIAN_POINT ( 'NONE',  ( 15.00000000000000000, 3.464101615137752610, -6.731249998770955756 ) ) ;
#35539 = CARTESIAN_POINT ( 'NONE',  ( 22.80587116629410360, 7.646167579472015790E-16, -7.115624999385533833 ) ) ;
#35540 = CARTESIAN_POINT ( 'NONE',  ( 25.06974154023176382, 0.000000000000000000, 168.1542863853351548 ) ) ;
#35541 = CARTESIAN_POINT ( 'NONE',  ( -29.00000000000002487, 204.0000000000000000, 0.000000000000000000 ) ) ;
#35542 = DIRECTION ( 'NONE',  ( 1.000000000000000000, 0.000000000000000000, 1.636531581110199847E-16 ) ) ;
#35543 = ADVANCED_FACE ( 'NONE', ( #524 ), #26874, .F. ) ;
#35544 = CARTESIAN_POINT ( 'NONE',  ( -0.1745138560725500443, 47.21018628210143930, 12.50000000000000355 ) ) ;
#35545 = VERTEX_POINT ( 'NONE', #10326 ) ;
#35546 = ORIENTED_EDGE ( 'NONE', *, *, #16773, .T. ) ;
#35547 = FACE_BOUND ( 'NONE', #26103, .T. ) ;
#35548 = CARTESIAN_POINT ( 'NONE',  ( 22.56230152254546439, -3.464101615136981227, -2.062499999999976463 ) ) ;
#35549 = CARTESIAN_POINT ( 'NONE',  ( -12.50000000000000178, 143.0000000000000000, -1.385339325893353291E-13 ) ) ;
#35550 = CARTESIAN_POINT ( 'NONE',  ( 26.99999999999999645, 243.0625000000000284, -3.464101615137755275 ) ) ;
#35551 = CARTESIAN_POINT ( 'NONE',  ( 23.87821517812499650, 4.985214923628404904, -6.140624999385474680 ) ) ;
#35552 = CARTESIAN_POINT ( 'NONE',  ( -11.61527771782819940, 94.93518628210145494, 4.622313124798574258 ) ) ;
#35553 = CARTESIAN_POINT ( 'NONE',  ( 0.1745138560722461762, 22.58981371789854364, 15.50000000000000533 ) ) ;
#35554 = CARTESIAN_POINT ( 'NONE',  ( 23.99999999999999645, 243.6062500012290286, -5.196152422706631135 ) ) ;
#35555 = CARTESIAN_POINT ( 'NONE',  ( 36.79853094953357129, 7.347880794884117764E-16, 161.7357555859521199 ) ) ;
#35556 = CARTESIAN_POINT ( 'NONE',  ( -32.78497103062156981, 206.1606490808709111, -2.350049139982163027 ) ) ;
#35557 = AXIS2_PLACEMENT_3D ( 'NONE', #34464, #13449, #8507 ) ;
#35558 = CARTESIAN_POINT ( 'NONE',  ( 15.00000000000000000, 0.000000000000000000, -3.599999999999992095 ) ) ;
#35559 = CARTESIAN_POINT ( 'NONE',  ( 28.13346597918727099, -5.196152422706632912, 165.9570289790974869 ) ) ;
#35560 = CARTESIAN_POINT ( 'NONE',  ( -10.69584247140429412, 136.1523137178985792, -6.932735513424201024 ) ) ;
#35561 = CARTESIAN_POINT ( 'NONE',  ( -61.48288769728821990, 203.5309553116391612, -1.857196546604028775 ) ) ;
#35562 = CARTESIAN_POINT ( 'NONE',  ( -30.20461230271183339, 207.6069050685336492, -8.469044688360751749 ) ) ;
#35563 = LINE ( 'NONE', #13017, #6426 ) ;
#35564 = CARTESIAN_POINT ( 'NONE',  ( -27.24356964375000345, 198.0031250006145456, 0.000000000000000000 ) ) ;
#35565 = CARTESIAN_POINT ( 'NONE',  ( -6.092822981423666739, 109.4148137178985536, -14.25334919248795096 ) ) ;
#35566 = CARTESIAN_POINT ( 'NONE',  ( -63.85044563604516554, 205.1570982666397072, -4.673758765035155527 ) ) ;
#35567 = EDGE_CURVE ( 'NONE', #10985, #30542, #21896, .T. ) ;
#35568 = ORIENTED_EDGE ( 'NONE', *, *, #12401, .F. ) ;
#35569 = CARTESIAN_POINT ( 'NONE',  ( 11.48171059495397728, 27.08518628210144996, 4.944772684328674117 ) ) ;
#35570 = CARTESIAN_POINT ( 'NONE',  ( 20.99999999999999645, 243.8687500012290172, 5.999999999999998224 ) ) ;
#35571 = DIRECTION ( 'NONE',  ( 0.08715574274765150453, 0.000000000000000000, 0.9961946980917461003 ) ) ;
#35572 = CARTESIAN_POINT ( 'NONE',  ( 28.10284103007056089, -5.407089921784865361, 167.0043083327929878 ) ) ;
#35573 = CARTESIAN_POINT ( 'NONE',  ( -0.1745138560725817967, 102.4101862821014493, 15.50000000000000533 ) ) ;
#35574 = CARTESIAN_POINT ( 'NONE',  ( -69.00372103062156270, 216.5309553116392181, -1.626142955000564383 ) ) ;
#35575 = CARTESIAN_POINT ( 'NONE',  ( 22.80587116629410360, -3.604726614523235284, -4.003124999385554439 ) ) ;
#35576 = CARTESIAN_POINT ( 'NONE',  ( -8.710071997420127943, 50.08518628210143930, -3.796722387233380402 ) ) ;
#35577 = DIRECTION ( 'NONE',  ( -0.000000000000000000, 1.000000000000000000, -0.000000000000000000 ) ) ;
#35578 = CARTESIAN_POINT ( 'NONE',  ( -33.57663769728823411, 202.5810206699313767, 4.149950860017909804 ) ) ;
#35579 = CARTESIAN_POINT ( 'NONE',  ( 4.622313124798573369, 83.43518628210145494, 11.61527771782819940 ) ) ;
#35580 = CARTESIAN_POINT ( 'NONE',  ( -5.732297079746171420, 222.9518338469886203, 2.500000000000000000 ) ) ;
#35581 = CYLINDRICAL_SURFACE ( 'NONE', #3863, 27.00000000000000355 ) ;
#35582 = DIRECTION ( 'NONE',  ( 0.000000000000000000, 0.000000000000000000, 1.000000000000000000 ) ) ;
#35583 = CARTESIAN_POINT ( 'NONE',  ( 36.90145218710753738, 7.646167579472015790E-16, 160.1175024667497837 ) ) ;
#35584 = CARTESIAN_POINT ( 'NONE',  ( 23.99999999999999645, 5.196152422706631135, -0.1500000000000112355 ) ) ;
#35585 = CIRCLE ( 'NONE', #4714, 2.649999999999987477 ) ;
#35586 = DIRECTION ( 'NONE',  ( 0.000000000000000000, 0.000000000000000000, 1.000000000000000000 ) ) ;
#35587 = CARTESIAN_POINT ( 'NONE',  ( 31.15718473220409379, 7.209453229046482114, 166.0971527379105908 ) ) ;
#35588 = CARTESIAN_POINT ( 'NONE',  ( 36.98155800919654723, -3.464101615137755275, 163.8277644507203945 ) ) ;
#35589 = CARTESIAN_POINT ( 'NONE',  ( 18.00000000000000000, 245.4250000000000114, -5.196152422706630247 ) ) ;
#35590 = CARTESIAN_POINT ( 'NONE',  ( 13.62178482187501416, 195.9031250006145513, 23.59362340125806767 ) ) ;
#35591 = CARTESIAN_POINT ( 'NONE',  ( -7.228626920338836470, 99.92731371789855643, -10.49813415416005213 ) ) ;
#35592 = CARTESIAN_POINT ( 'NONE',  ( -7.228626920339070061, 112.4726862821014350, 10.49813415415989404 ) ) ;
#35593 = VERTEX_POINT ( 'NONE', #16211 ) ;
#35594 = AXIS2_PLACEMENT_3D ( 'NONE', #1926, #10834, #28269 ) ;
#35595 = ORIENTED_EDGE ( 'NONE', *, *, #19147, .T. ) ;
#35596 = CARTESIAN_POINT ( 'NONE',  ( -27.24356964375000345, 194.8531250006145115, 0.000000000000000000 ) ) ;
#35597 = CARTESIAN_POINT ( 'NONE',  ( 21.00000000000000000, 239.9593750006145001, 6.646953231504538984 ) ) ;
#35598 = CARTESIAN_POINT ( 'NONE',  ( -3.257655550456946880, 82.10231371789853938, -15.46528703574811736 ) ) ;
#35599 = CARTESIAN_POINT ( 'NONE',  ( 15.24356964375000167, -3.323476615752272600, -7.415624999385471483 ) ) ;
#35600 = CARTESIAN_POINT ( 'NONE',  ( 26.75643035624999655, 247.8718750006145228, -3.323476615752271712 ) ) ;
#35601 = CARTESIAN_POINT ( 'NONE',  ( 9.534712964251941258, 99.82268628210142936, -1.715153634034235708 ) ) ;
#35602 = CYLINDRICAL_SURFACE ( 'NONE', #34901, 27.00000000000000000 ) ;
#35603 = CARTESIAN_POINT ( 'NONE',  ( -8.843639120294245259, 62.26481371789854791, -3.474262827703533230 ) ) ;
#35604 = CARTESIAN_POINT ( 'NONE',  ( 16.56230152254411436, -7.209453229046475009, -4.528124999385512162 ) ) ;
#35605 = CLOSED_SHELL ( 'NONE', ( #33228, #1215, #24657, #13716 ) ) ;
#35606 = AXIS2_PLACEMENT_3D ( 'NONE', #1023, #4431, #9380 ) ;
#35607 = CARTESIAN_POINT ( 'NONE',  ( 3.474262827703532341, 110.5648137178985593, -8.843639120294245259 ) ) ;
#35608 = CARTESIAN_POINT ( 'NONE',  ( 26.75643035624999655, 240.5593750006145228, -3.323476615752271268 ) ) ;
#35609 = CARTESIAN_POINT ( 'NONE',  ( 0.1745138560722779009, 31.78981371789854649, 12.50000000000000355 ) ) ;
#35610 =( BOUNDED_CURVE ( )  B_SPLINE_CURVE ( 2, ( #25182, #22348, #36735, #33710, #10774, #13437, #8315 ),
 .UNSPECIFIED., .F., .F. ) 
 B_SPLINE_CURVE_WITH_KNOTS ( ( 3, 2, 2, 3 ),
 ( 0.4347826086956516067, 0.4420289855072456753, 0.4492753623188397438, 0.4565217391304337569 ),
 .UNSPECIFIED. ) 
 CURVE ( )  GEOMETRIC_REPRESENTATION_ITEM ( )  RATIONAL_B_SPLINE_CURVE ( ( 1.000000000000010214, 0.8660254037844284936, 1.000000000000000000, 0.8660254037844387076, 1.000000000000000000, 0.8660254037844571373, 0.9999999999999815703 ) ) 
 REPRESENTATION_ITEM ( '' )  );
#35611 = CARTESIAN_POINT ( 'NONE',  ( 2.660918448318279950, 79.69768628210144357, -12.46528703574805697 ) ) ;
#35612 = CARTESIAN_POINT ( 'NONE',  ( 16.56230152254411081, 6.928203230275506996, -5.399999998770982579 ) ) ;
#35613 = CYLINDRICAL_SURFACE ( 'NONE', #12895, 7.500000000000000000 ) ;
#35614 = CARTESIAN_POINT ( 'NONE',  ( 24.79193261022362549, 3.604726614523236616, 164.9789157851677146 ) ) ;
#35615 = CARTESIAN_POINT ( 'NONE',  ( 15.53471296425195369, 81.42268628210145209, -2.908627838312120684 ) ) ;
#35616 = CARTESIAN_POINT ( 'NONE',  ( 10.31873187879411091, 3.604726614523240613, -5.184374999385507721 ) ) ;
#35617 = DIRECTION ( 'NONE',  ( 1.000000000000000000, 0.000000000000000000, 0.000000000000000000 ) ) ;
#35618 = CARTESIAN_POINT ( 'NONE',  ( 21.00000000000000355, 0.000000000000000000, 50.00000000000001421 ) ) ;
#35619 = CARTESIAN_POINT ( 'NONE',  ( -5.233372021372430183, 106.1476862821014322, -8.152565276336710909 ) ) ;
#35620 = CARTESIAN_POINT ( 'NONE',  ( 24.00000000000000000, -5.196152422706629359, -4.293749998770940657 ) ) ;
#35621 = CARTESIAN_POINT ( 'NONE',  ( 11.48171059495397728, 128.2851862821014493, 4.944772684328674117 ) ) ;
#35622 = CARTESIAN_POINT ( 'NONE',  ( -1.926257025242585782E-15, 196.5968750006145456, -31.45816453501075927 ) ) ;
#35623 = CARTESIAN_POINT ( 'NONE',  ( 23.87821517812500005, 240.8968750006145285, 4.985214923628404016 ) ) ;
#35624 = ORIENTED_EDGE ( 'NONE', *, *, #5546, .T. ) ;
#35625 = CARTESIAN_POINT ( 'NONE',  ( 37.44726502606470575, -3.604726614523235284, 166.3561717635493551 ) ) ;
#35626 = CARTESIAN_POINT ( 'NONE',  ( 15.24356964374999990, 0.000000000000000000, -2.390624999385471128 ) ) ;
#35627 = CARTESIAN_POINT ( 'NONE',  ( -27.24356964375000345, 199.8218750006145399, -15.72908226750537786 ) ) ;
#35628 = DIRECTION ( 'NONE',  ( 2.168404344971009484E-17, 0.000000000000000000, 1.000000000000000000 ) ) ;
#35629 = DIRECTION ( 'NONE',  ( -0.000000000000000000, -1.000000000000000000, -0.000000000000000000 ) ) ;
#35630 = LINE ( 'NONE', #24275, #25910 ) ;
#35631 = CARTESIAN_POINT ( 'NONE',  ( 1.069080835302379631E-14, 198.7624999999999886, 27.00000000000000000 ) ) ;
#35632 = CARTESIAN_POINT ( 'NONE',  ( 1.715153634034445762, 18.27731371789853299, -9.534712964251895073 ) ) ;
#35633 = CARTESIAN_POINT ( 'NONE',  ( 5.778771075727756162E-15, 196.3718750006145513, 31.45816453501076637 ) ) ;
#35635 = VERTEX_POINT ( 'NONE', #36465 ) ;
#35634 = ORIENTED_EDGE ( 'NONE', *, *, #5307, .F. ) ;
#35636 = CARTESIAN_POINT ( 'NONE',  ( 23.87821517812500005, 246.7468750006145228, 4.985214923628404016 ) ) ;
#35637 = CARTESIAN_POINT ( 'NONE',  ( 2.660918448318003282, 22.30231371789854933, 12.46528703574811558 ) ) ;
#35638 = EDGE_CURVE ( 'NONE', #9537, #21289, #25347, .T. ) ;
#35639 = CARTESIAN_POINT ( 'NONE',  ( 23.87821517812500005, -4.985214923628404016, -1.790624999385481697 ) ) ;
#35640 = CARTESIAN_POINT ( 'NONE',  ( 10.83675517735179206, 138.7398137178985564, -11.08355503943118769 ) ) ;
#35641 = ADVANCED_FACE ( 'NONE', ( #36657 ), #28977, .F. ) ;
#35642 = CARTESIAN_POINT ( 'NONE',  ( 26.99999999999999645, -3.464101615137751278, -8.306249998770956822 ) ) ;
#35643 = CARTESIAN_POINT ( 'NONE',  ( 20.99999999999999289, 244.0937500012290116, -5.999999999999997335 ) ) ;
#35644 = ORIENTED_EDGE ( 'NONE', *, *, #11558, .F. ) ;
#35645 = CARTESIAN_POINT ( 'NONE',  ( 22.80587116629411781, -3.604726614523238837, -4.959374999385526728 ) ) ;
#35646 = ORIENTED_EDGE ( 'NONE', *, *, #24836, .F. ) ;
#35647 = CARTESIAN_POINT ( 'NONE',  ( 5.778771075727756162E-15, 196.3156250006145171, 31.45816453501075927 ) ) ;
#35648 = CARTESIAN_POINT ( 'NONE',  ( 2.660918448318279950, 134.8976862821014890, -12.46528703574805697 ) ) ;
#35649 = CARTESIAN_POINT ( 'NONE',  ( 37.13513852234969193, 3.604726614523243278, 162.7885495010082764 ) ) ;
#35650 = ADVANCED_FACE ( 'NONE', ( #9453 ), #32944, .F. ) ;
#35651 = CARTESIAN_POINT ( 'NONE',  ( -61.27752896937849414, 214.3500491399821897, 7.303452534266821949 ) ) ;
#35652 = CARTESIAN_POINT ( 'NONE',  ( 20.99999999999999645, 247.3843750006145399, -6.646953231504538984 ) ) ;
#35653 = DIRECTION ( 'NONE',  ( -0.000000000000000000, -1.000000000000000000, -0.000000000000000000 ) ) ;
#35654 = CARTESIAN_POINT ( 'NONE',  ( -44.85044563604516554, 206.6211998817775566, -3.209657149897419348 ) ) ;
#35655 = CARTESIAN_POINT ( 'NONE',  ( -89.59418277001438469, 62.43429747954478159, -3.000000000000000000 ) ) ;
#35656 = CARTESIAN_POINT ( 'NONE',  ( 25.07300988058480229, -3.604726614523240613, 168.1916436865136291 ) ) ;
#35657 = ORIENTED_EDGE ( 'NONE', *, *, #12973, .F. ) ;
#35658 = CARTESIAN_POINT ( 'NONE',  ( 23.99999999999999645, 248.1062500012290570, -5.196152422706631135 ) ) ;
#35659 = CARTESIAN_POINT ( 'NONE',  ( 13.04141134922778988, 10.22731371789853405, -8.927990412390371944 ) ) ;
#35660 = CARTESIAN_POINT ( 'NONE',  ( -53.76413769728823411, 214.1499508600179240, 7.418979330068584233 ) ) ;
#35661 = CARTESIAN_POINT ( 'NONE',  ( -3.796722387233375073, 121.3851862821014578, 8.710071997420127943 ) ) ;
#35662 = PLANE ( 'NONE',  #12782 ) ;
#35663 = CARTESIAN_POINT ( 'NONE',  ( -11.61527771782819940, 21.33518628210144641, 4.622313124798574258 ) ) ;
#35664 = CARTESIAN_POINT ( 'NONE',  ( 13.56230152254410548, 5.196152422706636465, -7.275000000000058975 ) ) ;
#35665 = ORIENTED_EDGE ( 'NONE', *, *, #6147, .T. ) ;
#35666 = CARTESIAN_POINT ( 'NONE',  ( 14.25334919248782661, 128.2851862821014493, 6.092822981423971385 ) ) ;
#35667 =( BOUNDED_CURVE ( )  B_SPLINE_CURVE ( 2, ( #2608, #37288, #14182, #11336, #20063, #32165, #35753 ),
 .UNSPECIFIED., .F., .F. ) 
 B_SPLINE_CURVE_WITH_KNOTS ( ( 3, 2, 2, 3 ),
 ( 0.1304347826086954820, 0.1376811594202895783, 0.1449275362318836746, 0.1521739130434777709 ),
 .UNSPECIFIED. ) 
 CURVE ( )  GEOMETRIC_REPRESENTATION_ITEM ( )  RATIONAL_B_SPLINE_CURVE ( ( 1.000000000000002887, 0.8660254037844354880, 1.000000000000000000, 0.8660254037844387076, 1.000000000000000000, 0.8660254037844479225, 0.9999999999999907851 ) ) 
 REPRESENTATION_ITEM ( '' )  );
#35668 = CARTESIAN_POINT ( 'NONE',  ( 0.3500000000000065281, 244.5000000000000000, -2.499999999999999556 ) ) ;
#35669 = CARTESIAN_POINT ( 'NONE',  ( 9.465287035748106703, 139.6023137178985394, -2.064181346179063237 ) ) ;
#35670 = CARTESIAN_POINT ( 'NONE',  ( 5.778771075727756162E-15, 199.4656250006145797, 31.45816453501075927 ) ) ;
#35671 = CARTESIAN_POINT ( 'NONE',  ( 16.56230152254410726, 0.000000000000000000, -10.00000000000000000 ) ) ;
#35672 = CARTESIAN_POINT ( 'NONE',  ( 13.50000000000001421, 196.5500000000000114, 23.38268590217984055 ) ) ;
#35673 = CARTESIAN_POINT ( 'NONE',  ( 18.65685424949248628, -4.000000000000095923, 50.10230395283967653 ) ) ;
#35674 = CARTESIAN_POINT ( 'NONE',  ( 15.94236039944520833, 2.966254577781769264, -8.000000000000001776 ) ) ;
#35675 = CARTESIAN_POINT ( 'NONE',  ( 0.000000000000000000, 143.0000000000000000, 4.899999999999999467 ) ) ;
#35676 = CARTESIAN_POINT ( 'NONE',  ( -9.500000000000005329, 70.88981371789854791, 0.1745138560723101806 ) ) ;
#35677 = CARTESIAN_POINT ( 'NONE',  ( 20.99999999999997513, 246.3437500012290684, -5.999999999999999112 ) ) ;
#35678 = ORIENTED_EDGE ( 'NONE', *, *, #31917, .F. ) ;
#35679 = CARTESIAN_POINT ( 'NONE',  ( 23.99999999999999645, 244.9562500012290513, -5.196152422706631135 ) ) ;
#35680 = CARTESIAN_POINT ( 'NONE',  ( -4.622313124798826500, 78.36481371789855643, 11.61527771782809637 ) ) ;
#35681 = CARTESIAN_POINT ( 'NONE',  ( 13.44051670066911086, 5.407089921784862696, -3.421874999385537741 ) ) ;
#35682 = CARTESIAN_POINT ( 'NONE',  ( 19.39230484541326049, 242.7075961894323655, -5.999999999999997335 ) ) ;
#35683 = CARTESIAN_POINT ( 'NONE',  ( 15.24356964374999990, 0.000000000000000000, -3.853124999385476812 ) ) ;
#35684 = CARTESIAN_POINT ( 'NONE',  ( 2.311890736173452865, 55.07731371789855501, -12.53471296425189152 ) ) ;
#35685 = ORIENTED_EDGE ( 'NONE', *, *, #13669, .T. ) ;
#35686 = CARTESIAN_POINT ( 'NONE',  ( 26.75643035624999655, 3.323476615752271268, -7.528124999385462424 ) ) ;
#35687 = CARTESIAN_POINT ( 'NONE',  ( 21.00000000000000000, 244.4593750006145001, 6.646953231504538984 ) ) ;
#35688 = CARTESIAN_POINT ( 'NONE',  ( 8.962234695871762469, 25.36018628210144499, -8.715434833791931624 ) ) ;
#35689 = CARTESIAN_POINT ( 'NONE',  ( -36.14211230271182984, 203.5309553116391896, 1.857196546604092724 ) ) ;
#35690 = VECTOR ( 'NONE', #26153, 1000.000000000000000 ) ;
#35691 = CARTESIAN_POINT ( 'NONE',  ( -34.55877896937850124, 211.0902445701383101, -4.530955311639234040 ) ) ;
#35692 = CARTESIAN_POINT ( 'NONE',  ( 33.58116303054575269, 5.196152422706631135, 159.3822117317042455 ) ) ;
#35693 = CARTESIAN_POINT ( 'NONE',  ( 12.50000000000000355, 84.68981371789854506, -0.1745138560722771515 ) ) ;
#35694 = CARTESIAN_POINT ( 'NONE',  ( -44.26413769728823411, 212.1499508600178387, 3.954877714930865817 ) ) ;
#35695 = CARTESIAN_POINT ( 'NONE',  ( -32.58705436395489841, 203.8621396198270475, -6.307003348497942419 ) ) ;
#35696 = CARTESIAN_POINT ( 'NONE',  ( 15.24356964375000167, -3.323476615752272600, -7.415624999385472371 ) ) ;
#35697 = CARTESIAN_POINT ( 'NONE',  ( -49.64999999999999858, 244.5000000000000000, -2.499999999999998224 ) ) ;
#35698 = CARTESIAN_POINT ( 'NONE',  ( -15.50000000000000533, 52.48981371789855643, 0.1745138560722471477 ) ) ;
#35699 = CARTESIAN_POINT ( 'NONE',  ( -39.90252896937850124, 205.6499508600178103, -7.303452534266820173 ) ) ;
#35700 = CIRCLE ( 'NONE', #4240, 1.499999999999990452 ) ;
#35701 = DIRECTION ( 'NONE',  ( 0.08715574274765150453, 0.000000000000000000, 0.9961946980917461003 ) ) ;
#35702 = CARTESIAN_POINT ( 'NONE',  ( 11.61527771782819940, 90.33518628210144641, -4.622313124798573369 ) ) ;
#35703 = CARTESIAN_POINT ( 'NONE',  ( 13.04141134922759804, 36.57268628210144357, 8.927990412390657937 ) ) ;
#35704 = CARTESIAN_POINT ( 'NONE',  ( 22.56230152254411436, 3.464101615137759271, -0.1875000000000489608 ) ) ;
#35705 = CARTESIAN_POINT ( 'NONE',  ( 27.46224632087531958, 5.407089921784862696, 159.6822773018186297 ) ) ;
#35706 = ORIENTED_EDGE ( 'NONE', *, *, #14263, .F. ) ;
#35707 = CARTESIAN_POINT ( 'NONE',  ( -11.08355503943142573, 48.36018628210145209, 10.83675517735155402 ) ) ;
#35708 = CARTESIAN_POINT ( 'NONE',  ( -13.62178482187498396, 198.0781250006145342, 23.59362340125808188 ) ) ;
#35709 = CARTESIAN_POINT ( 'NONE',  ( 13.56230152254410548, 5.196152422706630247, -8.512499998770989507 ) ) ;
#35710 =( BOUNDED_CURVE ( )  B_SPLINE_CURVE ( 2, ( #35726, #18127, #17937, #15085, #6177, #26448, #29290 ),
 .UNSPECIFIED., .F., .F. ) 
 B_SPLINE_CURVE_WITH_KNOTS ( ( 3, 2, 2, 3 ),
 ( 0.8695652173913057670, 0.8768115942028998910, 0.8840579710144940151, 0.8913043478260880281 ),
 .UNSPECIFIED. ) 
 CURVE ( )  GEOMETRIC_REPRESENTATION_ITEM ( )  RATIONAL_B_SPLINE_CURVE ( ( 0.9999999999999733546, 0.8660254037844653530, 1.000000000000000000, 0.8660254037844387076, 1.000000000000000000, 0.8660254037844181685, 1.000000000000020428 ) ) 
 REPRESENTATION_ITEM ( '' )  );
#35711 = DIRECTION ( 'NONE',  ( 0.000000000000000000, 0.000000000000000000, 1.000000000000000000 ) ) ;
#35712 = CARTESIAN_POINT ( 'NONE',  ( 15.00000000000000000, 0.000000000000000000, -4.950000000000009948 ) ) ;
#35713 = CYLINDRICAL_SURFACE ( 'NONE', #6841, 5.999999999999999112 ) ;
#35714 = CARTESIAN_POINT ( 'NONE',  ( 10.69584247140445221, 25.64768628210143930, -6.932735513423970097 ) ) ;
#35715 = CARTESIAN_POINT ( 'NONE',  ( 19.39230484541326049, 247.2638461906613827, -5.999999999999994671 ) ) ;
#35716 = CARTESIAN_POINT ( 'NONE',  ( 2.064181346179061460, 123.5023137178985451, 9.465287035748106703 ) ) ;
#35717 = CARTESIAN_POINT ( 'NONE',  ( 26.75643035624999655, 246.0343750006145456, -7.049594010296217766E-16 ) ) ;
#35718 = VECTOR ( 'NONE', #16342, 1000.000000000000000 ) ;
#35719 = ORIENTED_EDGE ( 'NONE', *, *, #33134, .F. ) ;
#35720 = CARTESIAN_POINT ( 'NONE',  ( 21.00000000000000000, -6.928203230275506996, -7.537500000000000533 ) ) ;
#35721 = CARTESIAN_POINT ( 'NONE',  ( 18.00000000000000000, 5.196152422706630247, -3.225000000000005862 ) ) ;
#35722 = CARTESIAN_POINT ( 'NONE',  ( 8.715434833792128799, 138.7398137178985564, -8.962234695871567070 ) ) ;
#35723 = CARTESIAN_POINT ( 'NONE',  ( 10.31873187879411091, 3.604726614523236616, -7.828124999385535965 ) ) ;
#35724 = CARTESIAN_POINT ( 'NONE',  ( 30.92676673731498482, 7.209453229046475009, 163.4634630048305439 ) ) ;
#35725 = CARTESIAN_POINT ( 'NONE',  ( 10.56230152254411081, 0.000000000000000000, -2.587499998771031429 ) ) ;
#35726 = CARTESIAN_POINT ( 'NONE',  ( 24.66770419336863185, 0.000000000000000000, 160.7643302352881278 ) ) ;
#35727 = CARTESIAN_POINT ( 'NONE',  ( -4.944772684328673229, 56.98518628210144499, 11.48171059495397728 ) ) ;
#35728 = ORIENTED_EDGE ( 'NONE', *, *, #21488, .F. ) ;
#35729 = EDGE_LOOP ( 'NONE', ( #9265, #35546, #18593, #20825 ) ) ;
#35730 = FACE_OUTER_BOUND ( 'NONE', #27332, .T. ) ;
#35731 = CARTESIAN_POINT ( 'NONE',  ( 18.12178482187500350, -4.985214923628407568, -0.5156249993854555846 ) ) ;
#35732 = CARTESIAN_POINT ( 'NONE',  ( 33.56808966913361303, -5.196152422706629359, 159.2327825269904622 ) ) ;
#35733 = CYLINDRICAL_SURFACE ( 'NONE', #21982, 27.00000000000000355 ) ;
#35734 = CARTESIAN_POINT ( 'NONE',  ( 21.00000000000000000, 6.646953231504538984, -8.803124999385454785 ) ) ;
#35735 = AXIS2_PLACEMENT_3D ( 'NONE', #3904, #1241, #9784 ) ;
#35736 = CARTESIAN_POINT ( 'NONE',  ( -10.49813415415989581, 77.97268628210144925, -7.228626920339068285 ) ) ;
#35737 = CARTESIAN_POINT ( 'NONE',  ( -13.23911966647199812, 16.55231371789855643, -8.632099005475788900 ) ) ;
#35738 = DIRECTION ( 'NONE',  ( 0.000000000000000000, 0.000000000000000000, 1.000000000000000000 ) ) ;
#35739 = CARTESIAN_POINT ( 'NONE',  ( 17.34006124879866917, 219.7598366698699692, 4.770645753574776826 ) ) ;
#35740 = CARTESIAN_POINT ( 'NONE',  ( -32.58705436395489841, 206.7903428501026042, -3.378800118222489157 ) ) ;
#35741 = DIRECTION ( 'NONE',  ( 0.000000000000000000, 0.000000000000000000, -1.000000000000000000 ) ) ;
#35742 = CARTESIAN_POINT ( 'NONE',  ( 34.31327126962603558, -5.196152422706629359, 167.7502471956748877 ) ) ;
#35743 = CARTESIAN_POINT ( 'NONE',  ( 8.715434833792128799, 138.7398137178985564, -8.962234695871567070 ) ) ;
#35744 = CARTESIAN_POINT ( 'NONE',  ( -48.02455436395488420, 205.1570982666397356, 4.673758765035198159 ) ) ;
#35745 = CARTESIAN_POINT ( 'NONE',  ( -65.63913769728821990, 205.8500491399820760, -7.418979330068584233 ) ) ;
#35746 = CONTEXT_DEPENDENT_SHAPE_REPRESENTATION ( #2283, #31948 ) ;
#35747 = MECHANICAL_DESIGN_GEOMETRIC_PRESENTATION_REPRESENTATION (  '', ( #33920 ), #14545 ) ;
#35748 = CARTESIAN_POINT ( 'NONE',  ( 13.62178482187499640, 198.7531250006145456, -23.59362340125807123 ) ) ;
#35749 = CARTESIAN_POINT ( 'NONE',  ( -8.927990412390371944, 118.3273137178985763, -13.04141134922778988 ) ) ;
#35750 = CARTESIAN_POINT ( 'NONE',  ( -40.69419563604516554, 203.5000000000000000, 0.1155267958017914542 ) ) ;
#35751 = ORIENTED_EDGE ( 'NONE', *, *, #34811, .F. ) ;
#35752 = CARTESIAN_POINT ( 'NONE',  ( -8.962234695871760692, 20.76018628210144001, 8.715434833791933400 ) ) ;
#35753 = CARTESIAN_POINT ( 'NONE',  ( 37.26917196037089042, 7.347880794884117764E-16, 167.1152069556475510 ) ) ;
#35754 = EDGE_CURVE ( 'NONE', #36846, #36103, #914, .T. ) ;
#35755 = DIRECTION ( 'NONE',  ( 0.000000000000000000, 0.000000000000000000, -1.000000000000000000 ) ) ;
#35756 = CARTESIAN_POINT ( 'NONE',  ( 37.40967911200478824, 3.604726614523243278, 165.9265627999972992 ) ) ;
#35757 = CARTESIAN_POINT ( 'NONE',  ( -15.53471296425195369, 104.4226862821014521, 2.908627838312118019 ) ) ;
#35758 = CARTESIAN_POINT ( 'NONE',  ( -51.19122103062156270, 208.3738570449994256, -6.530955311639227823 ) ) ;
#35759 = CARTESIAN_POINT ( 'NONE',  ( 19.68408634441910365, 5.407089921784857367, -3.440624999385522020 ) ) ;
#35760 = CARTESIAN_POINT ( 'NONE',  ( 6.594114490232313663, 36.86018628210144499, 6.840914352312096547 ) ) ;
#35761 = CARTESIAN_POINT ( 'NONE',  ( 3.306546357697853733E-15, 210.0000000000000284, 27.00000000000000000 ) ) ;
#35762 = CARTESIAN_POINT ( 'NONE',  ( -33.77455436395489841, 203.6929966515020283, 6.137860380172978303 ) ) ;
#35763 = CARTESIAN_POINT ( 'NONE',  ( 19.68408634441910721, 5.407089921784862696, -9.796874999385529748 ) ) ;
#35764 = EDGE_CURVE ( 'NONE', #24506, #10376, #9641, .T. ) ;
#35765 = CARTESIAN_POINT ( 'NONE',  ( 8.962234695871762469, 71.36018628210145209, -8.715434833791931624 ) ) ;
#35766 = DIRECTION ( 'NONE',  ( 0.000000000000000000, 0.000000000000000000, 1.000000000000000000 ) ) ;
#35767 = CARTESIAN_POINT ( 'NONE',  ( 7.234628195640318005, 199.4174038105677198, -26.99999999999999645 ) ) ;
#35769 = EDGE_LOOP ( 'NONE', ( #7152, #36610, #23057, #22259 ) ) ;
#35768 = CARTESIAN_POINT ( 'NONE',  ( -8.152565276336710909, 39.44768628210144357, 5.233372021372435512 ) ) ;
#35770 = CARTESIAN_POINT ( 'NONE',  ( 27.48022219281702405, -5.407089921784859143, 159.8877424583000391 ) ) ;
#35771 = CARTESIAN_POINT ( 'NONE',  ( 21.00000000000000000, 6.646953231504538984, -9.703124999385480010 ) ) ;
#35772 = CARTESIAN_POINT ( 'NONE',  ( 25.24620043574905282, 0.000000000000000000, 167.3765725426477502 ) ) ;
#35773 = CARTESIAN_POINT ( 'NONE',  ( 33.89776776044609363, -5.407089921784861808, 161.6036962298979915 ) ) ;
#35774 = CARTESIAN_POINT ( 'NONE',  ( 36.78872592836736288, 7.347880794884125653E-16, 161.6236836811924604 ) ) ;
#35775 = CARTESIAN_POINT ( 'NONE',  ( 15.00000000000000000, 246.4000000000000057, 0.000000000000000000 ) ) ;
#35776 = CARTESIAN_POINT ( 'NONE',  ( -27.24356964374999279, 195.3406250006145228, 15.72908226750539384 ) ) ;
#35777 = EDGE_CURVE ( 'NONE', #34717, #27686, #15155, .T. ) ;
#35778 = CARTESIAN_POINT ( 'NONE',  ( 0.1745138560722779009, 96.18981371789855928, 12.50000000000000355 ) ) ;
#35779 = CARTESIAN_POINT ( 'NONE',  ( 12.50000000000000355, 109.3101862821014549, 0.1745138560725507937 ) ) ;
#35780 = ORIENTED_EDGE ( 'NONE', *, *, #33045, .F. ) ;
#35781 = AXIS2_PLACEMENT_3D ( 'NONE', #10072, #24297, #7054 ) ;
#35782 = ORIENTED_EDGE ( 'NONE', *, *, #7760, .T. ) ;
#35783 = CARTESIAN_POINT ( 'NONE',  ( 27.24356964375000700, 196.3906250006145058, 15.72908226750537075 ) ) ;
#35784 = CARTESIAN_POINT ( 'NONE',  ( 27.96351228082934171, 5.196152422706630247, 164.0144493178186167 ) ) ;
#35785 = EDGE_CURVE ( 'NONE', #31993, #30479, #17381, .T. ) ;
#35786 = CARTESIAN_POINT ( 'NONE',  ( -10.83675517735179028, 69.73981371789855643, 11.08355503943118947 ) ) ;
#35787 = CARTESIAN_POINT ( 'NONE',  ( 23.87821517812500005, -4.985214923628404016, -6.403124999385473082 ) ) ;
#35788 = CARTESIAN_POINT ( 'NONE',  ( 15.24356964375000167, 244.9468750006145399, 3.323476615752272600 ) ) ;
#35789 = CARTESIAN_POINT ( 'NONE',  ( -8.152565276336710909, 94.64768628210147483, 5.233372021372435512 ) ) ;
#35790 = DIRECTION ( 'NONE',  ( 0.000000000000000000, 0.000000000000000000, 1.000000000000000000 ) ) ;
#35791 = CARTESIAN_POINT ( 'NONE',  ( 8.152565276336593669, 57.95231371789854791, 5.233372021372610483 ) ) ;
#35792 = CARTESIAN_POINT ( 'NONE',  ( 16.56230152254411081, 7.209453229046475009, -8.353124999385524774 ) ) ;
#35793 = CARTESIAN_POINT ( 'NONE',  ( 8.152565276336593669, 113.1523137178985650, 5.233372021372610483 ) ) ;
#35794 = CARTESIAN_POINT ( 'NONE',  ( 23.87821517812500005, 240.4468750006145115, 4.985214923628404016 ) ) ;
#35795 = CARTESIAN_POINT ( 'NONE',  ( -2.660918448318004614, 36.10231371789853938, -12.46528703574811558 ) ) ;
#35796 = CARTESIAN_POINT ( 'NONE',  ( 0.000000000000000000, -20.00000000000000000, 4.899999999999999467 ) ) ;
#35797 = VECTOR ( 'NONE', #11857, 1000.000000000000000 ) ;
#35798 = CARTESIAN_POINT ( 'NONE',  ( 2.311890736173175753, 83.72268628210143504, 12.53471296425194836 ) ) ;
#35799 = CARTESIAN_POINT ( 'NONE',  ( 22.56230152254410370, 7.347880794884117764E-16, -5.062499998771007981 ) ) ;
#35800 = CARTESIAN_POINT ( 'NONE',  ( 20.99999999999999645, 185.0294372515228645, 0.000000000000000000 ) ) ;
#35801 = CARTESIAN_POINT ( 'NONE',  ( 37.17926111711567927, 3.604726614523238837, 163.2928730669172523 ) ) ;
#35802 = CARTESIAN_POINT ( 'NONE',  ( 10.31873187879410558, 0.000000000000000000, -4.246874999385502392 ) ) ;
#35803 = CARTESIAN_POINT ( 'NONE',  ( 24.00000000000000000, 248.3499999999999943, 5.196152422706629359 ) ) ;
#35804 = CARTESIAN_POINT ( 'NONE',  ( 22.56230152254451937, 3.464101615137510137, -7.274999998771029652 ) ) ;
#35805 = EDGE_CURVE ( 'NONE', #26422, #18816, #19050, .T. ) ;
#35806 = CARTESIAN_POINT ( 'NONE',  ( -9.534712964251941258, 104.4226862821014521, 1.715153634034234154 ) ) ;
#35807 = CARTESIAN_POINT ( 'NONE',  ( 15.00000000000000000, 248.2562500012290627, 0.000000000000000000 ) ) ;
#35808 = ADVANCED_FACE ( 'NONE', ( #13242 ), #33697, .F. ) ;
#35809 = CARTESIAN_POINT ( 'NONE',  ( -2.311890736173176641, 125.1226862821014549, -12.53471296425194836 ) ) ;
#35810 = CARTESIAN_POINT ( 'NONE',  ( -6.396089478038519793, 142.9999999999984652, 10.57287770549605632 ) ) ;
#35811 = CARTESIAN_POINT ( 'NONE',  ( 15.24356964374999990, 248.9218750006145058, -3.323476615752268604 ) ) ;
#35812 = EDGE_LOOP ( 'NONE', ( #30029, #3563, #30716, #22747 ) ) ;
#35813 = CARTESIAN_POINT ( 'NONE',  ( 31.27974749544297595, 7.209453229046475009, 167.4980515321021244 ) ) ;
#35814 = CARTESIAN_POINT ( 'NONE',  ( 18.12178482187500350, -4.985214923628407568, -1.865624999385473437 ) ) ;
#35816 = EDGE_CURVE ( 'NONE', #33644, #19092, #6979, .T. ) ;
#35815 = CARTESIAN_POINT ( 'NONE',  ( -27.24356964375000345, 199.3718750006145513, -15.72908226750537786 ) ) ;
#35817 = CARTESIAN_POINT ( 'NONE',  ( 19.98631459334238514, 239.9067735275330904, -5.748934852092073555 ) ) ;
#35818 = CARTESIAN_POINT ( 'NONE',  ( 20.99999999999999645, 185.0294372515228645, 0.000000000000000000 ) ) ;
#35819 = CARTESIAN_POINT ( 'NONE',  ( 31.12531841381553477, -6.928203230275506996, 165.7329190520329973 ) ) ;
#35820 = FACE_OUTER_BOUND ( 'NONE', #4349, .T. ) ;
#35821 = CARTESIAN_POINT ( 'NONE',  ( -9.465287035748106703, 15.40231371789854720, 2.064181346179061460 ) ) ;
#35822 = CARTESIAN_POINT ( 'NONE',  ( -27.24356964374999279, 196.2968750006145342, 15.72908226750539384 ) ) ;
#35824 = ORIENTED_EDGE ( 'NONE', *, *, #10189, .T. ) ;
#35823 = ORIENTED_EDGE ( 'NONE', *, *, #23982, .F. ) ;
#35825 = CARTESIAN_POINT ( 'NONE',  ( 15.24356964375000167, 247.9843750006145058, 3.323476615752272600 ) ) ;
#35826 = EDGE_CURVE ( 'NONE', #30347, #30489, #19319, .T. ) ;
#35827 = CARTESIAN_POINT ( 'NONE',  ( -12.46528703574811558, 24.60231371789854649, 2.660918448318004170 ) ) ;
#35828 = CARTESIAN_POINT ( 'NONE',  ( 26.75643035624999655, -3.323476615752267715, -0.4031249993854607028 ) ) ;
#35829 = CARTESIAN_POINT ( 'NONE',  ( -11.08355503943118592, 136.4398137178985735, -10.83675517735179383 ) ) ;
#35830 = CARTESIAN_POINT ( 'NONE',  ( 15.24356964374999990, 0.000000000000000000, -0.2531249993854844949 ) ) ;
#35831 = DIRECTION ( 'NONE',  ( 0.000000000000000000, -1.000000000000000000, 0.000000000000000000 ) ) ;
#35832 = ORIENTED_EDGE ( 'NONE', *, *, #2979, .T. ) ;
#35833 = CARTESIAN_POINT ( 'NONE',  ( 16.56230152254411436, -7.209453229046482114, -7.284374999385498484 ) ) ;
#35834 = EDGE_LOOP ( 'NONE', ( #1285, #12526 ) ) ;
#35835 = CARTESIAN_POINT ( 'NONE',  ( -13.62178482187498396, 196.7281250006145399, 23.59362340125808188 ) ) ;
#35836 = CARTESIAN_POINT ( 'NONE',  ( -0.1745138560725500443, 130.0101862821014436, 12.50000000000000355 ) ) ;
#35837 = CARTESIAN_POINT ( 'NONE',  ( 37.21031035046954116, 7.646167579472024665E-16, 163.6477674281124450 ) ) ;
#35838 = CARTESIAN_POINT ( 'NONE',  ( -50.59002896937850835, 202.6965474657332038, 4.350049139982197666 ) ) ;
#35839 = CARTESIAN_POINT ( 'NONE',  ( 26.75643035624999655, 245.8843750006145115, 3.323476615752267271 ) ) ;
#35840 = CARTESIAN_POINT ( 'NONE',  ( 22.56230152254410726, 7.347880794884117764E-16, -9.562499998771039955 ) ) ;
#35841 = CARTESIAN_POINT ( 'NONE',  ( -46.63169563604517265, 210.1155267958017703, 4.499999999999996447 ) ) ;
#35842 = CARTESIAN_POINT ( 'NONE',  ( 11.61527771782819940, 136.3351862821014606, -4.622313124798573369 ) ) ;
#35843 = CARTESIAN_POINT ( 'NONE',  ( 37.37209319794485651, 7.646167579472015790E-16, 165.4969538364452148 ) ) ;
#35844 = ORIENTED_EDGE ( 'NONE', *, *, #11897, .F. ) ;
#35845 = CARTESIAN_POINT ( 'NONE',  ( 26.99999999999999645, 241.7687500012290513, -3.464101615137755275 ) ) ;
#35846 = CARTESIAN_POINT ( 'NONE',  ( -14.25334919248782306, 132.8851862821014436, -6.092822981423979378 ) ) ;
#35847 = CARTESIAN_POINT ( 'NONE',  ( -46.83705436395489130, 203.8621396198270475, -6.307003348497942419 ) ) ;
#35848 = CARTESIAN_POINT ( 'NONE',  ( 8.710071997420127943, 109.8851862821014720, 3.796722387233375073 ) ) ;
#35849 = ADVANCED_FACE ( 'NONE', ( #7926 ), #25165, .T. ) ;
#35850 = CARTESIAN_POINT ( 'NONE',  ( 19.39230484541324273, 241.5424038105676914, 5.999999999999987566 ) ) ;
#35851 = CARTESIAN_POINT ( 'NONE',  ( 12.53471296425194836, 26.22268628210144925, -2.311890736173178418 ) ) ;
#35852 = CARTESIAN_POINT ( 'NONE',  ( 22.56230152254411792, 3.464101615137759271, -7.837500000000039435 ) ) ;
#35853 = UNCERTAINTY_MEASURE_WITH_UNIT (LENGTH_MEASURE( 1.000000000000000082E-05 ), #9698, 'distance_accuracy_value', 'NONE');
#35854 = ORIENTED_EDGE ( 'NONE', *, *, #19704, .T. ) ;
#35855 = CARTESIAN_POINT ( 'NONE',  ( -8.632099005475501130, 115.3476862821014493, -13.23911966647218996 ) ) ;
#35856 = CARTESIAN_POINT ( 'NONE',  ( 10.56230152254305565, -3.464101615137144652, -6.149999998771001231 ) ) ;
#35857 = CARTESIAN_POINT ( 'NONE',  ( -8.152565276336593669, 136.1523137178985507, -5.233372021372610483 ) ) ;
#35858 = CARTESIAN_POINT ( 'NONE',  ( 27.24356964375000345, 199.5781250006145342, -3.336375036156643733E-15 ) ) ;
#35859 = CARTESIAN_POINT ( 'NONE',  ( 20.99999999999997868, 245.1625000000000227, 5.999999999999999112 ) ) ;
#35860 = CARTESIAN_POINT ( 'NONE',  ( -1.909035429704832693E-15, 196.2875000000000227, -31.17691453623979214 ) ) ;
#35861 = FACE_OUTER_BOUND ( 'NONE', #8338, .T. ) ;
#35862 = CARTESIAN_POINT ( 'NONE',  ( 10.49999999999999645, 244.5000000000000000, -2.500000000000000000 ) ) ;
#35863 = DIRECTION ( 'NONE',  ( 0.000000000000000000, 0.000000000000000000, 1.000000000000000000 ) ) ;
#35864 = CARTESIAN_POINT ( 'NONE',  ( -3.796722387233185003, 81.81481371789855928, -8.710071997420207879 ) ) ;
#35865 = ORIENTED_EDGE ( 'NONE', *, *, #34859, .F. ) ;
#35866 = CARTESIAN_POINT ( 'NONE',  ( 15.00000000000000000, 243.7187500012290684, -3.464101615137752166 ) ) ;
#35867 = CARTESIAN_POINT ( 'NONE',  ( -12.50000000000000355, 89.28981371789855359, 0.1745138560722786503 ) ) ;
#35868 = CARTESIAN_POINT ( 'NONE',  ( 13.44051670066911441, -5.407089921784865361, -4.621874999385545024 ) ) ;
#35869 = CARTESIAN_POINT ( 'NONE',  ( -6.474010430066216237, 143.0000000000000284, 10.78258735713080796 ) ) ;
#35870 = CARTESIAN_POINT ( 'NONE',  ( 18.12178482187500350, -4.985214923628407568, -3.778124999385484628 ) ) ;
#35871 = CARTESIAN_POINT ( 'NONE',  ( 12.50000000000000355, 47.88981371789854791, -0.1745138560722771515 ) ) ;
#35872 = ORIENTED_EDGE ( 'NONE', *, *, #10512, .F. ) ;
#35873 = FACE_OUTER_BOUND ( 'NONE', #27636, .T. ) ;
#35874 = CARTESIAN_POINT ( 'NONE',  ( 26.75643035624999655, 244.5343750006144887, 3.323476615752267715 ) ) ;
#35875 = CARTESIAN_POINT ( 'NONE',  ( 2.311890736173175753, 19.32268628210144712, 12.53471296425194836 ) ) ;
#35876 = VECTOR ( 'NONE', #32962, 1000.000000000000000 ) ;
#35877 = CARTESIAN_POINT ( 'NONE',  ( -39.50669563604517265, 209.8844732041982013, -6.500000000000000888 ) ) ;
#35878 = CARTESIAN_POINT ( 'NONE',  ( -56.32961230271183695, 211.8571965466040297, 6.469044688360755302 ) ) ;
#35879 = CARTESIAN_POINT ( 'NONE',  ( 30.63506736085999549, 6.928203230275506996, 160.1293238752668913 ) ) ;
#35880 = CARTESIAN_POINT ( 'NONE',  ( -12.53471296425189152, 80.37731371789854506, -2.311890736173453753 ) ) ;
#35881 = CARTESIAN_POINT ( 'NONE',  ( -52.18080436395490551, 205.4999999999999716, -0.1155267958017894420 ) ) ;
#35882 = EDGE_CURVE ( 'NONE', #33723, #29149, #21265, .T. ) ;
#35883 = CARTESIAN_POINT ( 'NONE',  ( -56.53497103062156270, 204.4285982733020148, -3.350049139982115509 ) ) ;
#35884 = CARTESIAN_POINT ( 'NONE',  ( 26.75643035624999655, 7.049594010296217766E-16, -5.878124999385475391 ) ) ;
#35885 = CARTESIAN_POINT ( 'NONE',  ( 2.999999999999997335, 244.5000000000000000, -11.00000000000000000 ) ) ;
#35886 = CARTESIAN_POINT ( 'NONE',  ( 6.092822981423662299, 49.61481371789856354, 14.25334919248795096 ) ) ;
#35887 = CARTESIAN_POINT ( 'NONE',  ( -50.39211230271182984, 201.5309553116392181, 2.393094931466368980 ) ) ;
#35888 = CIRCLE ( 'NONE', #19582, 6.000000000000005329 ) ;
#35889 = CARTESIAN_POINT ( 'NONE',  ( -13.50000000000000533, 198.1250000000000284, -23.38268590217984411 ) ) ;
#35890 = CARTESIAN_POINT ( 'NONE',  ( 11.61527771782819940, 81.13518628210145778, -4.622313124798573369 ) ) ;
#35891 = EDGE_CURVE ( 'NONE', #33506, #24506, #29199, .T. ) ;
#35892 = CARTESIAN_POINT ( 'NONE',  ( 14.25334919248782661, 36.28518628210144215, 6.092822981423971385 ) ) ;
#35893 = FACE_OUTER_BOUND ( 'NONE', #28754, .T. ) ;
#35894 = CARTESIAN_POINT ( 'NONE',  ( -28.29769750636678793, 205.1215485303246453, -6.345809158763446867 ) ) ;
#35895 = EDGE_LOOP ( 'NONE', ( #30528, #5011, #1466, #9715 ) ) ;
#35896 = CARTESIAN_POINT ( 'NONE',  ( -10.83675517735155047, 41.46018628210145351, -11.08355503943142750 ) ) ;
#35897 = CARTESIAN_POINT ( 'NONE',  ( 27.24356964375000700, 197.7406250006145285, 15.72908226750537075 ) ) ;
#35898 = CARTESIAN_POINT ( 'NONE',  ( -27.24356964375000345, 199.8593750006145342, 0.000000000000000000 ) ) ;
#35899 = DIRECTION ( 'NONE',  ( -0.000000000000000000, -1.000000000000000000, -0.000000000000000000 ) ) ;
#35900 = CARTESIAN_POINT ( 'NONE',  ( -43.67038769728823411, 208.1428034533959703, 6.469044688360770401 ) ) ;
#35901 = DIRECTION ( 'NONE',  ( 0.000000000000000000, 0.000000000000000000, 1.000000000000000000 ) ) ;
#35902 = CARTESIAN_POINT ( 'NONE',  ( -10.69584247140444866, 30.24768628210144783, 6.932735513423972762 ) ) ;
#35903 = CARTESIAN_POINT ( 'NONE',  ( 26.75643035624999655, 249.2218750006144887, -3.323476615752271712 ) ) ;
#35904 = CARTESIAN_POINT ( 'NONE',  ( -7.954856959092309943, 134.4273137178984996, 5.529263428287300108 ) ) ;
#35905 = CARTESIAN_POINT ( 'NONE',  ( 20.99999999999999645, 244.3468750006145171, -6.646953231504538984 ) ) ;
#35906 = EDGE_LOOP ( 'NONE', ( #12856, #19866, #2564, #36848, #11622, #10540, #29763, #7436 ) ) ;
#35907 = ADVANCED_BREP_SHAPE_REPRESENTATION ( '', ( #20157, #17215 ), #5638 ) ;
#35908 = CARTESIAN_POINT ( 'NONE',  ( 26.99999999999952038, 3.464101615138031054, -3.337499999999980815 ) ) ;
#35909 = CARTESIAN_POINT ( 'NONE',  ( 6.932735513424201024, 129.2523137178985451, -10.69584247140429412 ) ) ;
#35910 = CARTESIAN_POINT ( 'NONE',  ( 13.44051670066911619, -5.407089921784859143, -7.715624999385550353 ) ) ;
#35911 = CARTESIAN_POINT ( 'NONE',  ( 24.75924920669326212, -3.604726614523240613, 164.6053427733833132 ) ) ;
#35912 = CARTESIAN_POINT ( 'NONE',  ( 22.56230152254410370, 0.000000000000000000, -10.00000000000000000 ) ) ;
#35913 = CARTESIAN_POINT ( 'NONE',  ( -27.00000000000000355, 197.7500000000000000, 0.000000000000000000 ) ) ;
#35914 = ORIENTED_EDGE ( 'NONE', *, *, #27085, .T. ) ;
#35915 = CARTESIAN_POINT ( 'NONE',  ( -11.61527771782819940, 48.93518628210144783, 4.622313124798574258 ) ) ;
#35916 = ORIENTED_EDGE ( 'NONE', *, *, #20101, .T. ) ;
#35917 = VERTEX_POINT ( 'NONE', #13617 ) ;
#35918 = CARTESIAN_POINT ( 'NONE',  ( 28.48305061405702787, 5.725134515572933402, 159.4403097883559894 ) ) ;
#35919 = CARTESIAN_POINT ( 'NONE',  ( 26.75643035624999655, 7.049594010296217766E-16, -1.265624999385456251 ) ) ;
#35920 = CARTESIAN_POINT ( 'NONE',  ( 10.56230152254410548, 0.000000000000000000, -9.450000000000041922 ) ) ;
#35922 = CARTESIAN_POINT ( 'NONE',  ( 20.99999999999999645, 6.928203230275506996, -4.612499999999980282 ) ) ;
#35921 = PRESENTATION_LAYER_ASSIGNMENT (  '', '', ( #14744 ) ) ;
#35923 = CARTESIAN_POINT ( 'NONE',  ( 23.87821517812499650, 4.985214923628404904, -7.940624999385470062 ) ) ;
#35924 = CARTESIAN_POINT ( 'NONE',  ( 12.53471296425194836, 81.42268628210145209, -2.311890736173178418 ) ) ;
#35925 = CARTESIAN_POINT ( 'NONE',  ( -13.23911966647218463, 140.6476862821014322, 8.632099005475506459 ) ) ;
#35926 = DIRECTION ( 'NONE',  ( 0.9961946980917459893, 0.000000000000000000, -0.08715574274765348906 ) ) ;
#35927 = CARTESIAN_POINT ( 'NONE',  ( 16.85147890419444394, 211.5556954109258641, 5.808099892140972109 ) ) ;
#35928 = CARTESIAN_POINT ( 'NONE',  ( -58.30877896937849414, 211.0902445701383101, -4.530955311639234040 ) ) ;
#35929 = DIRECTION ( 'NONE',  ( 1.000000000000000000, 0.000000000000000000, 0.000000000000000000 ) ) ;
#35930 = CARTESIAN_POINT ( 'NONE',  ( 34.28712454680172783, 5.196152422706631135, 167.4513887862474064 ) ) ;
#35931 = CARTESIAN_POINT ( 'NONE',  ( 11.48171059495408208, 139.3148137178985451, -4.944772684328420986 ) ) ;
#35932 = CARTESIAN_POINT ( 'NONE',  ( -43.47247103062156981, 206.6499508600178672, 5.571401726697986057 ) ) ;
#35933 = CARTESIAN_POINT ( 'NONE',  ( -31.59002896937850124, 202.6965474657332038, 4.350049139982197666 ) ) ;
#35935 = APPLICATION_CONTEXT ( 'automotive_design' ) ;
#35934 = SHAPE_DEFINITION_REPRESENTATION ( #14397, #2638 ) ;
#35936 = CARTESIAN_POINT ( 'NONE',  ( 16.56230152254410726, 0.000000000000000000, 0.000000000000000000 ) ) ;
#35937 = CARTESIAN_POINT ( 'NONE',  ( -27.24356964374999990, 197.5156250006145626, -15.72908226750537786 ) ) ;
#35938 = CARTESIAN_POINT ( 'NONE',  ( -8.632099005475794229, 106.2523137178985451, 13.23911966647199812 ) ) ;
#35939 = CARTESIAN_POINT ( 'NONE',  ( -42.47544563604516554, 214.8429017333602360, 4.673758765035156415 ) ) ;
#35940 = ORIENTED_EDGE ( 'NONE', *, *, #14499, .F. ) ;
#35941 =( BOUNDED_CURVE ( )  B_SPLINE_CURVE ( 2, ( #14753, #35019, #9063, #3740, #3561, #703, #20634 ),
 .UNSPECIFIED., .F., .F. ) 
 B_SPLINE_CURVE_WITH_KNOTS ( ( 3, 2, 2, 3 ),
 ( 0.4782608695652166841, 0.4855072463768107527, 0.4927536231884049323, 0.4999999999999990008 ),
 .UNSPECIFIED. ) 
 CURVE ( )  GEOMETRIC_REPRESENTATION_ITEM ( )  RATIONAL_B_SPLINE_CURVE ( ( 1.000000000000013545, 0.8660254037844254960, 1.000000000000000000, 0.8660254037844387076, 1.000000000000000000, 0.8660254037844571373, 0.9999999999999815703 ) ) 
 REPRESENTATION_ITEM ( '' )  );
#35942 = CARTESIAN_POINT ( 'NONE',  ( 12.46528703574805874, 26.79768628210144144, 2.660918448318279950 ) ) ;
#35943 = DIRECTION ( 'NONE',  ( -0.000000000000000000, -0.000000000000000000, 1.000000000000000000 ) ) ;
#35944 = CARTESIAN_POINT ( 'NONE',  ( 34.36840877128340566, -5.407089921784861808, 166.9831475995933943 ) ) ;
#35945=STYLED_ITEM('',(#37528),#7886);
#35946 = CARTESIAN_POINT ( 'NONE',  ( -8.632099005475501130, 106.1476862821014322, -13.23911966647218996 ) ) ;
#35947 = PRODUCT_DEFINITION_FORMATION_WITH_SPECIFIED_SOURCE ( 'ANY', '', #3512, .NOT_KNOWN. ) ;
#35948 = CARTESIAN_POINT ( 'NONE',  ( -49.21205436395489841, 214.6737587650351884, 4.842901733360205796 ) ) ;
#35949 = CARTESIAN_POINT ( 'NONE',  ( 22.80587116629410716, 7.646167579472015790E-16, -4.865624999385531169 ) ) ;
#35950 = CARTESIAN_POINT ( 'NONE',  ( 6.840914352312096547, 43.76018628210144357, -6.594114490232313663 ) ) ;
#35951 = CARTESIAN_POINT ( 'NONE',  ( 10.56230152254410903, 7.347880794884117764E-16, -10.00000000000000000 ) ) ;
#35952 = CARTESIAN_POINT ( 'NONE',  ( -40.50372103062156981, 218.5309553116391896, -2.162041339862839084 ) ) ;
#35953 = AXIS2_PLACEMENT_3D ( 'NONE', #19801, #25465, #33437 ) ;
#35954 = PLANE ( 'NONE',  #14697 ) ;
#35955 = CARTESIAN_POINT ( 'NONE',  ( 8.962234695871762469, 80.56018628210145494, -8.715434833791931624 ) ) ;
#35956 = CARTESIAN_POINT ( 'NONE',  ( 13.50000000000001421, 199.7000000000000171, 23.38268590217984055 ) ) ;
#35957 = DIRECTION ( 'NONE',  ( 0.000000000000000000, 0.000000000000000000, 1.000000000000000000 ) ) ;
#35959 = CARTESIAN_POINT ( 'NONE',  ( 15.00000000000000000, 0.000000000000000000, -5.399999999999987921 ) ) ;
#35958 = CARTESIAN_POINT ( 'NONE',  ( 8.710071997420127943, 45.48518628210144499, 3.796722387233375073 ) ) ;
#35960 = DIRECTION ( 'NONE',  ( -0.000000000000000000, -0.000000000000000000, 1.000000000000000000 ) ) ;
#35961 = ORIENTED_EDGE ( 'NONE', *, *, #25994, .T. ) ;
#35962 = CARTESIAN_POINT ( 'NONE',  ( 23.99999999999999645, 5.196152422706631135, -1.049999999999995381 ) ) ;
#35963 = CARTESIAN_POINT ( 'NONE',  ( -64.84747103062156270, 213.3500491399821328, -5.571401726697985168 ) ) ;
#35964 = CARTESIAN_POINT ( 'NONE',  ( 24.67263818733777470, 0.000000000000000000, 163.6153742921546836 ) ) ;
#35965 = CARTESIAN_POINT ( 'NONE',  ( 30.74292259240310443, 6.928203230275514990, 161.3621148129311109 ) ) ;
#35966 = CARTESIAN_POINT ( 'NONE',  ( 26.99999999999999645, 246.1375000000000171, 3.464101615137751278 ) ) ;
#35967 = CARTESIAN_POINT ( 'NONE',  ( -27.24356964375000345, 196.6531250006145513, 0.000000000000000000 ) ) ;
#35968 =( BOUNDED_CURVE ( )  B_SPLINE_CURVE ( 2, ( #18670, #18102, #24154, #831, #27177, #29829, #1201 ),
 .UNSPECIFIED., .F., .F. ) 
 B_SPLINE_CURVE_WITH_KNOTS ( ( 3, 2, 2, 3 ),
 ( 0.04347826086956579211, 0.05072463768116096394, 0.05797101449275612883, 0.06521739130435129372 ),
 .UNSPECIFIED. ) 
 CURVE ( )  GEOMETRIC_REPRESENTATION_ITEM ( )  RATIONAL_B_SPLINE_CURVE ( ( 0.9999999999999893419, 0.8660254037844493658, 1.000000000000000000, 0.8660254037844387076, 1.000000000000000000, 0.8660254037843745367, 1.000000000000064171 ) ) 
 REPRESENTATION_ITEM ( '' )  );
#35969 = CARTESIAN_POINT ( 'NONE',  ( 4.944772684328420986, 86.41481371789855359, 11.48171059495408208 ) ) ;
#35970 = CARTESIAN_POINT ( 'NONE',  ( 11.61527771782819940, 108.7351862821014663, -4.622313124798573369 ) ) ;
#35971 = ORIENTED_EDGE ( 'NONE', *, *, #25685, .F. ) ;
#35972 = ORIENTED_EDGE ( 'NONE', *, *, #31917, .T. ) ;
#35973 = CARTESIAN_POINT ( 'NONE',  ( -1.909035429704832693E-15, 198.6500000012290457, -31.17691453623979214 ) ) ;
#35974 = CARTESIAN_POINT ( 'NONE',  ( 19.56230152254411436, -5.196152422706629359, -9.187499998771025744 ) ) ;
#35975 = CARTESIAN_POINT ( 'NONE',  ( -0.1745138560722442889, 82.38981371789856212, -15.50000000000000533 ) ) ;
#35976 = EDGE_CURVE ( 'NONE', #31911, #30763, #31047, .T. ) ;
#35977 = CARTESIAN_POINT ( 'NONE',  ( 26.75643035624999655, 3.323476615752271712, -6.740624999385494753 ) ) ;
#35978 = CARTESIAN_POINT ( 'NONE',  ( 26.75643035624999655, 246.0343750006145456, -7.049594010296217766E-16 ) ) ;
#35979 = CARTESIAN_POINT ( 'NONE',  ( -52.37872103062156981, 205.4690446883607535, 1.090244570138264368 ) ) ;
#35980 = AXIS2_PLACEMENT_3D ( 'NONE', #33995, #13537, #36832 ) ;
#35981 = CARTESIAN_POINT ( 'NONE',  ( 24.00000000000000000, -5.196152422706629359, -6.543749998770942433 ) ) ;
#35982 = CARTESIAN_POINT ( 'NONE',  ( 0.1745138560723095977, 50.18981371789855217, 9.500000000000005329 ) ) ;
#35983 = CARTESIAN_POINT ( 'NONE',  ( 22.80587116629410716, 7.646167579472015790E-16, -8.465624999385523708 ) ) ;
#35984 = CARTESIAN_POINT ( 'NONE',  ( -0.1745138560723084320, 119.1898137178985593, -9.500000000000005329 ) ) ;
#35985 = CARTESIAN_POINT ( 'NONE',  ( 20.99999999999999645, 240.6343750006145115, -6.646953231504538984 ) ) ;
#35986 = CARTESIAN_POINT ( 'NONE',  ( -11.48171059495408208, 33.51481371789854791, 4.944772684328421875 ) ) ;
#35987 = CARTESIAN_POINT ( 'NONE',  ( 12.53471296425194836, 90.62268628210146915, -2.311890736173178418 ) ) ;
#35988 = CARTESIAN_POINT ( 'NONE',  ( 19.56230152254411792, -5.196152422706629359, -7.387499998771030363 ) ) ;
#35989 = EDGE_CURVE ( 'NONE', #10943, #37177, #16383, .T. ) ;
#35990 = CARTESIAN_POINT ( 'NONE',  ( 22.56230152254410370, 7.347880794884117764E-16, -6.412499998770998744 ) ) ;
#35991 = CARTESIAN_POINT ( 'NONE',  ( 24.67754069786733240, 0.000000000000000000, 163.6714102439223097 ) ) ;
#35992 = CARTESIAN_POINT ( 'NONE',  ( 10.31873187879411091, -3.604726614523244610, -4.659374999385518024 ) ) ;
#35993 = CARTESIAN_POINT ( 'NONE',  ( 10.56230152254426713, -3.464101615137852974, -1.762500000000048139 ) ) ;
#35994 = CARTESIAN_POINT ( 'NONE',  ( 19.39230484541326049, 244.0575961894323598, -5.999999999999997335 ) ) ;
#35995 = CARTESIAN_POINT ( 'NONE',  ( -9.534712964251941258, 86.02268628210144641, 1.715153634034234154 ) ) ;
#35996 = CARTESIAN_POINT ( 'NONE',  ( 26.99999999999995737, 3.464101615137778811, -2.381249998770954779 ) ) ;
#35997 = ADVANCED_FACE ( 'NONE', ( #4323 ), #33327, .T. ) ;
#35998 = CARTESIAN_POINT ( 'NONE',  ( 11.61527771782819940, 127.1351862821014578, -4.622313124798573369 ) ) ;
#35999 = CARTESIAN_POINT ( 'NONE',  ( 20.99999999999999645, 0.000000000000000000, -8.000000000000000000 ) ) ;
#36000 = CARTESIAN_POINT ( 'NONE',  ( 21.00000000000000000, 240.4093750006145171, 6.646953231504538984 ) ) ;
#36001 = VERTEX_POINT ( 'NONE', #26267 ) ;
#36002 = CARTESIAN_POINT ( 'NONE',  ( 24.87364111904954811, 0.000000000000000000, 165.9128483146287465 ) ) ;
#36003 = CARTESIAN_POINT ( 'NONE',  ( 21.00000000000000000, 6.646953231504538984, -2.503124999385450966 ) ) ;
#36004 = CARTESIAN_POINT ( 'NONE',  ( 36.83775103377001869, 7.347880794884117764E-16, 162.1840432000934129 ) ) ;
#36005 = FACE_OUTER_BOUND ( 'NONE', #9506, .T. ) ;
#36006 = CYLINDRICAL_SURFACE ( 'NONE', #28778, 5.999999999999999112 ) ;
#36007 = CARTESIAN_POINT ( 'NONE',  ( 37.43585731826866692, 0.000000000000000000, 169.0204293145237102 ) ) ;
#36008 = CARTESIAN_POINT ( 'NONE',  ( 26.75643035624999655, 242.3968750006145001, 3.323476615752267715 ) ) ;
#36009 = CARTESIAN_POINT ( 'NONE',  ( 10.31873187879411091, -3.604726614523240613, -1.903124999385531924 ) ) ;
#36010 = CARTESIAN_POINT ( 'NONE',  ( 3.796722387233182339, 12.81481371789855217, 8.710071997420207879 ) ) ;
#36011 = CARTESIAN_POINT ( 'NONE',  ( -27.24356964375000345, 198.0593750006145513, 0.000000000000000000 ) ) ;
#36013 = ORIENTED_EDGE ( 'NONE', *, *, #6679, .F. ) ;
#36012 = ORIENTED_EDGE ( 'NONE', *, *, #7408, .T. ) ;
#36014 = CARTESIAN_POINT ( 'NONE',  ( 15.24356964374999990, 247.9093750006145171, -3.323476615752268604 ) ) ;
#36015 = CARTESIAN_POINT ( 'NONE',  ( -12.46528703574811558, 33.80231371789854933, 2.660918448318004170 ) ) ;
#36016 = CARTESIAN_POINT ( 'NONE',  ( 15.24356964374999990, 3.323476615752268604, -0.6281249993854746139 ) ) ;
#36017 = CARTESIAN_POINT ( 'NONE',  ( -13.23911966647199812, 136.1523137178985507, -8.632099005475788900 ) ) ;
#36018 = CARTESIAN_POINT ( 'NONE',  ( 18.91622474583366653, 5.725135026351895640, -10.38020280809387863 ) ) ;
#36019 = VERTEX_POINT ( 'NONE', #14720 ) ;
#36020 = CARTESIAN_POINT ( 'NONE',  ( 10.31873187879410736, 0.000000000000000000, -5.146874999385541827 ) ) ;
#36021 = VERTEX_POINT ( 'NONE', #31411 ) ;
#36022 = CARTESIAN_POINT ( 'NONE',  ( 13.62178482187501416, 195.4531250006145342, 23.59362340125806767 ) ) ;
#36023 = CARTESIAN_POINT ( 'NONE',  ( 8.715434833791931624, 128.8601862821014663, 8.962234695871760692 ) ) ;
#36024 = CARTESIAN_POINT ( 'NONE',  ( 37.13187018199665346, 7.646167579472024665E-16, 162.7511921998298590 ) ) ;
#36025 = CARTESIAN_POINT ( 'NONE',  ( -53.95461230271185116, 207.6069050685336492, -8.469044688360751749 ) ) ;
#36026 = CARTESIAN_POINT ( 'NONE',  ( 26.75643035624999655, 247.7218750006145171, -7.049594010296217766E-16 ) ) ;
#36027 = CARTESIAN_POINT ( 'NONE',  ( -27.00000000000000355, 199.2125000012290457, 0.000000000000000000 ) ) ;
#36028 = ADVANCED_FACE ( 'NONE', ( #20418 ), #11501, .T. ) ;
#36029 = CARTESIAN_POINT ( 'NONE',  ( -49.40252896937850124, 207.6499508600178387, -3.839350919129087547 ) ) ;
#36030 = FACE_OUTER_BOUND ( 'NONE', #15020, .T. ) ;
#36031 = CARTESIAN_POINT ( 'NONE',  ( 34.34716455898865206, 5.407089921784857367, 166.7403251419335390 ) ) ;
#36032 = ORIENTED_EDGE ( 'NONE', *, *, #25579, .F. ) ;
#36033 = AXIS2_PLACEMENT_3D ( 'NONE', #11495, #31406, #20222 ) ;
#36034 = CARTESIAN_POINT ( 'NONE',  ( 13.49999999999999645, 195.4625000012290172, -23.38268590217984766 ) ) ;
#36035 = CARTESIAN_POINT ( 'NONE',  ( 2.908627838312118019, 129.7226862821014208, 15.53471296425195369 ) ) ;
#36036 = CARTESIAN_POINT ( 'NONE',  ( -47.82663769728823411, 202.5810206699313767, 4.149950860017909804 ) ) ;
#36037 = ADVANCED_FACE ( 'NONE', ( #5805 ), #25534, .T. ) ;
#36038 = CARTESIAN_POINT ( 'NONE',  ( 8.843639120294328748, 117.9351862821014407, -3.474262827703334722 ) ) ;
#36039 = FACE_BOUND ( 'NONE', #7267, .T. ) ;
#36040 = CARTESIAN_POINT ( 'NONE',  ( 12.53471296425194836, 7.822686282101448896, -2.311890736173178418 ) ) ;
#36041 = CARTESIAN_POINT ( 'NONE',  ( 19.56230152254412502, -5.196152422706635576, -7.500000000000062172 ) ) ;
#36042 = ORIENTED_EDGE ( 'NONE', *, *, #28448, .F. ) ;
#36043 = CYLINDRICAL_SURFACE ( 'NONE', #36080, 7.500000000000000000 ) ;
#36044 = CARTESIAN_POINT ( 'NONE',  ( 15.50000000000000533, 118.5101862821014720, 0.1745138560725827404 ) ) ;
#36045 = CARTESIAN_POINT ( 'NONE',  ( 10.31873187879410914, 0.000000000000000000, -0.1968749993855323233 ) ) ;
#36046 = CARTESIAN_POINT ( 'NONE',  ( -1.715153634034234598, 5.522686282101450850, -9.534712964251941258 ) ) ;
#36047 = CARTESIAN_POINT ( 'NONE',  ( 27.24356964375000700, 198.1906250006145740, 15.72908226750537075 ) ) ;
#36048 = CARTESIAN_POINT ( 'NONE',  ( 13.62178482187501416, 198.6593750006145456, 23.59362340125806767 ) ) ;
#36049 = CARTESIAN_POINT ( 'NONE',  ( 22.46128102716605923, 1.096376214649937619, -10.00000000000000000 ) ) ;
#36050 = DIRECTION ( 'NONE',  ( 0.000000000000000000, 0.000000000000000000, -1.000000000000000000 ) ) ;
#36051 = EDGE_CURVE ( 'NONE', #6034, #30802, #13831, .T. ) ;
#36052 = CARTESIAN_POINT ( 'NONE',  ( 5.529263428287300108, 67.72731371789853938, 7.954856959092309943 ) ) ;
#36053 = VERTEX_POINT ( 'NONE', #23436 ) ;
#36054 = VECTOR ( 'NONE', #11574, 1000.000000000000000 ) ;
#36055 = CARTESIAN_POINT ( 'NONE',  ( 21.00000000000000000, 244.7687500012290513, 6.928203230275506996 ) ) ;
#36056 = CARTESIAN_POINT ( 'NONE',  ( -4.622313124798826500, 87.56481371789855928, 11.61527771782809637 ) ) ;
#36057 = CARTESIAN_POINT ( 'NONE',  ( 22.80587116629411781, -3.604726614523238837, -4.959374999385524951 ) ) ;
#36058 = CARTESIAN_POINT ( 'NONE',  ( -6.580120243182696171, 142.9999999999999432, 10.82695099271156280 ) ) ;
#36059 = CARTESIAN_POINT ( 'NONE',  ( 21.00000000000000000, 6.646953231504538984, -5.315624999385480720 ) ) ;
#36060 = CARTESIAN_POINT ( 'NONE',  ( 11.61527771782809637, 48.46481371789855785, 4.622313124798827388 ) ) ;
#36061 = CIRCLE ( 'NONE', #14260, 2.649999999999999467 ) ;
#36062 = VERTEX_POINT ( 'NONE', #11683 ) ;
#36063 = CARTESIAN_POINT ( 'NONE',  ( 18.12178482187499640, 4.985214923628404904, -6.515624999385460470 ) ) ;
#36064 = CARTESIAN_POINT ( 'NONE',  ( 23.87821517812499650, 243.7468750006145228, -4.985214923628404904 ) ) ;
#36065 = CARTESIAN_POINT ( 'NONE',  ( 12.53471296425194836, 17.02268628210144996, -2.311890736173178418 ) ) ;
#36066 = EDGE_CURVE ( 'NONE', #8199, #1229, #5431, .T. ) ;
#36067 = CARTESIAN_POINT ( 'NONE',  ( -35.94419563604516554, 203.5000000000000000, 0.1155267958017914542 ) ) ;
#36068 = CARTESIAN_POINT ( 'NONE',  ( -56.92336230271182984, 215.6869285224997270, 3.149950860017831200 ) ) ;
#36069 = DIRECTION ( 'NONE',  ( 0.000000000000000000, 0.000000000000000000, 1.000000000000000000 ) ) ;
#36070 = CARTESIAN_POINT ( 'NONE',  ( 4.622313124798831829, 73.76481371789856212, -11.61527771782809282 ) ) ;
#36071 = CARTESIAN_POINT ( 'NONE',  ( -51.98288769728823411, 205.5309553116392465, -1.321298161741839117 ) ) ;
#36072 = CARTESIAN_POINT ( 'NONE',  ( -57.52455436395488420, 205.1570982666397356, 4.673758765035198159 ) ) ;
#36073 = CARTESIAN_POINT ( 'NONE',  ( 20.99999999999999645, 0.000000000000000000, -8.000000000000000000 ) ) ;
#36074 = CARTESIAN_POINT ( 'NONE',  ( 18.00000000000000355, -5.196152422706632912, -3.018749998770942078 ) ) ;
#36075 = CARTESIAN_POINT ( 'NONE',  ( -3.257655550456946880, 63.70231371789854791, -15.46528703574811736 ) ) ;
#36076 = CARTESIAN_POINT ( 'NONE',  ( -46.82961230271182984, 212.3930949314663792, 8.469044688360751749 ) ) ;
#36077 = FACE_OUTER_BOUND ( 'NONE', #13531, .T. ) ;
#36078 = CARTESIAN_POINT ( 'NONE',  ( -7.228626920339069173, 94.07268628210145778, 10.49813415415989581 ) ) ;
#36079 = CARTESIAN_POINT ( 'NONE',  ( -5.770363421893818234, 23.63518628210144357, -14.38691631536207005 ) ) ;
#36080 = AXIS2_PLACEMENT_3D ( 'NONE', #6492, #18066, #35477 ) ;
#36081 = CARTESIAN_POINT ( 'NONE',  ( 10.56230152254410370, 3.464101615137757051, -0.03749999999999697325 ) ) ;
#36082 = CARTESIAN_POINT ( 'NONE',  ( 15.00000000000000000, 244.1687500012290286, -3.464101615137752610 ) ) ;
#36083 = ORIENTED_EDGE ( 'NONE', *, *, #31697, .F. ) ;
#36084 = CARTESIAN_POINT ( 'NONE',  ( 15.50000000000000533, 35.71018628210144641, 0.1745138560725827404 ) ) ;
#36085 = CARTESIAN_POINT ( 'NONE',  ( 5.778771075727756162E-15, 196.7656250006145342, 31.45816453501076637 ) ) ;
#36086 = CARTESIAN_POINT ( 'NONE',  ( 18.06230152254410726, 1.836970198721030427E-16, 10.00000000000000000 ) ) ;
#36087 = CARTESIAN_POINT ( 'NONE',  ( -7.234628195640302017, 199.1924038105676686, 27.00000000000000711 ) ) ;
#36088 = CARTESIAN_POINT ( 'NONE',  ( -41.88913769728823411, 206.8500491399821044, -5.686928522499717253 ) ) ;
#36089 = CARTESIAN_POINT ( 'NONE',  ( 20.99999999999999645, 185.0294372515228645, 0.000000000000000000 ) ) ;
#36090 = CARTESIAN_POINT ( 'NONE',  ( 6.932735513423970097, 18.74768628210143717, 10.69584247140445044 ) ) ;
#36091 = LINE ( 'NONE', #6732, #11128 ) ;
#36092 = CARTESIAN_POINT ( 'NONE',  ( 5.233372021372610483, 129.2523137178985451, -8.152565276336593669 ) ) ;
#36093 = CARTESIAN_POINT ( 'NONE',  ( 20.99999999999999645, 245.2468750006145797, -6.646953231504538984 ) ) ;
#36094 = ORIENTED_EDGE ( 'NONE', *, *, #35496, .F. ) ;
#36095 = AXIS2_PLACEMENT_3D ( 'NONE', #2649, #25592, #5127 ) ;
#36096 = LINE ( 'NONE', #35396, #23502 ) ;
#36097 = CARTESIAN_POINT ( 'NONE',  ( 10.49813415416005213, 129.8273137178985621, -7.228626920338837358 ) ) ;
#36098 = ADVANCED_FACE ( 'NONE', ( #37272 ), #37086, .T. ) ;
#36099 = CARTESIAN_POINT ( 'NONE',  ( 22.80587116629410360, -3.604726614523235284, -6.253124999385533123 ) ) ;
#36100 = CARTESIAN_POINT ( 'NONE',  ( 24.79193261022362549, 3.604726614523236616, 164.9789157851677146 ) ) ;
#36101 = CARTESIAN_POINT ( 'NONE',  ( 14.99999999999982414, 3.464101615137652246, -1.837499999999977929 ) ) ;
#36102 = CARTESIAN_POINT ( 'NONE',  ( 27.00000000000000355, 198.4250000000000114, -3.306546357697854128E-15 ) ) ;
#36103 = VERTEX_POINT ( 'NONE', #20229 ) ;
#36104 = CARTESIAN_POINT ( 'NONE',  ( 8.962234695871762469, 34.56018628210144783, -8.715434833791931624 ) ) ;
#36105 = VERTEX_POINT ( 'NONE', #13982 ) ;
#36106 = ORIENTED_EDGE ( 'NONE', *, *, #30952, .F. ) ;
#36107 = CARTESIAN_POINT ( 'NONE',  ( 10.49999999999999467, 222.9518338469886203, 2.500000000000000000 ) ) ;
#36108 = CARTESIAN_POINT ( 'NONE',  ( 23.87821517812500005, -4.985214923628404016, -0.4406249993854638447 ) ) ;
#36109 = CARTESIAN_POINT ( 'NONE',  ( 14.99999999999999822, 204.0000000000000284, -3.514718625761426019 ) ) ;
#36110 = CARTESIAN_POINT ( 'NONE',  ( -26.99999999999999645, 196.4375000000000284, 15.58845726811991561 ) ) ;
#36111 = CARTESIAN_POINT ( 'NONE',  ( 26.75643035624999655, 7.049594010296217766E-16, -9.815624999385457627 ) ) ;
#36112 = CARTESIAN_POINT ( 'NONE',  ( 10.49813415415989581, 73.37268628210144072, 7.228626920339068285 ) ) ;
#36113 = EDGE_CURVE ( 'NONE', #17469, #10453, #30534, .T. ) ;
#36114 = CARTESIAN_POINT ( 'NONE',  ( -15.50000000000000533, 132.3101862821014549, -0.1745138560725808530 ) ) ;
#36115 = EDGE_CURVE ( 'NONE', #29774, #20600, #3299, .T. ) ;
#36116 = CARTESIAN_POINT ( 'NONE',  ( 21.00000000000000000, 243.4187500012290002, 5.999999999999998224 ) ) ;
#36117 = CARTESIAN_POINT ( 'NONE',  ( 20.60729646369923529, 211.0472094301353536, 5.999999999999996447 ) ) ;
#36118 = CARTESIAN_POINT ( 'NONE',  ( -49.79836230271183695, 206.0451222850691977, -2.149950860017851184 ) ) ;
#36119 = CARTESIAN_POINT ( 'NONE',  ( 0.000000000000000000, 200.0000000000000000, 0.000000000000000000 ) ) ;
#36120 = CARTESIAN_POINT ( 'NONE',  ( 31.18414854017020232, 6.928203230275506996, 166.4053504732449085 ) ) ;
#36121 = CARTESIAN_POINT ( 'NONE',  ( -9.500000000000005329, 6.489813717898557321, 0.1745138560723101806 ) ) ;
#36122 = CARTESIAN_POINT ( 'NONE',  ( -41.49330436395490551, 210.1155267958017134, -6.500000000000000888 ) ) ;
#36123 = CARTESIAN_POINT ( 'NONE',  ( -59.50372103062157692, 218.5309553116391896, -2.162041339862839084 ) ) ;
#36124 = CARTESIAN_POINT ( 'NONE',  ( 18.12178482187500350, -4.985214923628407568, -1.528124999385482852 ) ) ;
#36125 = CARTESIAN_POINT ( 'NONE',  ( -27.24356964374999635, 199.3906250006145342, 15.72908226750539384 ) ) ;
#36126 = CARTESIAN_POINT ( 'NONE',  ( -15.46528703574811736, 116.6023137178985394, 3.257655550456946436 ) ) ;
#36127 = CARTESIAN_POINT ( 'NONE',  ( -48.61086230271182984, 213.1499508600178387, -5.686928522499747451 ) ) ;
#36128 = VECTOR ( 'NONE', #26095, 1000.000000000000000 ) ;
#36129 = EDGE_LOOP ( 'NONE', ( #27879, #21468, #7249, #15947 ) ) ;
#36130 = DIRECTION ( 'NONE',  ( 0.8660254037844187236, -0.5000000000000346390, 0.000000000000000000 ) ) ;
#36131 = CARTESIAN_POINT ( 'NONE',  ( -4.622313124798576922, 134.0351862821014493, -11.61527771782819762 ) ) ;
#36132 = CYLINDRICAL_SURFACE ( 'NONE', #10211, 3.500000000000003109 ) ;
#36133 = CARTESIAN_POINT ( 'NONE',  ( 30.92186422678543778, 7.209453229046482114, 163.4074270530628894 ) ) ;
#36134 = CARTESIAN_POINT ( 'NONE',  ( -8.632099005475501130, 96.94768628210147199, -13.23911966647218996 ) ) ;
#36135 = CARTESIAN_POINT ( 'NONE',  ( -60.69122103062155560, 208.3738570449994256, -6.530955311639227823 ) ) ;
#36136 = CARTESIAN_POINT ( 'NONE',  ( 10.31873187879411091, -3.604726614523240613, -3.253124999385518912 ) ) ;
#36137 = CARTESIAN_POINT ( 'NONE',  ( -8.710071997420127943, 40.88518628210145067, -3.796722387233380402 ) ) ;
#36138 = CARTESIAN_POINT ( 'NONE',  ( 15.00000000000000000, 246.4000000000000057, 0.000000000000000000 ) ) ;
#36139 = CARTESIAN_POINT ( 'NONE',  ( -32.78497103062156981, 202.6965474657331185, -4.350049139982091084 ) ) ;
#36140 = CARTESIAN_POINT ( 'NONE',  ( 16.56230152254411792, 7.209453229046482114, -9.759374999385554972 ) ) ;
#36141 = CARTESIAN_POINT ( 'NONE',  ( -6.932735513423968321, 78.54768628210146630, -10.69584247140445221 ) ) ;
#36142 = CARTESIAN_POINT ( 'NONE',  ( 27.00000000000001066, 199.2875000000000227, 15.58845726811988897 ) ) ;
#36144 = FACE_OUTER_BOUND ( 'NONE', #22883, .T. ) ;
#36143 = CARTESIAN_POINT ( 'NONE',  ( -9.500000000000005329, 40.31018628210145494, -0.1745138560725176813 ) ) ;
#36145 = CARTESIAN_POINT ( 'NONE',  ( 13.49999999999999645, 198.6125000012290513, -23.38268590217984766 ) ) ;
#36146 = EDGE_LOOP ( 'NONE', ( #25350, #25032, #4917, #27540, #23377, #24605 ) ) ;
#36147 = CARTESIAN_POINT ( 'NONE',  ( 18.00000000000000355, -5.196152422706632912, -2.624999999999988454 ) ) ;
#36148 = CARTESIAN_POINT ( 'NONE',  ( 24.67590652769082027, -3.604726614523244610, 163.6527315933331295 ) ) ;
#36149 = CARTESIAN_POINT ( 'NONE',  ( 36.74623750377789122, -3.464101615137755275, 161.1380387658727216 ) ) ;
#36150 = CARTESIAN_POINT ( 'NONE',  ( 15.00000000000000000, 245.0124999999999602, -3.464101615137752166 ) ) ;
#36151 = CARTESIAN_POINT ( 'NONE',  ( 22.56230152254386923, 3.464101615137892942, -4.124999998771019527 ) ) ;
#36152 = CARTESIAN_POINT ( 'NONE',  ( 4.944772684328420986, 77.21481371789855075, 11.48171059495408208 ) ) ;
#36153 = CARTESIAN_POINT ( 'NONE',  ( 8.715434833791931624, 82.86018628210145209, 8.962234695871760692 ) ) ;
#36154 = ORIENTED_EDGE ( 'NONE', *, *, #35816, .F. ) ;
#36155 = VERTEX_POINT ( 'NONE', #28553 ) ;
#36156 = CARTESIAN_POINT ( 'NONE',  ( -1.909035429704832693E-15, 197.7500000012290400, -31.17691453623979214 ) ) ;
#36157 = CARTESIAN_POINT ( 'NONE',  ( 24.00000000000000000, -5.196152422706629359, -3.899999999999987033 ) ) ;
#36158 = CARTESIAN_POINT ( 'NONE',  ( -5.770363421894122880, 59.96481371789855075, 14.38691631536194393 ) ) ;
#36159 = CARTESIAN_POINT ( 'NONE',  ( 26.75643035624999655, 7.049594010296217766E-16, -7.228124999385493687 ) ) ;
#36160 = CARTESIAN_POINT ( 'NONE',  ( 15.24356964374999990, 246.2218750006145456, -3.323476615752268604 ) ) ;
#36161 = CARTESIAN_POINT ( 'NONE',  ( -53.76413769728823411, 212.1499508600178387, 3.954877714930865817 ) ) ;
#36162 = CARTESIAN_POINT ( 'NONE',  ( -13.50000000000000533, 195.0875000012290457, -23.38268590217984411 ) ) ;
#36163 = CARTESIAN_POINT ( 'NONE',  ( -1.715153634034442431, 59.67731371789855643, 9.534712964251900402 ) ) ;
#36164 = CARTESIAN_POINT ( 'NONE',  ( 22.80587116629411071, -3.604726614523235284, -7.153124999385557459 ) ) ;
#36165 =( BOUNDED_CURVE ( )  B_SPLINE_CURVE ( 2, ( #12523, #15178, #24086, #23521, #20877, #18220, #26725, #1136, #35631 ),
 .UNSPECIFIED., .F., .F. ) 
 B_SPLINE_CURVE_WITH_KNOTS ( ( 3, 2, 2, 2, 3 ),
 ( 0.1875000000000000000, 0.1944444444444444475, 0.2083333333333333426, 0.2222222222222222099, 0.2291666666666666574 ),
 .UNSPECIFIED. ) 
 CURVE ( )  GEOMETRIC_REPRESENTATION_ITEM ( )  RATIONAL_B_SPLINE_CURVE ( ( 0.9330127018922194093, 0.9330127018922194093, 1.000000000000000000, 0.8660254037844387076, 1.000000000000000000, 0.8660254037844387076, 1.000000000000000000, 0.9330127018922194093, 0.9330127018922194093 ) ) 
 REPRESENTATION_ITEM ( '' )  );
#36166 = CARTESIAN_POINT ( 'NONE',  ( -9.534712964251895073, 117.1773137178985706, -1.715153634034446428 ) ) ;
#36167 = CARTESIAN_POINT ( 'NONE',  ( 7.234628195640295800, 197.8825961894323484, 27.00000000000001066 ) ) ;
#36168 = CARTESIAN_POINT ( 'NONE',  ( 11.48171059495408208, 38.11481371789854222, -4.944772684328420986 ) ) ;
#36169 = CARTESIAN_POINT ( 'NONE',  ( 12.46528703574805874, 81.99768628210146915, 2.660918448318279950 ) ) ;
#36170 = CARTESIAN_POINT ( 'NONE',  ( 10.56230152254411436, -3.464101615137757051, -7.949999998771033916 ) ) ;
#36171 = CARTESIAN_POINT ( 'NONE',  ( 21.00000000000016342, -4.000000000000002665, 50.00000000000000000 ) ) ;
#36172 = CARTESIAN_POINT ( 'NONE',  ( 24.64158895398392701, -3.604726614523240613, 163.2604799309594910 ) ) ;
#36173 = CARTESIAN_POINT ( 'NONE',  ( 10.31873187879410736, 0.000000000000000000, -5.596874999385520688 ) ) ;
#36174 = CARTESIAN_POINT ( 'NONE',  ( 20.99999999999999645, -6.928203230275506996, -0.7875000000000005329 ) ) ;
#36175 = CARTESIAN_POINT ( 'NONE',  ( 27.00000000000047251, -3.464101615137475942, -3.806249998770962151 ) ) ;
#36176 = CARTESIAN_POINT ( 'NONE',  ( 10.56230152254410903, 7.347880794884117764E-16, -10.00000000000000000 ) ) ;
#36177 = CARTESIAN_POINT ( 'NONE',  ( -8.152565276336710909, 103.8476862821014493, 5.233372021372435512 ) ) ;
#36178 = CARTESIAN_POINT ( 'NONE',  ( 18.00000000000000000, 248.1812500012290457, -5.196152422706630247 ) ) ;
#36179 =( BOUNDED_CURVE ( )  B_SPLINE_CURVE ( 2, ( #29071, #5771, #269, #20010, #34770, #5396, #11286 ),
 .UNSPECIFIED., .F., .F. ) 
 B_SPLINE_CURVE_WITH_KNOTS ( ( 3, 2, 2, 3 ),
 ( 0.1521739130434776044, 0.1594202898550718950, 0.1666666666666661856, 0.1739130434782605039 ),
 .UNSPECIFIED. ) 
 CURVE ( )  GEOMETRIC_REPRESENTATION_ITEM ( )  RATIONAL_B_SPLINE_CURVE ( ( 1.000000000000012212, 0.8660254037844263841, 1.000000000000000000, 0.8660254037844387076, 1.000000000000000000, 0.8660254037844453689, 0.9999999999999933387 ) ) 
 REPRESENTATION_ITEM ( '' )  );
#36180 = CARTESIAN_POINT ( 'NONE',  ( -12.50000000000000355, 132.3101862821014549, -0.1745138560725492671 ) ) ;
#36181 = CARTESIAN_POINT ( 'NONE',  ( 22.56230152254361698, 3.464101615138050150, -3.337500000000045208 ) ) ;
#36182 = CARTESIAN_POINT ( 'NONE',  ( 26.75643035624999655, 240.1093750006145342, -3.323476615752271712 ) ) ;
#36183 = ORIENTED_EDGE ( 'NONE', *, *, #3543, .F. ) ;
#36184 = CARTESIAN_POINT ( 'NONE',  ( 37.14004103287923186, 3.604726614523238837, 162.8445854527759309 ) ) ;
#36185 = CIRCLE ( 'NONE', #19284, 2.649999999999990585 ) ;
#36186 = CARTESIAN_POINT ( 'NONE',  ( 18.12178482187499640, 4.985214923628404904, -5.165624999385470595 ) ) ;
#36187 = CARTESIAN_POINT ( 'NONE',  ( -1.926257025242585782E-15, 197.9468750006145399, -31.45816453501076637 ) ) ;
#36188 = FACE_OUTER_BOUND ( 'NONE', #21951, .T. ) ;
#36189 = CARTESIAN_POINT ( 'NONE',  ( 19.95811093400027403, 239.6067736145540152, -5.908846518073574750 ) ) ;
#36190 = CARTESIAN_POINT ( 'NONE',  ( 23.87821517812500005, 243.2593750006145399, 4.985214923628404016 ) ) ;
#36191 = CARTESIAN_POINT ( 'NONE',  ( 2.311890736173452865, 137.8773137178986019, -12.53471296425189152 ) ) ;
#36192 = CARTESIAN_POINT ( 'NONE',  ( -27.24356964375000345, 196.2218750006145456, -15.72908226750537786 ) ) ;
#36194 = VERTEX_POINT ( 'NONE', #14165 ) ;
#36193 = ORIENTED_EDGE ( 'NONE', *, *, #4615, .T. ) ;
#36195 = CARTESIAN_POINT ( 'NONE',  ( 21.00000000000000000, 243.7843750006144887, -6.646953231504538984 ) ) ;
#36196 = CARTESIAN_POINT ( 'NONE',  ( -4.622313124798826500, 23.16481371789855359, 11.61527771782809637 ) ) ;
#36197 = CARTESIAN_POINT ( 'NONE',  ( 21.00000000000000000, 6.646953231504538984, -3.403124999385474858 ) ) ;
#36198 = CARTESIAN_POINT ( 'NONE',  ( 13.04141134922778988, 111.4273137178985422, -8.927990412390371944 ) ) ;
#36199 = CARTESIAN_POINT ( 'NONE',  ( 26.99999999999999645, -3.464101615137751278, -9.656249998770976006 ) ) ;
#36200 = VECTOR ( 'NONE', #24356, 1000.000000000000000 ) ;
#36201 = ORIENTED_EDGE ( 'NONE', *, *, #28836, .F. ) ;
#36202 = CARTESIAN_POINT ( 'NONE',  ( 13.44051670066911086, 5.407089921784862696, -6.121874999385518379 ) ) ;
#36203 = ORIENTED_EDGE ( 'NONE', *, *, #34648, .F. ) ;
#36204 = CARTESIAN_POINT ( 'NONE',  ( 5.778771075727756162E-15, 196.7656250006145342, 31.45816453501075927 ) ) ;
#36205 = CARTESIAN_POINT ( 'NONE',  ( -12.50000000000000355, 132.3101862821014549, -0.1745138560725492671 ) ) ;
#36206 = CARTESIAN_POINT ( 'NONE',  ( 10.31873187879410914, 0.000000000000000000, -0.5906249993855583469 ) ) ;
#36207 = CARTESIAN_POINT ( 'NONE',  ( 24.47980610650859390, -3.604726614523244610, 161.4112935226266359 ) ) ;
#36208 = CARTESIAN_POINT ( 'NONE',  ( -59.69419563604517265, 201.5000000000000000, 0.1155267958018195706 ) ) ;
#36209 = VECTOR ( 'NONE', #19063, 1000.000000000000000 ) ;
#36210 = CARTESIAN_POINT ( 'NONE',  ( 18.12178482187500350, 247.1218750006145228, 4.985214923628407568 ) ) ;
#36211 =( LENGTH_UNIT ( ) NAMED_UNIT ( * ) SI_UNIT ( .MILLI., .METRE. ) );
#36212 = CARTESIAN_POINT ( 'NONE',  ( 19.56230152254410370, 5.196152422706631135, -2.737499998770986931 ) ) ;
#36213 = CARTESIAN_POINT ( 'NONE',  ( -41.88169563604517265, 210.1155267958017703, 4.499999999999996447 ) ) ;
#36214 = CARTESIAN_POINT ( 'NONE',  ( -0.1745138560725500443, 139.2101862821014606, 12.50000000000000355 ) ) ;
#36215 = CARTESIAN_POINT ( 'NONE',  ( 14.39393461504979399, 5.957546011302761180, -10.18332779764974383 ) ) ;
#36216 = VERTEX_POINT ( 'NONE', #34253 ) ;
#36217 = CARTESIAN_POINT ( 'NONE',  ( -13.50000000000000533, 195.0875000012290457, -23.38268590217984411 ) ) ;
#36218 = CARTESIAN_POINT ( 'NONE',  ( -0.1745138560725817967, 111.6101862821014521, 15.50000000000000533 ) ) ;
#36219 = CARTESIAN_POINT ( 'NONE',  ( -50.20163769728823411, 217.4189793300686233, -4.149950860017907139 ) ) ;
#36220 =( BOUNDED_CURVE ( )  B_SPLINE_CURVE ( 2, ( #14461, #22998, #11800, #8587, #26017, #23185, #34732 ),
 .UNSPECIFIED., .F., .F. ) 
 B_SPLINE_CURVE_WITH_KNOTS ( ( 3, 2, 2, 3 ),
 ( 0.1521739130434777709, 0.1594202898550720338, 0.1666666666666663243, 0.1739130434782606149 ),
 .UNSPECIFIED. ) 
 CURVE ( )  GEOMETRIC_REPRESENTATION_ITEM ( )  RATIONAL_B_SPLINE_CURVE ( ( 1.000000000000009326, 0.8660254037844296038, 1.000000000000000000, 0.8660254037844387076, 1.000000000000000000, 0.8660254037844433705, 0.9999999999999953371 ) ) 
 REPRESENTATION_ITEM ( '' )  );
#36221 = CARTESIAN_POINT ( 'NONE',  ( -0.1745138560725182642, 111.6101862821014521, 9.500000000000005329 ) ) ;
#36222 = DIRECTION ( 'NONE',  ( 1.000000000000000000, 0.000000000000000000, 0.000000000000000000 ) ) ;
#36223 = CARTESIAN_POINT ( 'NONE',  ( 10.69584247140445221, 7.247686282101428290, -6.932735513423970097 ) ) ;
#36224 = EDGE_CURVE ( 'NONE', #31196, #9403, #8623, .T. ) ;
#36225 = CARTESIAN_POINT ( 'NONE',  ( 10.56230152254410548, 0.000000000000000000, -9.000000000000035527 ) ) ;
#36226 = AXIS2_PLACEMENT_3D ( 'NONE', #21934, #35755, #9799 ) ;
#36227 = ORIENTED_EDGE ( 'NONE', *, *, #36458, .T. ) ;
#36228 = CARTESIAN_POINT ( 'NONE',  ( 20.99999999999999645, 185.0294372515228645, 0.000000000000000000 ) ) ;
#36229 = CARTESIAN_POINT ( 'NONE',  ( 3.796722387233379514, 89.18518628210145494, -8.710071997420127943 ) ) ;
#36230 = CARTESIAN_POINT ( 'NONE',  ( 20.99999999999999645, 185.0294372515228645, 0.000000000000000000 ) ) ;
#36231 = CARTESIAN_POINT ( 'NONE',  ( -9.465287035748106703, 125.8023137178985706, 2.064181346179061460 ) ) ;
#36232 = CARTESIAN_POINT ( 'NONE',  ( 27.24356964374999635, 195.1156250006145001, -15.72908226750539029 ) ) ;
#36233 = CARTESIAN_POINT ( 'NONE',  ( -13.62178482187498396, 198.1343750006145399, 23.59362340125808188 ) ) ;
#36234 = DIRECTION ( 'NONE',  ( 0.000000000000000000, 0.000000000000000000, 1.000000000000000000 ) ) ;
#36235 = FACE_OUTER_BOUND ( 'NONE', #31438, .T. ) ;
#36236 = EDGE_CURVE ( 'NONE', #17991, #20530, #22916, .T. ) ;
#36237 = CARTESIAN_POINT ( 'NONE',  ( -1.715153634034442431, 59.67731371789855643, 9.534712964251900402 ) ) ;
#36238 = VERTEX_POINT ( 'NONE', #8660 ) ;
#36239 = CARTESIAN_POINT ( 'NONE',  ( 15.00000000000000178, 245.1437500012290513, 3.464101615137757051 ) ) ;
#36240 = CARTESIAN_POINT ( 'NONE',  ( 2.660918448318003282, 86.70231371789854791, 12.46528703574811558 ) ) ;
#36241 = CARTESIAN_POINT ( 'NONE',  ( 22.80587116629411781, 7.646167579472024665E-16, -5.371874999385517491 ) ) ;
#36242 = CARTESIAN_POINT ( 'NONE',  ( -9.164001878794323375, 143.0000000000000000, 9.815649414211552681 ) ) ;
#36243 = CARTESIAN_POINT ( 'NONE',  ( 26.75643035624999655, 3.323476615752271712, -8.090624999385481075 ) ) ;
#36244 = CARTESIAN_POINT ( 'NONE',  ( -8.715434833792127023, 42.13981371789854791, 8.962234695871568846 ) ) ;
#36245 = ORIENTED_EDGE ( 'NONE', *, *, #9709, .T. ) ;
#36246 = CARTESIAN_POINT ( 'NONE',  ( 18.12178482187499640, 4.985214923628404904, -6.965624999385466865 ) ) ;
#36247 = EDGE_CURVE ( 'NONE', #26157, #7551, #2093, .T. ) ;
#36248 = CARTESIAN_POINT ( 'NONE',  ( 12.46528703574805874, 26.79768628210144144, 2.660918448318279950 ) ) ;
#36249 = CARTESIAN_POINT ( 'NONE',  ( 34.40762885551985306, -5.407089921784861808, 167.4314352137346873 ) ) ;
#36250 = CARTESIAN_POINT ( 'NONE',  ( -57.12127896937847993, 216.5309553116391612, 1.626142955000506873 ) ) ;
#36251 = FILL_AREA_STYLE ('',( #22426 ) ) ;
#36252 = CARTESIAN_POINT ( 'NONE',  ( 36.56321044411491528, 7.347880794884117764E-16, 159.0460299011043901 ) ) ;
#36253 = CARTESIAN_POINT ( 'NONE',  ( 12.46528703574811558, 66.00231371789855928, -2.660918448318005503 ) ) ;
#36254 = CARTESIAN_POINT ( 'NONE',  ( -50.39955436395490551, 213.3788001182225003, -3.209657149897400252 ) ) ;
#36255 = CARTESIAN_POINT ( 'NONE',  ( -56.73288769728823411, 203.5309553116391612, -1.857196546604028775 ) ) ;
#36256 = B_SPLINE_CURVE_WITH_KNOTS ( 'NONE', 3,
 ( #12067, #23449, #35185, #3351, #26282, #31422, #25731, #8671, #34448, #35002, #19880, #37282, #25917, #17024, #11330, #5627, #2603, #23642, #31602, #17769, #5819, #8489, #2976, #20433, #20058, #316, #28564, #17210, #9045, #28751, #20617, #2789, #34627, #14362, #14546, #20242, #37462, #11512 ),
 .UNSPECIFIED., .F., .F.,
 ( 4, 2, 2, 2, 2, 2, 2, 2, 2, 2, 2, 2, 2, 2, 2, 2, 2, 2, 4 ),
 ( 0.000000000000000000, 0.003347226634339490244, 0.006694453268678980488, 0.01004167990301847030, 0.01171529322018821477, 0.01338890653735796098, 0.02008335980603693019, 0.02175697312320667293, 0.02343058644037641566, 0.02677781307471589767, 0.03012503970905539008, 0.03179865302622512935, 0.03347226634339488249, 0.03681949297773436103, 0.04016671961207383262, 0.04686117288075281051, 0.04853478619792254978, 0.05020839951509228904, 0.05355562614943176064 ),
 .UNSPECIFIED. ) ;
#36257 = CARTESIAN_POINT ( 'NONE',  ( -7.234628195640302017, 196.9424038105676971, 27.00000000000000711 ) ) ;
#36258 = CARTESIAN_POINT ( 'NONE',  ( -6.797732988389737052, 221.2600366402566010, -2.615528913832024127 ) ) ;
#36259 = CARTESIAN_POINT ( 'NONE',  ( -10.83675517735179028, 42.13981371789854791, 11.08355503943118947 ) ) ;
#36260 = CARTESIAN_POINT ( 'NONE',  ( -47.81919563604517265, 218.5000000000000000, -0.1155267958018185298 ) ) ;
#36261 = CARTESIAN_POINT ( 'NONE',  ( 20.99999999999999645, 185.0294372515228645, 0.000000000000000000 ) ) ;
#36262 = CARTESIAN_POINT ( 'NONE',  ( -12.50000000000000355, 67.91018628210144925, -0.1745138560725492671 ) ) ;
#36263 = CARTESIAN_POINT ( 'NONE',  ( 14.38691631536207538, 35.13518628210143646, -5.770363421893813793 ) ) ;
#36264 = CARTESIAN_POINT ( 'NONE',  ( 22.56230152254412147, 3.464101615137759271, -3.337500000000051426 ) ) ;
#36265 = ORIENTED_EDGE ( 'NONE', *, *, #2054, .F. ) ;
#36266 = CARTESIAN_POINT ( 'NONE',  ( -2.908627838312119351, 33.12268628210143362, -15.53471296425195369 ) ) ;
#36267 = CARTESIAN_POINT ( 'NONE',  ( 27.24356964374999279, 197.8156250006145171, -15.72908226750539207 ) ) ;
#36268 = EDGE_CURVE ( 'NONE', #13971, #15757, #6514, .T. ) ;
#36269 = CARTESIAN_POINT ( 'NONE',  ( 19.56230152254410370, 5.196152422706631135, -8.587499998771008336 ) ) ;
#36270 = DIRECTION ( 'NONE',  ( -1.000000000000000000, -6.123233995736766036E-17, 0.000000000000000000 ) ) ;
#36271 = CARTESIAN_POINT ( 'NONE',  ( -41.09747103062156981, 213.3500491399821328, -5.571401726697985168 ) ) ;
#36272 = DIRECTION ( 'NONE',  ( 1.000000000000000000, 0.000000000000000000, 0.000000000000000000 ) ) ;
#36273 = CARTESIAN_POINT ( 'NONE',  ( 23.87821517812499650, 247.9093750006145171, -4.985214923628404904 ) ) ;
#36274 = CARTESIAN_POINT ( 'NONE',  ( -6.594114490232462877, 124.9398137178985451, 6.840914352311949109 ) ) ;
#36275 = CARTESIAN_POINT ( 'NONE',  ( 15.24356964374999990, 244.9093750006145171, 0.000000000000000000 ) ) ;
#36276 = ORIENTED_EDGE ( 'NONE', *, *, #32573, .T. ) ;
#36277 = CARTESIAN_POINT ( 'NONE',  ( 10.56230152254474497, -3.464101615138128754, -7.162500000000022737 ) ) ;
#36278 = DIRECTION ( 'NONE',  ( 1.000000000000000000, 0.000000000000000000, 0.000000000000000000 ) ) ;
#36279 = CARTESIAN_POINT ( 'NONE',  ( -29.50000000000000711, 237.0000000000000000, 2.500000000000005329 ) ) ;
#36280 = CARTESIAN_POINT ( 'NONE',  ( 22.80587116629410360, 7.646167579472015790E-16, -6.665624999385527438 ) ) ;
#36281 = CARTESIAN_POINT ( 'NONE',  ( 24.83442103481310781, 0.000000000000000000, 165.4645607004874535 ) ) ;
#36282 = CARTESIAN_POINT ( 'NONE',  ( -69.00000000000002842, 214.0000000000000000, 2.500000000000000000 ) ) ;
#36283 = CARTESIAN_POINT ( 'NONE',  ( -13.49999999999998401, 197.8249999999999886, 23.38268590217985476 ) ) ;
#36284 = VERTEX_POINT ( 'NONE', #9595 ) ;
#36285 = SHAPE_REPRESENTATION ( 'follower spring', ( #17215 ), #1426 ) ;
#36286 = CARTESIAN_POINT ( 'NONE',  ( 11.48171059495397728, 36.28518628210144925, 4.944772684328674117 ) ) ;
#36287 = ORIENTED_EDGE ( 'NONE', *, *, #34894, .F. ) ;
#36288 = VERTEX_POINT ( 'NONE', #32516 ) ;
#36289 = CARTESIAN_POINT ( 'NONE',  ( 26.99999999999999645, 3.464101615137755275, -5.081249998770961618 ) ) ;
#36290 = LINE ( 'NONE', #15846, #27415 ) ;
#36291 = DIRECTION ( 'NONE',  ( 0.000000000000000000, 0.000000000000000000, -1.000000000000000000 ) ) ;
#36292 = CARTESIAN_POINT ( 'NONE',  ( 18.12178482187499640, 4.985214923628404904, -9.665624999385475036 ) ) ;
#36293 = CARTESIAN_POINT ( 'NONE',  ( 12.50000000000000355, 72.51018628210145778, 0.1745138560725507937 ) ) ;
#36294 = CARTESIAN_POINT ( 'NONE',  ( -15.50000000000000533, 141.5101862821014720, -0.1745138560725808530 ) ) ;
#36295 = CARTESIAN_POINT ( 'NONE',  ( 22.56230152254576993, -3.464101615136805368, -5.662500000000002309 ) ) ;
#36296 = CARTESIAN_POINT ( 'NONE',  ( 36.80179928988602711, 3.464101615138092782, 161.7731128871306225 ) ) ;
#36297 = CARTESIAN_POINT ( 'NONE',  ( -55.73586230271182984, 207.8500491399821613, 3.954877714930852495 ) ) ;
#36298 =( NAMED_UNIT ( * ) PLANE_ANGLE_UNIT ( ) SI_UNIT ( $, .RADIAN. ) );
#36299 = CARTESIAN_POINT ( 'NONE',  ( 28.19883278624800127, 5.196152422706630247, 166.7041750026663181 ) ) ;
#36300 = CARTESIAN_POINT ( 'NONE',  ( 10.49813415416005213, 129.8273137178985905, -7.228626920338837358 ) ) ;
#36301 = CARTESIAN_POINT ( 'NONE',  ( -47.82663769728823411, 204.3130714775002730, 3.149950860017883603 ) ) ;
#36302 = CARTESIAN_POINT ( 'NONE',  ( -57.52455436395489841, 203.6929966515020283, 6.137860380172978303 ) ) ;
#36303 = EDGE_CURVE ( 'NONE', #37392, #33961, #18833, .T. ) ;
#36304 = CARTESIAN_POINT ( 'NONE',  ( 23.87821517812500005, -4.985214923628404016, -1.003124999385485161 ) ) ;
#36305 = CARTESIAN_POINT ( 'NONE',  ( -27.24356964374999635, 197.1406250006145058, 15.72908226750539384 ) ) ;
#36306 = CARTESIAN_POINT ( 'NONE',  ( 8.632099005475788900, 120.0523137178985280, -13.23911966647199812 ) ) ;
#36307 = CARTESIAN_POINT ( 'NONE',  ( -50.59002896937850124, 204.4285982733020433, 3.350049139982171020 ) ) ;
#36308 = ORIENTED_EDGE ( 'NONE', *, *, #12969, .F. ) ;
#36309 = CARTESIAN_POINT ( 'NONE',  ( -27.12178482187499995, 199.7328125009217956, 0.000000000000000000 ) ) ;
#36310 = CARTESIAN_POINT ( 'NONE',  ( 6.932735513423970097, 129.1476862821014890, 10.69584247140445044 ) ) ;
#36311 = CARTESIAN_POINT ( 'NONE',  ( -8.632099005475501130, 78.54768628210145209, -13.23911966647218996 ) ) ;
#36312 = CARTESIAN_POINT ( 'NONE',  ( 26.99999999999999289, 0.000000000000000000, -8.000000000000000000 ) ) ;
#36313 = CARTESIAN_POINT ( 'NONE',  ( 24.78703009969406779, 3.604726614523240613, 164.9228798334000601 ) ) ;
#36314 = CIRCLE ( 'NONE', #8488, 2.649999999999985700 ) ;
#36315 = CARTESIAN_POINT ( 'NONE',  ( -14.25334919248782306, 86.88518628210145778, -6.092822981423979378 ) ) ;
#36316 = CARTESIAN_POINT ( 'NONE',  ( -50.99330436395489841, 210.1155267958017134, -6.500000000000000888 ) ) ;
#36317 = EDGE_CURVE ( 'NONE', #12005, #26168, #24004, .T. ) ;
#36318 = CARTESIAN_POINT ( 'NONE',  ( 13.44051670066911797, -5.407089921784859143, -3.665624999385552751 ) ) ;
#36319 = CARTESIAN_POINT ( 'NONE',  ( -9.465287035748065847, 40.59768628210144215, -2.064181346179273735 ) ) ;
#36320 = CARTESIAN_POINT ( 'NONE',  ( 22.56230152254464727, -3.464101615137448409, -7.462500000000031442 ) ) ;
#36321 = CARTESIAN_POINT ( 'NONE',  ( -41.49330436395490551, 210.1155267958016850, -8.500000000000003553 ) ) ;
#36322 = FACE_OUTER_BOUND ( 'NONE', #12385, .T. ) ;
#36323 = CARTESIAN_POINT ( 'NONE',  ( -2.311890736173176641, 79.12268628210145494, -12.53471296425194836 ) ) ;
#36324 = CARTESIAN_POINT ( 'NONE',  ( 16.56230152254411792, -6.928203230275514990, -8.437500000000024869 ) ) ;
#36325 = PLANE ( 'NONE',  #14160 ) ;
#36327 = CARTESIAN_POINT ( 'NONE',  ( 13.44051670066911441, -5.407089921784865361, -1.021874999385524729 ) ) ;
#36326 = CARTESIAN_POINT ( 'NONE',  ( 9.500000000000005329, 35.71018628210144641, 0.1745138560725188748 ) ) ;
#36328 = DIRECTION ( 'NONE',  ( 1.000000000000000000, 0.000000000000000000, 0.000000000000000000 ) ) ;
#36329 = EDGE_CURVE ( 'NONE', #6323, #10609, #20041, .T. ) ;
#36330 = VERTEX_POINT ( 'NONE', #9218 ) ;
#36331 = CARTESIAN_POINT ( 'NONE',  ( 23.99999999999999645, 5.196152422706631135, -1.500000000000001332 ) ) ;
#36332 = CARTESIAN_POINT ( 'NONE',  ( 33.97620792891898134, -5.407089921784861808, 162.5002714581805492 ) ) ;
#36333 = CARTESIAN_POINT ( 'NONE',  ( 36.66779733530500351, -3.464101615137755275, 160.2414635375901355 ) ) ;
#36334 = CARTESIAN_POINT ( 'NONE',  ( 26.99999999999999645, 247.1125000000000114, -3.464101615137755275 ) ) ;
#36335 = DIRECTION ( 'NONE',  ( 1.000000000000000000, 0.000000000000000000, 0.000000000000000000 ) ) ;
#36336 = CARTESIAN_POINT ( 'NONE',  ( 10.49813415416005213, 83.82731371789856212, -7.228626920338837358 ) ) ;
#36337 = CARTESIAN_POINT ( 'NONE',  ( -12.46528703574805874, 77.39768628210144641, -2.660918448318280838 ) ) ;
#36338 = ORIENTED_EDGE ( 'NONE', *, *, #28562, .T. ) ;
#36339 = B_SPLINE_CURVE_WITH_KNOTS ( 'NONE', 1,
 ( #24998, #13077 ),
 .UNSPECIFIED., .F., .F.,
 ( 2, 2 ),
 ( 0.000000000000000000, 1.000000000000000000 ),
 .UNSPECIFIED. ) ;
#36340 = ORIENTED_EDGE ( 'NONE', *, *, #33116, .T. ) ;
#36341 = CARTESIAN_POINT ( 'NONE',  ( 27.00000000000001066, 197.6000000012290627, 15.58845726811988897 ) ) ;
#36342 = DIRECTION ( 'NONE',  ( -0.5887012860850802110, 0.8083506638593009885, 0.000000000000000000 ) ) ;
#36343 = CARTESIAN_POINT ( 'NONE',  ( -8.632099005475794229, 60.25231371789854506, 13.23911966647199812 ) ) ;
#36344 = CARTESIAN_POINT ( 'NONE',  ( 18.12178482187500350, -4.985214923628407568, -5.578124999385480898 ) ) ;
#36345 = CARTESIAN_POINT ( 'NONE',  ( 21.00000000000000000, 245.9218750006145058, 6.646953231504538984 ) ) ;
#36346 = AXIS2_PLACEMENT_3D ( 'NONE', #4769, #36786, #22033 ) ;
#36347 = CARTESIAN_POINT ( 'NONE',  ( -59.10788769728823411, 214.4690446883608104, 1.321298161741840893 ) ) ;
#36348 = DIRECTION ( 'NONE',  ( -1.000000000000000000, 0.000000000000000000, -0.000000000000000000 ) ) ;
#36349 = CARTESIAN_POINT ( 'NONE',  ( 9.500000000000005329, 47.88981371789855501, -0.1745138560723090149 ) ) ;
#36350 = CARTESIAN_POINT ( 'NONE',  ( 22.80587116629410716, 3.604726614523238837, -7.528124999385559235 ) ) ;
#36351 = CARTESIAN_POINT ( 'NONE',  ( 9.534712964251900402, 103.3773137178985451, 1.715153634034445540 ) ) ;
#36352 = CARTESIAN_POINT ( 'NONE',  ( -1.926257025242585782E-15, 199.2968750006145342, -31.45816453501075927 ) ) ;
#36353 = CARTESIAN_POINT ( 'NONE',  ( -10.49813415416004858, 24.02731371789855785, 7.228626920338839135 ) ) ;
#36354 = EDGE_CURVE ( 'NONE', #12534, #2167, #32859, .T. ) ;
#36355 = CARTESIAN_POINT ( 'NONE',  ( -12.50000000000000355, 86.31018628210145494, -0.1745138560725492671 ) ) ;
#36356 = CARTESIAN_POINT ( 'NONE',  ( 22.56230152254411436, -3.464101615137751278, -8.699999998771005494 ) ) ;
#36357 = FACE_OUTER_BOUND ( 'NONE', #9308, .T. ) ;
#36358 = CARTESIAN_POINT ( 'NONE',  ( 36.97662401522738662, -3.604726614523235284, 160.9767203938538955 ) ) ;
#36359 = CARTESIAN_POINT ( 'NONE',  ( 25.21351703232559061, 3.464101615137630485, 167.0029995320877845 ) ) ;
#36360 = CARTESIAN_POINT ( 'NONE',  ( 22.80587116629411781, 7.646167579472024665E-16, -5.371874999385517491 ) ) ;
#36361 = CARTESIAN_POINT ( 'NONE',  ( 24.00000000000000000, -5.196152422706629359, -0.7500000000000006661 ) ) ;
#36362 = CARTESIAN_POINT ( 'NONE',  ( 0.000000000000000000, -20.00000000000000000, 0.000000000000000000 ) ) ;
#36363 = CARTESIAN_POINT ( 'NONE',  ( -5.529263428287477744, 94.07268628210144357, 7.954856959092191815 ) ) ;
#36364 = LINE ( 'NONE', #10412, #17680 ) ;
#36365 = EDGE_CURVE ( 'NONE', #36641, #19019, #20246, .T. ) ;
#36366 = CARTESIAN_POINT ( 'NONE',  ( 6.932735513423970097, 129.1476862821014890, 10.69584247140445044 ) ) ;
#36367 = CARTESIAN_POINT ( 'NONE',  ( 13.56230152254410903, 5.196152422706636465, -3.225000000000033396 ) ) ;
#36368 = CARTESIAN_POINT ( 'NONE',  ( 21.00000000000000000, 239.9593750006145001, 6.646953231504538984 ) ) ;
#36370 = ORIENTED_EDGE ( 'NONE', *, *, #26959, .T. ) ;
#36369 = CIRCLE ( 'NONE', #647, 7.500000000000000000 ) ;
#36371 = CARTESIAN_POINT ( 'NONE',  ( 31.00520690578787253, 7.209453229046475009, 164.3600382331131868 ) ) ;
#36372 = CARTESIAN_POINT ( 'NONE',  ( 18.12178482187500350, -4.985214923628407568, -5.015624999385459581 ) ) ;
#36373 = CARTESIAN_POINT ( 'NONE',  ( -27.24356964375000345, 198.9218750006145626, -15.72908226750537786 ) ) ;
#36374 = CARTESIAN_POINT ( 'NONE',  ( 31.33122385594975512, 6.928203230275514990, 168.0864290250504212 ) ) ;
#36375 = DIRECTION ( 'NONE',  ( 0.000000000000000000, 0.000000000000000000, 1.000000000000000000 ) ) ;
#36376 = CARTESIAN_POINT ( 'NONE',  ( 15.24356964374999990, 242.2093750006145285, 0.000000000000000000 ) ) ;
#36377 = CARTESIAN_POINT ( 'NONE',  ( 13.56230152254411614, -5.196152422706632912, -7.012499998771043686 ) ) ;
#36378 = CARTESIAN_POINT ( 'NONE',  ( -9.534712964251895073, 6.777313717898553413, -1.715153634034446428 ) ) ;
#36379 = CARTESIAN_POINT ( 'NONE',  ( 5.778771075727756162E-15, 195.0218750006145569, 31.45816453501076637 ) ) ;
#36381 = ORIENTED_EDGE ( 'NONE', *, *, #18282, .F. ) ;
#36380 = ORIENTED_EDGE ( 'NONE', *, *, #5262, .T. ) ;
#36382 = CARTESIAN_POINT ( 'NONE',  ( 18.12178482187500350, 245.7718750006145001, 4.985214923628407568 ) ) ;
#36383 = CARTESIAN_POINT ( 'NONE',  ( -10.49813415416004858, 14.82731371789855501, 7.228626920338840023 ) ) ;
#36384 = CARTESIAN_POINT ( 'NONE',  ( 15.24356964374999990, 0.000000000000000000, -4.640624999385472904 ) ) ;
#36385 = CARTESIAN_POINT ( 'NONE',  ( -15.46528703574811736, 107.4023137178985650, 3.257655550456946436 ) ) ;
#36386 =( BOUNDED_CURVE ( )  B_SPLINE_CURVE ( 2, ( #21425, #24446, #18587, #15542, #30129, #9477, #4161, #35994, #3406 ),
 .UNSPECIFIED., .F., .F. ) 
 B_SPLINE_CURVE_WITH_KNOTS ( ( 3, 2, 2, 2, 3 ),
 ( 0.5543478260869565410, 0.5579710144927536586, 0.5652173913043477826, 0.5724637681159420177, 0.5760869565217391353 ),
 .UNSPECIFIED. ) 
 CURVE ( )  GEOMETRIC_REPRESENTATION_ITEM ( )  RATIONAL_B_SPLINE_CURVE ( ( 0.9330127018922194093, 0.9330127018922194093, 1.000000000000000000, 0.8660254037844387076, 1.000000000000000000, 0.8660254037844387076, 1.000000000000000000, 0.9330127018922194093, 0.9330127018922194093 ) ) 
 REPRESENTATION_ITEM ( '' )  );
#36387 = FACE_OUTER_BOUND ( 'NONE', #31496, .T. ) ;
#36388 = CARTESIAN_POINT ( 'NONE',  ( 26.99999999999999645, 3.464101615137755275, -9.581249998770951848 ) ) ;
#36389 = CARTESIAN_POINT ( 'NONE',  ( 16.56230152254411081, -7.209453229046482114, -9.084374999385513405 ) ) ;
#36390 = EDGE_LOOP ( 'NONE', ( #11667, #25057, #15870, #3423 ) ) ;
#36391 = CARTESIAN_POINT ( 'NONE',  ( -1.909035429704832693E-15, 199.5500000012290513, -31.17691453623979214 ) ) ;
#36392 = CARTESIAN_POINT ( 'NONE',  ( -11.48171059495397373, 123.6851862821014549, -4.944772684328680334 ) ) ;
#36393 = CARTESIAN_POINT ( 'NONE',  ( 22.80587116629411071, -3.604726614523235284, -1.303124999385484095 ) ) ;
#36394 = CARTESIAN_POINT ( 'NONE',  ( 24.47653776615555898, 0.000000000000000000, 161.3739362214482469 ) ) ;
#36395 = CARTESIAN_POINT ( 'NONE',  ( -59.29836230271182984, 202.5810206699313767, -4.149950860017804111 ) ) ;
#36396 = CARTESIAN_POINT ( 'NONE',  ( 23.87821517812500005, 245.8468750006145171, 4.985214923628404016 ) ) ;
#36397 = CARTESIAN_POINT ( 'NONE',  ( 10.56230152254411081, 0.000000000000000000, -2.587499998771031429 ) ) ;
#36398 = CARTESIAN_POINT ( 'NONE',  ( -31.78794563604516910, 206.7903428501025758, 3.378800118222471838 ) ) ;
#36399 = CARTESIAN_POINT ( 'NONE',  ( -8.962234695871760692, 131.1601862821014777, 8.715434833791933400 ) ) ;
#36400 = CARTESIAN_POINT ( 'NONE',  ( 13.56230152254410548, 5.196152422706630247, -2.212499998771017218 ) ) ;
#36401 = ORIENTED_EDGE ( 'NONE', *, *, #13141, .F. ) ;
#36402 =( BOUNDED_CURVE ( )  B_SPLINE_CURVE ( 2, ( #32817, #20707, #35658, #23734, #32250, #12735, #15395, #3255, #4008 ),
 .UNSPECIFIED., .F., .F. ) 
 B_SPLINE_CURVE_WITH_KNOTS ( ( 3, 2, 2, 2, 3 ),
 ( 0.1413043478260869457, 0.1449275362318840632, 0.1521739130434782705, 0.1594202898550724501, 0.1630434782608695676 ),
 .UNSPECIFIED. ) 
 CURVE ( )  GEOMETRIC_REPRESENTATION_ITEM ( )  RATIONAL_B_SPLINE_CURVE ( ( 0.9330127018922194093, 0.9330127018922190762, 1.000000000000000000, 0.8660254037844387076, 1.000000000000000000, 0.8660254037844387076, 1.000000000000000000, 0.9330127018922190762, 0.9330127018922194093 ) ) 
 REPRESENTATION_ITEM ( '' )  );
#36403 = FACE_OUTER_BOUND ( 'NONE', #35729, .T. ) ;
#36404 = FILL_AREA_STYLE_COLOUR ( '', #11735 ) ;
#36405 = CARTESIAN_POINT ( 'NONE',  ( 13.04141134922759804, 119.3726862821014265, 8.927990412390657937 ) ) ;
#36406 = CARTESIAN_POINT ( 'NONE',  ( 22.60769515458671108, 242.5388461906613600, 6.000000000000010658 ) ) ;
#36407 = CARTESIAN_POINT ( 'NONE',  ( -2.660918448318275509, 10.69768628210143646, 12.46528703574805874 ) ) ;
#36408 = CARTESIAN_POINT ( 'NONE',  ( 16.56230152254411436, -6.928203230275514990, -9.787500000000044054 ) ) ;
#36409 = ORIENTED_EDGE ( 'NONE', *, *, #30444, .T. ) ;
#36410 = CARTESIAN_POINT ( 'NONE',  ( 10.56230152254410726, 0.000000000000000000, -8.100000000000024514 ) ) ;
#36411 = CARTESIAN_POINT ( 'NONE',  ( 6.594114490232313663, 73.66018628210144925, 6.840914352312096547 ) ) ;
#36412 = SURFACE_STYLE_USAGE ( .BOTH. , #15409 ) ;
#36413 = CARTESIAN_POINT ( 'NONE',  ( -7.954856959092309943, 134.4273137178984996, 5.529263428287300108 ) ) ;
#36414 = CARTESIAN_POINT ( 'NONE',  ( 27.24356964374999635, 196.0156250006145626, -15.72908226750539029 ) ) ;
#36415 = CARTESIAN_POINT ( 'NONE',  ( 24.00000000000000000, -5.196152422706629359, -5.700000000000010836 ) ) ;
#36416 = CARTESIAN_POINT ( 'NONE',  ( 27.24356964374999635, 198.3218750006145399, -15.72908226750539029 ) ) ;
#36417 = CARTESIAN_POINT ( 'NONE',  ( -104.7527771047627994, 12.87393045632884636, -3.000000000000000000 ) ) ;
#36418 = CARTESIAN_POINT ( 'NONE',  ( 19.56230152254410726, 5.196152422706631135, -6.787499998771012955 ) ) ;
#36419 = CARTESIAN_POINT ( 'NONE',  ( -0.1745138560723084320, 54.78981371789855359, -9.500000000000005329 ) ) ;
#36420 = CYLINDRICAL_SURFACE ( 'NONE', #29055, 2.649999999999991029 ) ;
#36421 = VERTEX_POINT ( 'NONE', #29676 ) ;
#36422 = AXIS2_PLACEMENT_3D ( 'NONE', #1265, #20819, #3927 ) ;
#36423 = CARTESIAN_POINT ( 'NONE',  ( 21.00000000000000000, 241.3937500012290229, -6.928203230275506996 ) ) ;
#36424 = CARTESIAN_POINT ( 'NONE',  ( -10.69584247140429412, 53.35231371789856070, -6.932735513424201024 ) ) ;
#36425 = CARTESIAN_POINT ( 'NONE',  ( 10.31873187879410736, -3.604726614523244610, -6.459374999385468996 ) ) ;
#36426 = CARTESIAN_POINT ( 'NONE',  ( -27.24356964374999635, 198.4906250006145569, 15.72908226750539384 ) ) ;
#36427 = CARTESIAN_POINT ( 'NONE',  ( 21.00000000000000000, -6.646953231504538984, -7.340624999385477523 ) ) ;
#36428 = CARTESIAN_POINT ( 'NONE',  ( -10.49813415416004858, 24.02731371789855785, 7.228626920338839135 ) ) ;
#36429 = VERTEX_POINT ( 'NONE', #29866 ) ;
#36430 = CARTESIAN_POINT ( 'NONE',  ( 15.24356964375000167, -3.323476615752272600, -7.753124999385476279 ) ) ;
#36431 = CARTESIAN_POINT ( 'NONE',  ( 12.46528703574805874, 17.59768628210143859, 2.660918448318279950 ) ) ;
#36432 = EDGE_CURVE ( 'NONE', #14950, #34407, #24188, .T. ) ;
#36433 = CARTESIAN_POINT ( 'NONE',  ( 25.21845102629493951, 3.604726614523240613, 169.8540435889542550 ) ) ;
#36434 = CARTESIAN_POINT ( 'NONE',  ( -60.48586230271183695, 206.8500491399821328, 5.686928522499748340 ) ) ;
#36435 = SHAPE_REPRESENTATION_RELATIONSHIP ( 'NONE' , 'NONE' ,  #35512, #27327 ) ;
#36437 =( BOUNDED_CURVE ( )  B_SPLINE_CURVE ( 2, ( #8825, #20579, #3128, #23050, #29086, #34781, #34594 ),
 .UNSPECIFIED., .F., .F. ) 
 B_SPLINE_CURVE_WITH_KNOTS ( ( 3, 2, 2, 3 ),
 ( 0.8260869565217369148, 0.8333333333333312609, 0.8405797101449254960, 0.8478260869565198421 ),
 .UNSPECIFIED. ) 
 CURVE ( )  GEOMETRIC_REPRESENTATION_ITEM ( )  RATIONAL_B_SPLINE_CURVE ( ( 1.000000000000041078, 0.8660254037843976294, 1.000000000000000000, 0.8660254037844387076, 1.000000000000000000, 0.8660254037844735686, 0.9999999999999651390 ) ) 
 REPRESENTATION_ITEM ( '' )  );
#36436 = AXIS2_PLACEMENT_3D ( 'NONE', #2850, #37164, #11390 ) ;
#36438 = DIRECTION ( 'NONE',  ( 1.000000000000000000, 0.000000000000000000, 0.000000000000000000 ) ) ;
#36439 = CARTESIAN_POINT ( 'NONE',  ( -2.660918448318004614, 63.70231371789855501, -12.46528703574811558 ) ) ;
#36440 = CARTESIAN_POINT ( 'NONE',  ( -32.78497103062156981, 206.1606490808709111, -2.350049139982163027 ) ) ;
#36441 = CARTESIAN_POINT ( 'NONE',  ( -55.34747103062156981, 213.3500491399821328, -5.571401726697985168 ) ) ;
#36442 = CARTESIAN_POINT ( 'NONE',  ( 10.56230152254410903, 0.000000000000000000, -1.687499998771019305 ) ) ;
#36443 = CARTESIAN_POINT ( 'NONE',  ( 33.80341017455227615, -5.196152422706629359, 161.9225082118381920 ) ) ;
#36444 = CARTESIAN_POINT ( 'NONE',  ( -5.770363421894122880, 32.36481371789854933, 14.38691631536194393 ) ) ;
#36445 = CARTESIAN_POINT ( 'NONE',  ( -50.98586230271183695, 205.8500491399821613, 7.418979330068642852 ) ) ;
#36446 = DIRECTION ( 'NONE',  ( -0.000000000000000000, 1.000000000000000000, -0.000000000000000000 ) ) ;
#36447 = CARTESIAN_POINT ( 'NONE',  ( 10.69584247140445221, 71.64768628210146062, -6.932735513423970097 ) ) ;
#36448 = CARTESIAN_POINT ( 'NONE',  ( 15.50000000000000533, 17.31018628210144428, 0.1745138560725827404 ) ) ;
#36449 = ADVANCED_FACE ( 'NONE', ( #3900 ), #35733, .T. ) ;
#36450 = CARTESIAN_POINT ( 'NONE',  ( 22.56230152254412147, -3.464101615137755275, -1.162500000000034284 ) ) ;
#36451 = CARTESIAN_POINT ( 'NONE',  ( 15.00000000000000178, 244.2437500012290457, 3.464101615137757051 ) ) ;
#36452 = ORIENTED_EDGE ( 'NONE', *, *, #8477, .F. ) ;
#36453 = CARTESIAN_POINT ( 'NONE',  ( 8.632099005475504683, 27.94768628210144001, 13.23911966647218996 ) ) ;
#36454 = CARTESIAN_POINT ( 'NONE',  ( -13.49999999999998401, 196.1375000012290286, 23.38268590217985476 ) ) ;
#36455 = CARTESIAN_POINT ( 'NONE',  ( 5.778771075727756162E-15, 197.7218750006145456, 31.45816453501075927 ) ) ;
#36456 = CARTESIAN_POINT ( 'NONE',  ( -29.00000000000002487, 210.0000000000000000, 0.000000000000000000 ) ) ;
#36457 = CARTESIAN_POINT ( 'NONE',  ( 1.120210788295102201E-13, 195.5000000012290400, -27.00000000000000711 ) ) ;
#36458 = EDGE_CURVE ( 'NONE', #22517, #14644, #4751, .T. ) ;
#36459 = CARTESIAN_POINT ( 'NONE',  ( 10.49813415415989581, 8.972686282101431487, 7.228626920339068285 ) ) ;
#36460 = CARTESIAN_POINT ( 'NONE',  ( 18.12178482187500350, 247.6843750006145228, 4.985214923628407568 ) ) ;
#36461 = CARTESIAN_POINT ( 'NONE',  ( -9.465287035748106703, 116.6023137178985394, 2.064181346179061460 ) ) ;
#36462 = CARTESIAN_POINT ( 'NONE',  ( 26.75643035624999655, 243.7843750006145456, -7.049594010296217766E-16 ) ) ;
#36463 = ORIENTED_EDGE ( 'NONE', *, *, #12493, .T. ) ;
#36464 = CARTESIAN_POINT ( 'NONE',  ( 26.97716818855048260, 0.000000000000000000, 49.47706554351410801 ) ) ;
#36465 = CARTESIAN_POINT ( 'NONE',  ( 22.56230152254411792, 7.347880794884125653E-16, -2.025000000000027001 ) ) ;
#36466 = CARTESIAN_POINT ( 'NONE',  ( -60.72871937935236986, 215.3268752544371978, 7.500000000000000000 ) ) ;
#36467 = CARTESIAN_POINT ( 'NONE',  ( 22.80587116629411071, -3.604726614523235284, -9.403124999385536142 ) ) ;
#36468 = CARTESIAN_POINT ( 'NONE',  ( 27.79398286670857132, -5.407089921784859143, 163.4740433714303265 ) ) ;
#36469 = FACE_OUTER_BOUND ( 'NONE', #31507, .T. ) ;
#36470 = CARTESIAN_POINT ( 'NONE',  ( 13.50000000000001421, 197.0000000000000000, 23.38268590217984055 ) ) ;
#36471 = AXIS2_PLACEMENT_3D ( 'NONE', #27618, #30472, #21386 ) ;
#36472 = EDGE_LOOP ( 'NONE', ( #5145, #13021, #24606 ) ) ;
#36473 = CARTESIAN_POINT ( 'NONE',  ( 7.228626920339069173, 34.27268628210144641, -10.49813415415989404 ) ) ;
#36474 = EDGE_LOOP ( 'NONE', ( #19729, #18974, #36409, #6943 ) ) ;
#36475 = ORIENTED_EDGE ( 'NONE', *, *, #5656, .F. ) ;
#36476 = CARTESIAN_POINT ( 'NONE',  ( 24.00000000000000000, -5.196152422706629359, -3.843749998770962240 ) ) ;
#36477 = CARTESIAN_POINT ( 'NONE',  ( 26.75643035624999655, 7.049594010296217766E-16, -0.3656249993854721048 ) ) ;
#36478 = CARTESIAN_POINT ( 'NONE',  ( -13.50000000000000533, 199.1375000012290286, -23.38268590217984411 ) ) ;
#36479 = CARTESIAN_POINT ( 'NONE',  ( 20.99999999999999645, 6.928203230275506996, -5.962500000000000355 ) ) ;
#36480 = CARTESIAN_POINT ( 'NONE',  ( 26.75643035624999655, 249.5593750006145228, -3.323476615752271712 ) ) ;
#36481 = CARTESIAN_POINT ( 'NONE',  ( -6.932735513423968321, 69.34768628210143504, -10.69584247140445221 ) ) ;
#36482 = CARTESIAN_POINT ( 'NONE',  ( -15.53471296425195369, 141.2226862821014493, 2.908627838312118019 ) ) ;
#36483 = CARTESIAN_POINT ( 'NONE',  ( -67.61086230271183695, 213.1499508600178387, -5.686928522499747451 ) ) ;
#36484 = CARTESIAN_POINT ( 'NONE',  ( 5.536961926790850086, 215.7986392774537308, -1.553813268097582245 ) ) ;
#36485 = CARTESIAN_POINT ( 'NONE',  ( -54.54836230271183695, 206.0451222850691977, -2.149950860017851184 ) ) ;
#36486 = CARTESIAN_POINT ( 'NONE',  ( 20.99999999999999645, 185.0294372515228645, 0.000000000000000000 ) ) ;
#36487 = CARTESIAN_POINT ( 'NONE',  ( 31.08609832957909092, -6.928203230275506996, 165.2846314378917043 ) ) ;
#36488 = CARTESIAN_POINT ( 'NONE',  ( -11.48171059495408208, 116.3148137178985593, 4.944772684328421875 ) ) ;
#36489 = EDGE_CURVE ( 'NONE', #35077, #28874, #36734, .T. ) ;
#36490 = CARTESIAN_POINT ( 'NONE',  ( -46.63913769728824121, 206.8500491399821044, -5.686928522499717253 ) ) ;
#36491 = CARTESIAN_POINT ( 'NONE',  ( -61.68080436395489841, 201.5000000000000000, -0.1155267958017054536 ) ) ;
#36492 = CARTESIAN_POINT ( 'NONE',  ( 26.75643035624999655, 3.323476615752271268, -1.790624999385477256 ) ) ;
#36493 = CARTESIAN_POINT ( 'NONE',  ( 5.778771075727756162E-15, 195.4156250006145399, 31.45816453501075927 ) ) ;
#36494 = CARTESIAN_POINT ( 'NONE',  ( -6.092822981423666739, 91.01481371789856212, -14.25334919248795096 ) ) ;
#36495 = CARTESIAN_POINT ( 'NONE',  ( -42.67336230271183695, 215.6869285224997270, 3.149950860017831200 ) ) ;
#36496 = EDGE_CURVE ( 'NONE', #24223, #14024, #33096, .T. ) ;
#36497 = ORIENTED_EDGE ( 'NONE', *, *, #23618, .T. ) ;
#36498 = CARTESIAN_POINT ( 'NONE',  ( 24.88995133726761111, 3.464101615137512358, 163.3046267141977808 ) ) ;
#36499 = CARTESIAN_POINT ( 'NONE',  ( 6.932735513423970097, 119.9476862821014578, 10.69584247140445044 ) ) ;
#36500 = CARTESIAN_POINT ( 'NONE',  ( -8.632099005475501130, 60.14768628210144641, -13.23911966647218996 ) ) ;
#36501 = CARTESIAN_POINT ( 'NONE',  ( 34.22460179574976991, 5.407089921784862696, 165.3394263477420054 ) ) ;
#36502 = CARTESIAN_POINT ( 'NONE',  ( -8.927990412390661490, 94.07268628210144357, 13.04141134922759804 ) ) ;
#36503 = VECTOR ( 'NONE', #21875, 1000.000000000000000 ) ;
#36504 = CARTESIAN_POINT ( 'NONE',  ( -52.37872103062156270, 203.4690446883607535, 1.626142955000567936 ) ) ;
#36505 = EDGE_CURVE ( 'NONE', #15426, #12608, #30671, .T. ) ;
#36506 = CARTESIAN_POINT ( 'NONE',  ( 13.44051670066911086, 5.407089921784856479, -6.965624999385521932 ) ) ;
#36507 = CARTESIAN_POINT ( 'NONE',  ( 5.529263428287477744, 34.27268628210144641, -7.954856959092191815 ) ) ;
#36508 = CARTESIAN_POINT ( 'NONE',  ( 26.99999999999999645, 7.347880794884117764E-16, -2.868749998770958598 ) ) ;
#36509 = CARTESIAN_POINT ( 'NONE',  ( -61.08705436395488420, 205.3262412349647263, -4.842901733360204020 ) ) ;
#36510 = FACE_OUTER_BOUND ( 'NONE', #14090, .T. ) ;
#36511 = CARTESIAN_POINT ( 'NONE',  ( 10.69584247140445221, 53.24768628210144072, -6.932735513423970097 ) ) ;
#36512 = CARTESIAN_POINT ( 'NONE',  ( -27.00000000000000355, 199.5500000000000114, 0.000000000000000000 ) ) ;
#36513 = CARTESIAN_POINT ( 'NONE',  ( 16.56230152254411792, 6.928203230275514990, -6.862500000000054889 ) ) ;
#36515 = CARTESIAN_POINT ( 'NONE',  ( 16.56230152254412147, -7.209453229046482114, -0.9843749993855260838 ) ) ;
#36514 = CARTESIAN_POINT ( 'NONE',  ( 1.715153634034233487, 19.32268628210144001, 9.534712964251941258 ) ) ;
#36516 = DIRECTION ( 'NONE',  ( 1.000000000000000000, 0.000000000000000000, 0.000000000000000000 ) ) ;
#36517 = VERTEX_POINT ( 'NONE', #10521 ) ;
#36518 = CARTESIAN_POINT ( 'NONE',  ( 26.99999999999999645, -3.464101615137751278, -1.162500000000002309 ) ) ;
#36519 = CARTESIAN_POINT ( 'NONE',  ( 27.73678691053042300, 5.407089921784862696, 162.8202906008076241 ) ) ;
#36520 = CARTESIAN_POINT ( 'NONE',  ( 36.67106567565804198, 7.347880794884125653E-16, 160.2788208387686097 ) ) ;
#36521 = CARTESIAN_POINT ( 'NONE',  ( 26.99999999999999645, 242.9874999999999829, 3.464101615137751278 ) ) ;
#36522 = PLANE ( 'NONE',  #31200 ) ;
#36523 = EDGE_CURVE ( 'NONE', #14391, #13208, #30440, .T. ) ;
#36524 = CARTESIAN_POINT ( 'NONE',  ( -2.660918448318004614, 91.30231371789857064, -12.46528703574811558 ) ) ;
#36525 = CARTESIAN_POINT ( 'NONE',  ( -8.715434833791929847, 87.46018628210144641, -8.962234695871762469 ) ) ;
#36526 = ORIENTED_EDGE ( 'NONE', *, *, #14680, .F. ) ;
#36527 = VERTEX_POINT ( 'NONE', #7687 ) ;
#36528 = CARTESIAN_POINT ( 'NONE',  ( -13.50000000000000533, 197.3375000012290457, -23.38268590217984411 ) ) ;
#36529 = CARTESIAN_POINT ( 'NONE',  ( -27.00000000000000355, 196.8500000000000227, 0.000000000000000000 ) ) ;
#36530 = CARTESIAN_POINT ( 'NONE',  ( 10.83675517735179206, 55.93981371789855217, -11.08355503943118769 ) ) ;
#36531 = CARTESIAN_POINT ( 'NONE',  ( 18.12178482187500350, -4.985214923628407568, -9.628124999385478944 ) ) ;
#36532 = CARTESIAN_POINT ( 'NONE',  ( 23.87821517812499650, 243.4093750006145171, -4.985214923628404904 ) ) ;
#36533 = AXIS2_PLACEMENT_3D ( 'NONE', #17500, #2527, #2889 ) ;
#36534 = CARTESIAN_POINT ( 'NONE',  ( -60.29538769728823411, 211.3212981617418222, -4.469044688360751749 ) ) ;
#36535 = LINE ( 'NONE', #30682, #2228 ) ;
#36536 = EDGE_CURVE ( 'NONE', #4926, #1851, #19268, .T. ) ;
#36537 = CARTESIAN_POINT ( 'NONE',  ( 9.465287035748106703, 38.40231371789853654, -2.064181346179063237 ) ) ;
#36538 = CARTESIAN_POINT ( 'NONE',  ( 13.44051670066911086, 5.407089921784856479, -6.965624999385521932 ) ) ;
#36539 = CARTESIAN_POINT ( 'NONE',  ( -6.840914352311947333, 90.43981371789854506, -6.594114490232462877 ) ) ;
#36540 = CARTESIAN_POINT ( 'NONE',  ( 13.62178482187501416, 199.5593750006145513, 23.59362340125806767 ) ) ;
#36541 = CARTESIAN_POINT ( 'NONE',  ( 2.311890736173452865, 9.077313717898549683, -12.53471296425189152 ) ) ;
#36542 = CARTESIAN_POINT ( 'NONE',  ( -7.228626920339069173, 57.27268628210144641, 10.49813415415989581 ) ) ;
#36543 = CARTESIAN_POINT ( 'NONE',  ( 22.56230152254411436, -3.464101615137751278, -7.799999998771014020 ) ) ;
#36544 = AXIS2_PLACEMENT_3D ( 'NONE', #37478, #21015, #11529 ) ;
#36545 = CARTESIAN_POINT ( 'NONE',  ( 26.99999999999999645, 7.347880794884117764E-16, -1.968749998770946696 ) ) ;
#36546 = CARTESIAN_POINT ( 'NONE',  ( 27.75476278247212747, -5.407089921784859143, 163.0257557572890335 ) ) ;
#36547 = EDGE_CURVE ( 'NONE', #5600, #1101, #27782, .T. ) ;
#36548 = CARTESIAN_POINT ( 'NONE',  ( 10.31873187879411091, -3.604726614523244610, -5.559374999385509497 ) ) ;
#36549 =( NAMED_UNIT ( * ) SI_UNIT ( $, .STERADIAN. ) SOLID_ANGLE_UNIT ( ) );
#36550 = CARTESIAN_POINT ( 'NONE',  ( 1.120210788295102201E-13, 195.5000000012290400, -27.00000000000000711 ) ) ;
#36551 = CARTESIAN_POINT ( 'NONE',  ( 8.152565276336714462, 90.04768628210145209, -5.233372021372432847 ) ) ;
#36552 = CARTESIAN_POINT ( 'NONE',  ( 15.00000000000000000, 0.000000000000000000, -7.593749998770965348 ) ) ;
#36553 = CARTESIAN_POINT ( 'NONE',  ( 12.50000000000000355, 118.5101862821014578, 0.1745138560725507937 ) ) ;
#36554 = CARTESIAN_POINT ( 'NONE',  ( -6.392720816132698936, 142.9999999999999147, 10.60379120543304055 ) ) ;
#36555 = CARTESIAN_POINT ( 'NONE',  ( 0.000000000000000000, 200.0000000000000000, 0.000000000000000000 ) ) ;
#36556 = VERTEX_POINT ( 'NONE', #27957 ) ;
#36557 = CARTESIAN_POINT ( 'NONE',  ( 34.05955060792140188, -5.407089921784855591, 163.4528826382307614 ) ) ;
#36558 = CARTESIAN_POINT ( 'NONE',  ( 26.75643035624999655, -3.323476615752267715, -5.803124999385441463 ) ) ;
#36559 = CARTESIAN_POINT ( 'NONE',  ( 13.62178482187499640, 198.3593750006145342, -23.59362340125807123 ) ) ;
#36560 = CARTESIAN_POINT ( 'NONE',  ( -47.00000000000000711, 244.5000000000000000, 5.000000000000000000 ) ) ;
#36561 = CARTESIAN_POINT ( 'NONE',  ( 34.30346624845981296, -5.196152422706635576, 167.6381752909151999 ) ) ;
#36562 = DIRECTION ( 'NONE',  ( 1.000000000000000000, 0.000000000000000000, 0.000000000000000000 ) ) ;
#36563 = CARTESIAN_POINT ( 'NONE',  ( 15.24356964374999990, 242.6218750006145228, -3.323476615752268604 ) ) ;
#36564 = DIRECTION ( 'NONE',  ( -0.000000000000000000, 1.000000000000000000, -0.000000000000000000 ) ) ;
#36565 = CARTESIAN_POINT ( 'NONE',  ( 7.954856959092311719, 10.22731371789853405, -5.529263428287300108 ) ) ;
#36566 = CARTESIAN_POINT ( 'NONE',  ( -13.62178482187498396, 195.8843750006145399, 23.59362340125808188 ) ) ;
#36568 = VERTEX_POINT ( 'NONE', #24742 ) ;
#36567 = ORIENTED_EDGE ( 'NONE', *, *, #36523, .T. ) ;
#36569 = EDGE_CURVE ( 'NONE', #19865, #21112, #24749, .T. ) ;
#36570 = CARTESIAN_POINT ( 'NONE',  ( 15.24356964375000167, 244.8343750006145285, 3.323476615752272600 ) ) ;
#36571 = CARTESIAN_POINT ( 'NONE',  ( -2.311890736173447980, 13.67731371789854222, 12.53471296425189330 ) ) ;
#36572 = CIRCLE ( 'NONE', #16625, 7.500000000000000000 ) ;
#36573 = CARTESIAN_POINT ( 'NONE',  ( 23.87821517812499650, 4.985214923628404904, -2.990624999385460558 ) ) ;
#36574 = CARTESIAN_POINT ( 'NONE',  ( -14.38691631536193860, 117.4648137178985650, -5.770363421894132649 ) ) ;
#36575 = ADVANCED_FACE ( 'NONE', ( #7135 ), #1988, .T. ) ;
#36576 = DIRECTION ( 'NONE',  ( 0.000000000000000000, 0.000000000000000000, -1.000000000000000000 ) ) ;
#36577 = CARTESIAN_POINT ( 'NONE',  ( 15.00000000000000000, 0.000000000000000000, -10.29374999877094510 ) ) ;
#36578 = CARTESIAN_POINT ( 'NONE',  ( 16.56230152254411792, 7.209453229046482114, -8.859374999385531524 ) ) ;
#36579 = ORIENTED_EDGE ( 'NONE', *, *, #11717, .F. ) ;
#36580 = CARTESIAN_POINT ( 'NONE',  ( -13.49999999999998401, 198.8375000012290457, 23.38268590217985476 ) ) ;
#36581 = CARTESIAN_POINT ( 'NONE',  ( 12.50000000000000355, 109.3101862821014549, 0.1745138560725507937 ) ) ;
#36582 = CARTESIAN_POINT ( 'NONE',  ( 16.56230152254411436, -7.209453229046475009, -0.4781249993855187230 ) ) ;
#36583 = EDGE_CURVE ( 'NONE', #2189, #18678, #13560, .T. ) ;
#36584 = CARTESIAN_POINT ( 'NONE',  ( -47.81919563604517265, 218.5000000000000000, -0.1155267958018185298 ) ) ;
#36585 = CARTESIAN_POINT ( 'NONE',  ( 23.87821517812499650, 243.2968750006145058, -4.985214923628404904 ) ) ;
#36586 =( NAMED_UNIT ( * ) SI_UNIT ( $, .STERADIAN. ) SOLID_ANGLE_UNIT ( ) );
#36587 = CARTESIAN_POINT ( 'NONE',  ( -13.50000000000000533, 197.3375000012290457, -23.38268590217984411 ) ) ;
#36588 = CARTESIAN_POINT ( 'NONE',  ( -64.84002896937850835, 204.4285982733020433, 3.350049139982171020 ) ) ;
#36589 = CARTESIAN_POINT ( 'NONE',  ( -0.1745138560725500443, 130.0101862821014436, 12.50000000000000355 ) ) ;
#36590 = CARTESIAN_POINT ( 'NONE',  ( 22.56230152254410370, -3.464101615137751278, -0.5999999987710181726 ) ) ;
#36591 = ORIENTED_EDGE ( 'NONE', *, *, #414, .T. ) ;
#36592 = CARTESIAN_POINT ( 'NONE',  ( 10.56230152254410903, 7.347880794884117764E-16, -10.00000000000000000 ) ) ;
#36593 = CARTESIAN_POINT ( 'NONE',  ( -13.49999999999998401, 199.6250000000000284, 23.38268590217985476 ) ) ;
#36594 = CARTESIAN_POINT ( 'NONE',  ( 6.092822981423978490, 125.9851862821014521, -14.25334919248782306 ) ) ;
#36595 = CARTESIAN_POINT ( 'NONE',  ( 0.000000000000000000, 200.0000000000000000, 0.000000000000000000 ) ) ;
#36596 = CARTESIAN_POINT ( 'NONE',  ( -12.46528703574805697, 3.797686282101447652, -2.660918448318280838 ) ) ;
#36597 = CARTESIAN_POINT ( 'NONE',  ( 14.47852554861151830, 5.725134610794655465, -9.986452800325864132 ) ) ;
#36598 = ORIENTED_EDGE ( 'NONE', *, *, #10299, .T. ) ;
#36599 = CYLINDRICAL_SURFACE ( 'NONE', #3400, 8.000000000000000000 ) ;
#36600 = CARTESIAN_POINT ( 'NONE',  ( -9.500000000000005329, 86.31018628210145494, -0.1745138560725176813 ) ) ;
#36601 = CARTESIAN_POINT ( 'NONE',  ( 9.500000000000005329, 130.6898137178985451, -0.1745138560723090149 ) ) ;
#36602 = CARTESIAN_POINT ( 'NONE',  ( 5.778771075727756162E-15, 195.4156250006145399, 31.45816453501075927 ) ) ;
#36604 = CYLINDRICAL_SURFACE ( 'NONE', #33513, 6.000000000000001776 ) ;
#36603 =( BOUNDED_CURVE ( )  B_SPLINE_CURVE ( 2, ( #35377, #34820, #8863, #20624, #21005, #9053, #29510, #17776, #6394 ),
 .UNSPECIFIED., .F., .F. ) 
 B_SPLINE_CURVE_WITH_KNOTS ( ( 3, 2, 2, 2, 3 ),
 ( 0.1875000000000000000, 0.1944444444444444475, 0.2083333333333333426, 0.2222222222222222099, 0.2291666666666666574 ),
 .UNSPECIFIED. ) 
 CURVE ( )  GEOMETRIC_REPRESENTATION_ITEM ( )  RATIONAL_B_SPLINE_CURVE ( ( 0.9330127018922194093, 0.9330127018922194093, 1.000000000000000000, 0.8660254037844387076, 1.000000000000000000, 0.8660254037844387076, 1.000000000000000000, 0.9330127018922194093, 0.9330127018922194093 ) ) 
 REPRESENTATION_ITEM ( '' )  );
#36605 = CARTESIAN_POINT ( 'NONE',  ( -13.62178482187498396, 199.0343750006145456, 23.59362340125808188 ) ) ;
#36606 = DIRECTION ( 'NONE',  ( -0.2588190451025212391, 0.000000000000000000, -0.9659258262890682012 ) ) ;
#36607 = CARTESIAN_POINT ( 'NONE',  ( 21.00000000000000000, 243.8125000000000284, 5.999999999999998224 ) ) ;
#36608 = CARTESIAN_POINT ( 'NONE',  ( -9.500000000000005329, 61.68981371789855928, 0.1745138560723101806 ) ) ;
#36609 = DIRECTION ( 'NONE',  ( 0.000000000000000000, 0.000000000000000000, -1.000000000000000000 ) ) ;
#36610 = ORIENTED_EDGE ( 'NONE', *, *, #13192, .T. ) ;
#36611 = CARTESIAN_POINT ( 'NONE',  ( 15.00000000000000000, 241.0187500012290513, -3.464101615137752166 ) ) ;
#36612 = CARTESIAN_POINT ( 'NONE',  ( 11.48171059495408208, 65.71481371789855075, -4.944772684328420986 ) ) ;
#36613 = CARTESIAN_POINT ( 'NONE',  ( 19.68408634441911431, 5.407089921784862696, -5.296874999385526195 ) ) ;
#36614 = CARTESIAN_POINT ( 'NONE',  ( -27.24356964374999990, 197.9656250006145228, -15.72908226750537786 ) ) ;
#36615 = CARTESIAN_POINT ( 'NONE',  ( 21.00000000000000000, -6.646953231504538984, -6.890624999385480898 ) ) ;
#36616 = CARTESIAN_POINT ( 'NONE',  ( 4.944772684328420986, 31.21481371789855430, 11.48171059495408208 ) ) ;
#36617 = ORIENTED_EDGE ( 'NONE', *, *, #88, .T. ) ;
#36618 = UNCERTAINTY_MEASURE_WITH_UNIT (LENGTH_MEASURE( 1.000000000000000082E-05 ), #6136, 'distance_accuracy_value', 'NONE');
#36619 = CARTESIAN_POINT ( 'NONE',  ( 22.80587116629411781, 3.604726614523243278, -0.3843749993855423708 ) ) ;
#36620 = CARTESIAN_POINT ( 'NONE',  ( 4.622313124798573369, 9.835186282101449962, 11.61527771782819940 ) ) ;
#36621 = CARTESIAN_POINT ( 'NONE',  ( 28.29894145125277660, -5.407089921784865361, 169.2457464034993961 ) ) ;
#36622 = CIRCLE ( 'NONE', #22743, 8.000000000000000000 ) ;
#36623 =( BOUNDED_CURVE ( )  B_SPLINE_CURVE ( 3, ( #2658, #33949, #14175, #31784 ),
 .UNSPECIFIED., .F., .F. ) 
 B_SPLINE_CURVE_WITH_KNOTS ( ( 4, 4 ),
 ( 0.000000000000000000, 1.570796326794856812 ),
 .UNSPECIFIED. ) 
 CURVE ( )  GEOMETRIC_REPRESENTATION_ITEM ( )  RATIONAL_B_SPLINE_CURVE ( ( 1.000000000000000000, 0.8047378541243743744, 0.8047378541243743744, 1.000000000000000000 ) ) 
 REPRESENTATION_ITEM ( '' )  );
#36624 = PRODUCT_RELATED_PRODUCT_CATEGORY ( 'part', '', ( #17435 ) ) ;
#36625 = CARTESIAN_POINT ( 'NONE',  ( -47.62127896937847993, 216.5309553116391612, 1.626142955000506873 ) ) ;
#36626 = SURFACE_STYLE_USAGE ( .BOTH. , #20747 ) ;
#36627 = CARTESIAN_POINT ( 'NONE',  ( -12.46528703574811558, 61.40231371789855785, 2.660918448318003726 ) ) ;
#36628 = CARTESIAN_POINT ( 'NONE',  ( -65.43377896937850835, 208.9097554298617183, 4.530955311639234040 ) ) ;
#36629 = CARTESIAN_POINT ( 'NONE',  ( -61.08705436395488420, 205.3262412349647263, -4.842901733360204020 ) ) ;
#36630 = EDGE_CURVE ( 'NONE', #9264, #28127, #28142, .T. ) ;
#36631 = CARTESIAN_POINT ( 'NONE',  ( -70.80918835584510873, 215.2843023367891249, -2.999999999999999112 ) ) ;
#36632 = CARTESIAN_POINT ( 'NONE',  ( 10.49999999999999645, 252.0000000000000000, 5.000000000000000000 ) ) ;
#36633 = CARTESIAN_POINT ( 'NONE',  ( -13.23911966647199812, 44.15231371789854364, -8.632099005475788900 ) ) ;
#36634 = CARTESIAN_POINT ( 'NONE',  ( -39.30877896937850124, 212.1620413398627534, -8.530955311639255356 ) ) ;
#36635 = CARTESIAN_POINT ( 'NONE',  ( 0.1745138560725515708, 24.21018628210144641, -12.50000000000000355 ) ) ;
#36636 = CARTESIAN_POINT ( 'NONE',  ( 14.99999999999972466, -3.464101615137598067, -0.4125000000000021982 ) ) ;
#36637 = CARTESIAN_POINT ( 'NONE',  ( -12.46528703574805697, 58.99768628210144783, -2.660918448318280838 ) ) ;
#36638 = CARTESIAN_POINT ( 'NONE',  ( 14.25334919248782661, 8.685186282101437172, 6.092822981423971385 ) ) ;
#36639 = CARTESIAN_POINT ( 'NONE',  ( 19.56230152254411792, 5.196152422706637353, -2.400000000000013234 ) ) ;
#36640 = CARTESIAN_POINT ( 'NONE',  ( -28.09666271755782674, 206.4427866876137045, -7.184768031510477826 ) ) ;
#36641 = VERTEX_POINT ( 'NONE', #9964 ) ;
#36642 = CARTESIAN_POINT ( 'NONE',  ( -11.08355503943142573, 39.16018628210144215, 10.83675517735155402 ) ) ;
#36643 = CIRCLE ( 'NONE', #10027, 7.500000000000000000 ) ;
#36644 = CARTESIAN_POINT ( 'NONE',  ( -7.234628195640316228, 195.9700961906613372, -27.00000000000000000 ) ) ;
#36645 = CARTESIAN_POINT ( 'NONE',  ( 27.24356964375000700, 197.7968750006145342, 15.72908226750537075 ) ) ;
#36646 = FACE_OUTER_BOUND ( 'NONE', #16582, .T. ) ;
#36647 = FILL_AREA_STYLE ('',( #33994 ) ) ;
#36648 = CARTESIAN_POINT ( 'NONE',  ( 37.25936693920468201, 7.347880794884125653E-16, 167.0031350508878631 ) ) ;
#36649 = CARTESIAN_POINT ( 'NONE',  ( -8.962234695871760692, 11.56018628210145316, 8.715434833791933400 ) ) ;
#36650 = AXIS2_PLACEMENT_3D ( 'NONE', #25417, #31294, #22588 ) ;
#36651 = CARTESIAN_POINT ( 'NONE',  ( 15.24356964374999990, 248.0593750006145228, 0.000000000000000000 ) ) ;
#36652 = CARTESIAN_POINT ( 'NONE',  ( 8.710071997420211432, 120.9148137178985678, -3.796722387233181895 ) ) ;
#36653 = CARTESIAN_POINT ( 'NONE',  ( 15.24356964374999990, 241.2718750006145001, -3.323476615752268604 ) ) ;
#36654 = ORIENTED_EDGE ( 'NONE', *, *, #13623, .T. ) ;
#36655 = CARTESIAN_POINT ( 'NONE',  ( -63.06622103062156981, 211.6261429550005744, 6.530955311639227823 ) ) ;
#36656 =( NAMED_UNIT ( * ) PLANE_ANGLE_UNIT ( ) SI_UNIT ( $, .RADIAN. ) );
#36657 = FACE_OUTER_BOUND ( 'NONE', #31929, .T. ) ;
#36658 = CARTESIAN_POINT ( 'NONE',  ( 4.944772684328420986, 114.0148137178985621, 11.48171059495408208 ) ) ;
#36659 = CARTESIAN_POINT ( 'NONE',  ( 19.68408634441910721, -5.407089921784855591, -8.990624999385548932 ) ) ;
#36660 = CARTESIAN_POINT ( 'NONE',  ( 33.87652354815133293, 5.407089921784857367, 161.3608737722381079 ) ) ;
#36661 = CARTESIAN_POINT ( 'NONE',  ( 23.99999999999999645, 240.9062500012290684, -5.196152422706631135 ) ) ;
#36662 = CARTESIAN_POINT ( 'NONE',  ( 5.727106289114498080E-15, 198.3125000000000000, 31.17691453623979214 ) ) ;
#36663 = ORIENTED_EDGE ( 'NONE', *, *, #19096, .F. ) ;
#36664 = CARTESIAN_POINT ( 'NONE',  ( 10.69584247140445221, 25.64768628210144286, -6.932735513423970097 ) ) ;
#36665 = ORIENTED_EDGE ( 'NONE', *, *, #6720, .T. ) ;
#36666 = ORIENTED_EDGE ( 'NONE', *, *, #15755, .F. ) ;
#36667 = CARTESIAN_POINT ( 'NONE',  ( 26.99999999999999645, 7.347880794884117764E-16, -5.118749998770960374 ) ) ;
#36668 = CARTESIAN_POINT ( 'NONE',  ( 18.12178482187499640, 4.985214923628404904, -2.015624999385456917 ) ) ;
#36669 = CARTESIAN_POINT ( 'NONE',  ( 20.99999999999999289, 249.4937500012290457, -5.999999999999998224 ) ) ;
#36670 =( BOUNDED_CURVE ( )  B_SPLINE_CURVE ( 2, ( #15508, #32932, #6984, #18553, #25336, #24593, #10930 ),
 .UNSPECIFIED., .F., .F. ) 
 B_SPLINE_CURVE_WITH_KNOTS ( ( 3, 2, 2, 3 ),
 ( 0.1739130434782605317, 0.1811594202898539063, 0.1884057971014473087, 0.1956521739130406834 ),
 .UNSPECIFIED. ) 
 CURVE ( )  GEOMETRIC_REPRESENTATION_ITEM ( )  RATIONAL_B_SPLINE_CURVE ( ( 1.000000000000006217, 0.8660254037844326014, 1.000000000000000000, 0.8660254037844387076, 1.000000000000000000, 0.8660254037844905550, 0.9999999999999481526 ) ) 
 REPRESENTATION_ITEM ( '' )  );
#36671 = CARTESIAN_POINT ( 'NONE',  ( 21.00000000000000355, 0.000000000000000000, 50.00000000000001421 ) ) ;
#36672 = CARTESIAN_POINT ( 'NONE',  ( 15.24356964374999990, 248.8093750006144944, -3.323476615752268604 ) ) ;
#36673 = CARTESIAN_POINT ( 'NONE',  ( -4.622313124798576922, 51.23518628210143788, -11.61527771782819762 ) ) ;
#36674 = CARTESIAN_POINT ( 'NONE',  ( -10.83675517735155047, 133.4601862821014606, -11.08355503943142750 ) ) ;
#36675 = CARTESIAN_POINT ( 'NONE',  ( -59.10044563604517265, 205.1570982666397072, -4.673758765035155527 ) ) ;
#36676 = CARTESIAN_POINT ( 'NONE',  ( 14.06542688029398036, 216.9345731196990243, -0.01200585064250309433 ) ) ;
#36677 = CARTESIAN_POINT ( 'NONE',  ( -52.37127896937850835, 214.5309553116392749, 1.090244570138288127 ) ) ;
#36678 = CYLINDRICAL_SURFACE ( 'NONE', #22662, 5.999999999999999112 ) ;
#36679 = CARTESIAN_POINT ( 'NONE',  ( 30.90960795051509891, 6.928203230275506996, 163.2673371742559141 ) ) ;
#36680 = CARTESIAN_POINT ( 'NONE',  ( 4.622313124798831829, 128.9648137178985507, -11.61527771782809282 ) ) ;
#36681 = CARTESIAN_POINT ( 'NONE',  ( -67.22247103062156270, 207.6499508600178387, 3.839350919129076445 ) ) ;
#36682 = CARTESIAN_POINT ( 'NONE',  ( -57.32663769728824121, 202.5810206699313767, 4.149950860017909804 ) ) ;
#36683 = CARTESIAN_POINT ( 'NONE',  ( 18.12178482187499640, 4.985214923628404904, -1.228124999385488136 ) ) ;
#36684 = CARTESIAN_POINT ( 'NONE',  ( -13.62178482187500528, 197.0281250006145228, -23.59362340125807123 ) ) ;
#36685 = CARTESIAN_POINT ( 'NONE',  ( -0.1745138560722442889, 100.7898137178985536, -15.50000000000000533 ) ) ;
#36686 = CARTESIAN_POINT ( 'NONE',  ( -34.95461230271183695, 208.1428034533959135, -6.469044688360754414 ) ) ;
#36687 = EDGE_LOOP ( 'NONE', ( #14875, #16508, #18699, #30883, #959 ) ) ;
#36688 = CARTESIAN_POINT ( 'NONE',  ( -13.50000000000000533, 195.9875000012290229, -23.38268590217984411 ) ) ;
#36689 = CARTESIAN_POINT ( 'NONE',  ( -4.622313124798576922, 124.8351862821014748, -11.61527771782819762 ) ) ;
#36690 = CARTESIAN_POINT ( 'NONE',  ( -13.23911966647218463, 67.04768628210143788, 8.632099005475506459 ) ) ;
#36691 = CARTESIAN_POINT ( 'NONE',  ( 21.00000000000016342, 4.000000000000002665, 50.00000000000000000 ) ) ;
#36692 = CARTESIAN_POINT ( 'NONE',  ( 24.83278686463658502, -3.604726614523244610, 165.4458820498982163 ) ) ;
#36693 = CARTESIAN_POINT ( 'NONE',  ( 6.092822981423978490, 79.98518628210145209, -14.25334919248782306 ) ) ;
#36694 = CARTESIAN_POINT ( 'NONE',  ( -44.06622103062156981, 211.6261429550005744, 6.530955311639228711 ) ) ;
#36695 = CARTESIAN_POINT ( 'NONE',  ( 10.31873187879410736, 0.000000000000000000, -6.440624999385525129 ) ) ;
#36696 = CARTESIAN_POINT ( 'NONE',  ( -6.594114490232312775, 13.86018628210145032, -6.840914352312096547 ) ) ;
#36697 = CARTESIAN_POINT ( 'NONE',  ( 15.00000000000010658, 3.464101615137812562, -2.681249998770963483 ) ) ;
#36698 = CARTESIAN_POINT ( 'NONE',  ( -68.80580436395490551, 216.5000000000000000, 0.1155267958017343610 ) ) ;
#36699 = EDGE_CURVE ( 'NONE', #6323, #9298, #33090, .T. ) ;
#36700 =( NAMED_UNIT ( * ) PLANE_ANGLE_UNIT ( ) SI_UNIT ( $, .RADIAN. ) );
#36701 = CARTESIAN_POINT ( 'NONE',  ( 8.715434833791931624, 64.46018628210146062, 8.962234695871760692 ) ) ;
#36702 = CARTESIAN_POINT ( 'NONE',  ( 26.99999999999999645, 198.9124999999999943, -15.58845726811990495 ) ) ;
#36703 = DIRECTION ( 'NONE',  ( -0.000000000000000000, 1.000000000000000000, -0.000000000000000000 ) ) ;
#36705 = CARTESIAN_POINT ( 'NONE',  ( 16.56230152254411436, 7.209453229046482114, -0.3093749993854842950 ) ) ;
#36704 = CARTESIAN_POINT ( 'NONE',  ( -9.465287035748065847, 22.19768628210144001, -2.064181346179273735 ) ) ;
#36706 = CARTESIAN_POINT ( 'NONE',  ( 1.069080835302379631E-14, 198.4250000012290229, 27.00000000000000000 ) ) ;
#36707 = ORIENTED_EDGE ( 'NONE', *, *, #32855, .T. ) ;
#36708 = CARTESIAN_POINT ( 'NONE',  ( 26.99999999999999645, -3.464101615137751278, -2.512499999999989075 ) ) ;
#36709 = LINE ( 'NONE', #10934, #23946 ) ;
#36710 = CARTESIAN_POINT ( 'NONE',  ( 27.54068648934820729, 5.407089921784862696, 160.5788525301012157 ) ) ;
#36711 = CARTESIAN_POINT ( 'NONE',  ( 10.31873187879411091, 0.000000000000000000, -1.940624999385548444 ) ) ;
#36712 = CARTESIAN_POINT ( 'NONE',  ( 30.60565229757555272, -6.928203230275514990, 159.7931081634365853 ) ) ;
#36713 = CARTESIAN_POINT ( 'NONE',  ( 24.00000000000000000, 244.7500000000000000, 5.196152422706629359 ) ) ;
#36714 = DIRECTION ( 'NONE',  ( 0.000000000000000000, 0.000000000000000000, -1.000000000000000000 ) ) ;
#36715 = CARTESIAN_POINT ( 'NONE',  ( -7.228626920338836470, 90.72731371789853938, -10.49813415416005213 ) ) ;
#36716 = CARTESIAN_POINT ( 'NONE',  ( -8.962234695871760692, 85.16018628210144925, 8.715434833791933400 ) ) ;
#36717 = ORIENTED_EDGE ( 'NONE', *, *, #10325, .F. ) ;
#36718 = ORIENTED_EDGE ( 'NONE', *, *, #2636, .F. ) ;
#36719 = CARTESIAN_POINT ( 'NONE',  ( 13.49999999999999645, 198.1625000012290343, -23.38268590217984766 ) ) ;
#36720 = CARTESIAN_POINT ( 'NONE',  ( 1.069080835302379631E-14, 196.9624999999999773, 27.00000000000000000 ) ) ;
#36721 = CARTESIAN_POINT ( 'NONE',  ( -15.50000000000000533, 52.48981371789855643, 0.1745138560722471477 ) ) ;
#36722 = CARTESIAN_POINT ( 'NONE',  ( 15.24356964375000167, -3.323476615752272600, -8.315624999385494931 ) ) ;
#36723 = CARTESIAN_POINT ( 'NONE',  ( 18.12178482187500350, 243.1843750006145513, 4.985214923628407568 ) ) ;
#36724 = CARTESIAN_POINT ( 'NONE',  ( -60.69122103062156981, 208.9097554298617752, -4.530955311639240257 ) ) ;
#36725 = ADVANCED_FACE ( 'NONE', ( #27396 ), #1427, .T. ) ;
#36726 = CARTESIAN_POINT ( 'NONE',  ( 25.47825260081467391, 3.464101615137757051, 170.0289409263170626 ) ) ;
#36727 = CARTESIAN_POINT ( 'NONE',  ( -9.465287035748106703, 33.80231371789854222, 2.064181346179061460 ) ) ;
#36728 = CARTESIAN_POINT ( 'NONE',  ( 16.56230152254410726, 7.209453229046475009, -9.253124999385514471 ) ) ;
#36729 = CARTESIAN_POINT ( 'NONE',  ( -3.474262827703527901, 87.56481371789857349, 8.843639120294245259 ) ) ;
#36730 = CARTESIAN_POINT ( 'NONE',  ( -13.62178482187498396, 197.6843750006145228, 23.59362340125808188 ) ) ;
#36731 = CARTESIAN_POINT ( 'NONE',  ( -10.69584247140429412, 7.352313717898545598, -6.932735513424201024 ) ) ;
#36732 = CARTESIAN_POINT ( 'NONE',  ( -8.715434833791929847, 69.06018628210145494, -8.962234695871762469 ) ) ;
#36733 = CARTESIAN_POINT ( 'NONE',  ( 19.56230152254411081, -5.196152422706629359, -9.637499998771032139 ) ) ;
#36734 =( BOUNDED_CURVE ( )  B_SPLINE_CURVE ( 2, ( #33277, #18889, #13371, #36479, #4274, #16599, #4830 ),
 .UNSPECIFIED., .F., .F. ) 
 B_SPLINE_CURVE_WITH_KNOTS ( ( 3, 2, 2, 3 ),
 ( 0.5652173913043473386, 0.5724637681159415736, 0.5797101449275359197, 0.5869565217391301548 ),
 .UNSPECIFIED. ) 
 CURVE ( )  GEOMETRIC_REPRESENTATION_ITEM ( )  RATIONAL_B_SPLINE_CURVE ( ( 1.000000000000008216, 0.8660254037844304920, 1.000000000000000000, 0.8660254037844387076, 1.000000000000000000, 0.8660254037844448138, 0.9999999999999938938 ) ) 
 REPRESENTATION_ITEM ( '' )  );
#36735 = CARTESIAN_POINT ( 'NONE',  ( 28.07136751237244354, 5.196152422706636465, 165.2472402554827795 ) ) ;
#36736 = CARTESIAN_POINT ( 'NONE',  ( 30.69144623189632526, 7.209453229046475009, 160.7737373199828426 ) ) ;
#36737 = CARTESIAN_POINT ( 'NONE',  ( 13.44051670066910731, 5.407089921784862696, -10.17187499938551554 ) ) ;
#36738 = CARTESIAN_POINT ( 'NONE',  ( 19.68408634441911431, 5.407089921784862696, -6.646874999385543603 ) ) ;
#36739 = CARTESIAN_POINT ( 'NONE',  ( 30.60565229757555628, -6.928203230275514990, 159.7931081634365853 ) ) ;
#36740 = CARTESIAN_POINT ( 'NONE',  ( 36.68087069682425039, 7.347880794884117764E-16, 160.3908927435282692 ) ) ;
#36741 = CARTESIAN_POINT ( 'NONE',  ( -9.500000000000005329, 86.31018628210145494, -0.1745138560725176813 ) ) ;
#36742 = CARTESIAN_POINT ( 'NONE',  ( -77.00000000000002842, 210.0000000000000000, 5.000000000000000000 ) ) ;
#36743 = CARTESIAN_POINT ( 'NONE',  ( -8.962234695871760692, 121.9601862821014464, 8.715434833791933400 ) ) ;
#36744 = DIRECTION ( 'NONE',  ( 0.000000000000000000, 0.000000000000000000, 1.000000000000000000 ) ) ;
#36745 = CARTESIAN_POINT ( 'NONE',  ( 20.99999999999999289, 240.4937500012290457, -5.999999999999997335 ) ) ;
#36746 = EDGE_LOOP ( 'NONE', ( #13389, #32825, #35832, #10426 ) ) ;
#36747 = CARTESIAN_POINT ( 'NONE',  ( 37.21848120135211957, 3.604726614523238837, 163.7411606810585454 ) ) ;
#36748 = CARTESIAN_POINT ( 'NONE',  ( 23.87821517812500005, -4.985214923628404016, -5.390624999385473792 ) ) ;
#36749 = AXIS2_PLACEMENT_3D ( 'NONE', #6528, #6339, #9929 ) ;
#36750 = CARTESIAN_POINT ( 'NONE',  ( 5.778771075727756162E-15, 197.7218750006145456, 31.45816453501076637 ) ) ;
#36751 = CARTESIAN_POINT ( 'NONE',  ( 1.069080835302379631E-14, 199.3250000012290286, 27.00000000000000000 ) ) ;
#36752 = CARTESIAN_POINT ( 'NONE',  ( 25.43903251657823006, 3.464101615137757051, 169.5806533121757695 ) ) ;
#36753 = CARTESIAN_POINT ( 'NONE',  ( 15.00000000000000178, 239.7437500012290457, 3.464101615137757051 ) ) ;
#36754 = CARTESIAN_POINT ( 'NONE',  ( 15.00000000000000000, 250.0000000000000000, 0.000000000000000000 ) ) ;
#36755 = CARTESIAN_POINT ( 'NONE',  ( 20.99999999999999645, 185.0294372515228645, 0.000000000000000000 ) ) ;
#36756 = CARTESIAN_POINT ( 'NONE',  ( -4.944772684328424539, 137.0148137178985621, -11.48171059495408031 ) ) ;
#36757 = CARTESIAN_POINT ( 'NONE',  ( -1.926257025242585782E-15, 195.2468750006145513, -31.45816453501076637 ) ) ;
#36759 = ORIENTED_EDGE ( 'NONE', *, *, #3459, .F. ) ;
#36758 = EDGE_LOOP ( 'NONE', ( #32994, #24644 ) ) ;
#36760 = CARTESIAN_POINT ( 'NONE',  ( 21.00000000000000000, 245.5843750006145569, -6.646953231504538984 ) ) ;
#36761 = DIRECTION ( 'NONE',  ( 0.08715574274765150453, 0.000000000000000000, 0.9961946980917461003 ) ) ;
#36762 = CARTESIAN_POINT ( 'NONE',  ( 21.00000000000000000, 6.646953231504538984, -2.953124999385479565 ) ) ;
#36763 = CARTESIAN_POINT ( 'NONE',  ( -0.1745138560722442889, 119.1898137178985593, -15.50000000000000533 ) ) ;
#36764 = CARTESIAN_POINT ( 'NONE',  ( -1.045839947578415010E-13, 196.5125000000000455, 27.00000000000000355 ) ) ;
#36765 = CARTESIAN_POINT ( 'NONE',  ( 18.12178482187499640, 4.985214923628404904, -2.128124999385472282 ) ) ;
#36766 = CARTESIAN_POINT ( 'NONE',  ( 13.44051670066911264, -5.407089921784865361, -8.671874999385515537 ) ) ;
#36767 = CARTESIAN_POINT ( 'NONE',  ( -1.909035429704832693E-15, 198.6500000012290457, -31.17691453623979214 ) ) ;
#36768 = CARTESIAN_POINT ( 'NONE',  ( 2.660918448318279950, 107.2976862821014521, -12.46528703574805697 ) ) ;
#36769 = FACE_OUTER_BOUND ( 'NONE', #35906, .T. ) ;
#36770 = CARTESIAN_POINT ( 'NONE',  ( -42.27752896937850835, 214.3500491399821897, 7.303452534266821949 ) ) ;
#36771 = CARTESIAN_POINT ( 'NONE',  ( 26.75643035624999655, 244.5343750006144887, 3.323476615752267271 ) ) ;
#36772 = CARTESIAN_POINT ( 'NONE',  ( -65.82961230271179431, 211.8571965466040297, 6.469044688360755302 ) ) ;
#36773 = CARTESIAN_POINT ( 'NONE',  ( -11.61527771782819940, 113.3351862821014606, 4.622313124798574258 ) ) ;
#36774 = CARTESIAN_POINT ( 'NONE',  ( 22.56230152254410370, 7.347880794884117764E-16, -1.012499998771038134 ) ) ;
#36775 = CARTESIAN_POINT ( 'NONE',  ( -47.43080436395489841, 203.5000000000000000, -0.1155267958017335561 ) ) ;
#36776 = DIRECTION ( 'NONE',  ( 0.000000000000000000, 0.000000000000000000, -1.000000000000000000 ) ) ;
#36777 = SURFACE_STYLE_USAGE ( .BOTH. , #36963 ) ;
#36778 = B_SPLINE_CURVE_WITH_KNOTS ( 'NONE', 3,
 ( #2984, #35010, #139, #3550, #17406, #11702, #6011, #12074, #20813, #17595, #29126, #23649, #32166, #14741, #17220, #12266, #9240, #32355 ),
 .UNSPECIFIED., .F., .F.,
 ( 4, 2, 2, 2, 2, 2, 2, 2, 4 ),
 ( 0.000000000000000000, 0.001127056113610278064, 0.002254112227220556128, 0.003381168340830834410, 0.004508224454441112257, 0.005635280568051390104, 0.006762336681661668819, 0.007889392795271945799, 0.009016448908882224514 ),
 .UNSPECIFIED. ) ;
#36779 = CARTESIAN_POINT ( 'NONE',  ( -13.04141134922759804, 114.7726862821014322, -8.927990412390657937 ) ) ;
#36780 = CARTESIAN_POINT ( 'NONE',  ( 7.234628195640322446, 199.2325961894323711, 26.99999999999999645 ) ) ;
#36781 = CARTESIAN_POINT ( 'NONE',  ( 12.53471296425194836, 17.02268628210144996, -2.311890736173178418 ) ) ;
#36782 = CARTESIAN_POINT ( 'NONE',  ( 19.56230152254411792, 5.196152422706637353, -9.150000000000046541 ) ) ;
#36783 = EDGE_LOOP ( 'NONE', ( #31145, #10704, #20464, #1841 ) ) ;
#36784 = CYLINDRICAL_SURFACE ( 'NONE', #25774, 5.999999999999999112 ) ;
#36785 = CARTESIAN_POINT ( 'NONE',  ( -5.233372021372430183, 78.54768628210145209, -8.152565276336710909 ) ) ;
#36786 = DIRECTION ( 'NONE',  ( 0.000000000000000000, 0.000000000000000000, 1.000000000000000000 ) ) ;
#36787 = EDGE_CURVE ( 'NONE', #17895, #5701, #25671, .T. ) ;
#36788 = CARTESIAN_POINT ( 'NONE',  ( 27.24356964375000345, 196.8781250006145171, -3.336375036156643733E-15 ) ) ;
#36789 = CARTESIAN_POINT ( 'NONE',  ( 20.99999999999999645, 6.928203230275506996, -2.812499999999997335 ) ) ;
#36790 = CARTESIAN_POINT ( 'NONE',  ( 27.24356964375000345, 198.7343750006145626, -3.336375036156643733E-15 ) ) ;
#36791 = CARTESIAN_POINT ( 'NONE',  ( 24.00000000000000000, -5.196152422706629359, -1.593749998770960241 ) ) ;
#36792 = EDGE_CURVE ( 'NONE', #13953, #805, #34524, .T. ) ;
#36793 = CARTESIAN_POINT ( 'NONE',  ( 10.56230152254410726, 0.000000000000000000, -6.637499998771001941 ) ) ;
#36794 = CARTESIAN_POINT ( 'NONE',  ( -5.233372021372612259, 51.05231371789854222, 8.152565276336593669 ) ) ;
#36795 = CARTESIAN_POINT ( 'NONE',  ( 21.00000000000000000, -6.928203230275506996, -8.437499999999991118 ) ) ;
#36796 = ORIENTED_EDGE ( 'NONE', *, *, #31483, .T. ) ;
#36797 = CARTESIAN_POINT ( 'NONE',  ( 21.00000000000000000, 241.6187500012291025, 6.928203230275506996 ) ) ;
#36798 = CARTESIAN_POINT ( 'NONE',  ( -4.944772684328424539, 63.41481371789856070, -11.48171059495408031 ) ) ;
#36799 = CARTESIAN_POINT ( 'NONE',  ( 13.44051670066911086, 5.407089921784862696, -5.671874999385540406 ) ) ;
#36800 = CARTESIAN_POINT ( 'NONE',  ( -27.24356964375000345, 198.0031250006145456, 0.000000000000000000 ) ) ;
#36801 = CARTESIAN_POINT ( 'NONE',  ( 26.75643035624999655, 7.049594010296217766E-16, -6.778124999385487293 ) ) ;
#36802 = CARTESIAN_POINT ( 'NONE',  ( 12.46528703574811558, 29.20231371789855501, -2.660918448318005503 ) ) ;
#36803 = EDGE_CURVE ( 'NONE', #34283, #27158, #31733, .T. ) ;
#36804 = ORIENTED_EDGE ( 'NONE', *, *, #6243, .T. ) ;
#36805 = VECTOR ( 'NONE', #33915, 1000.000000000000000 ) ;
#36806 = CARTESIAN_POINT ( 'NONE',  ( 22.80587116629411426, -3.604726614523238837, -1.809374999385491511 ) ) ;
#36807 = CARTESIAN_POINT ( 'NONE',  ( 6.932735513423970097, 9.547686282101453870, 10.69584247140445044 ) ) ;
#36808 = CARTESIAN_POINT ( 'NONE',  ( 25.14001085782205891, 3.604726614523240613, 168.9574683606716690 ) ) ;
#36809 = CARTESIAN_POINT ( 'NONE',  ( -43.66294563604516554, 214.6737587650350747, -4.842901733360249317 ) ) ;
#36810 = CARTESIAN_POINT ( 'NONE',  ( 37.38356387272733627, -3.464101615137664236, 168.4227124968929559 ) ) ;
#36811 =( NAMED_UNIT ( * ) PLANE_ANGLE_UNIT ( ) SI_UNIT ( $, .RADIAN. ) );
#36812 = CARTESIAN_POINT ( 'NONE',  ( 10.56230152254450161, 3.464101615137985757, -2.737500000000008260 ) ) ;
#36813 = CARTESIAN_POINT ( 'NONE',  ( 2.660918448318002838, 68.30231371789854222, 12.46528703574811558 ) ) ;
#36814 = CARTESIAN_POINT ( 'NONE',  ( -38.72247103062156981, 207.6499508600178387, 3.839350919129076445 ) ) ;
#36815 = CARTESIAN_POINT ( 'NONE',  ( -39.90997103062156270, 215.5714017266979852, 3.350049139982118618 ) ) ;
#36816 = AXIS2_PLACEMENT_3D ( 'NONE', #32874, #7292, #16017 ) ;
#36817 = FACE_OUTER_BOUND ( 'NONE', #11239, .T. ) ;
#36818 = CARTESIAN_POINT ( 'NONE',  ( -12.42035509746875022, 216.7950050350868310, -4.614743948463994272 ) ) ;
#36819 = CARTESIAN_POINT ( 'NONE',  ( -15.50000000000000533, 43.28981371789856070, 0.1745138560722471477 ) ) ;
#36820 = CARTESIAN_POINT ( 'NONE',  ( -33.76711230271183695, 218.4690446883607535, -2.393094931466363651 ) ) ;
#36821 = CARTESIAN_POINT ( 'NONE',  ( -0.1745138560725500443, 19.61018628210144144, 12.50000000000000355 ) ) ;
#36822 =( BOUNDED_CURVE ( )  B_SPLINE_CURVE ( 2, ( #12241, #12622, #32705, #1049, #3899, #9593, #24002 ),
 .UNSPECIFIED., .F., .F. ) 
 B_SPLINE_CURVE_WITH_KNOTS ( ( 3, 2, 2, 3 ),
 ( 0.3695652173913038796, 0.3768115942028982257, 0.3840579710144925163, 0.3913043478260868624 ),
 .UNSPECIFIED. ) 
 CURVE ( )  GEOMETRIC_REPRESENTATION_ITEM ( )  RATIONAL_B_SPLINE_CURVE ( ( 1.000000000000008216, 0.8660254037844304920, 1.000000000000000000, 0.8660254037844387076, 1.000000000000000000, 0.8660254037844407060, 0.9999999999999980016 ) ) 
 REPRESENTATION_ITEM ( '' )  );
#36823 = CARTESIAN_POINT ( 'NONE',  ( -8.715434833791929847, 59.86018628210145209, -8.962234695871762469 ) ) ;
#36824 = CARTESIAN_POINT ( 'NONE',  ( -14.25334919248782306, 4.085186282101443744, -6.092822981423979378 ) ) ;
#36825 = CARTESIAN_POINT ( 'NONE',  ( 10.56230152254410726, -3.464101615137761048, -1.762500000000049916 ) ) ;
#36826 = CYLINDRICAL_SURFACE ( 'NONE', #13760, 6.000000000000001776 ) ;
#36827 = EDGE_LOOP ( 'NONE', ( #16428, #31863 ) ) ;
#36828 = CARTESIAN_POINT ( 'NONE',  ( -5.770363421893818234, 23.63518628210144357, -14.38691631536207005 ) ) ;
#36829 = CARTESIAN_POINT ( 'NONE',  ( -1.926257025242585782E-15, 196.0906250006145228, -31.45816453501076637 ) ) ;
#36830 = CARTESIAN_POINT ( 'NONE',  ( -13.62178482187500528, 199.3343750006145569, -23.59362340125807123 ) ) ;
#36831 = CARTESIAN_POINT ( 'NONE',  ( 37.10248660225891371, 7.347880794884125653E-16, 165.2099845943227479 ) ) ;
#36832 = DIRECTION ( 'NONE',  ( 0.000000000000000000, -0.000000000000000000, -1.000000000000000000 ) ) ;
#36833 = CARTESIAN_POINT ( 'NONE',  ( -6.932735513423968321, 4.947686282101432909, -10.69584247140445221 ) ) ;
#36834 = CARTESIAN_POINT ( 'NONE',  ( 15.24356964374999990, 247.1218750006145228, -3.323476615752268604 ) ) ;
#36835 = CARTESIAN_POINT ( 'NONE',  ( 6.840914352311949109, 113.4398137178985593, 6.594114490232462877 ) ) ;
#36836 = CARTESIAN_POINT ( 'NONE',  ( 15.24356964374999990, 242.1718750006145058, -3.323476615752268604 ) ) ;
#36837 = ORIENTED_EDGE ( 'NONE', *, *, #30706, .T. ) ;
#36838 = CARTESIAN_POINT ( 'NONE',  ( -67.42038769728823411, 208.1428034533959703, 6.469044688360770401 ) ) ;
#36839 = CARTESIAN_POINT ( 'NONE',  ( 15.00000000000000000, 249.6062500012290570, 0.000000000000000000 ) ) ;
#36840 = CARTESIAN_POINT ( 'NONE',  ( 24.00000000000000000, 249.3062500012290457, 5.196152422706629359 ) ) ;
#36841 = CARTESIAN_POINT ( 'NONE',  ( -12.53471296425189152, 126.3773137178985593, -2.311890736173453309 ) ) ;
#36842 = CARTESIAN_POINT ( 'NONE',  ( 22.80587116629410716, 7.646167579472015790E-16, -9.365624999385563143 ) ) ;
#36843 = CARTESIAN_POINT ( 'NONE',  ( 33.83730346391489263, 5.407089921784857367, 160.9125861580968149 ) ) ;
#36844 = CARTESIAN_POINT ( 'NONE',  ( 23.87821517812499650, 4.985214923628404904, -0.4031249993854957303 ) ) ;
#36845 = CARTESIAN_POINT ( 'NONE',  ( -27.00000000000000355, 196.3625000000000114, -15.58845726811989429 ) ) ;
#36846 = VERTEX_POINT ( 'NONE', #20511 ) ;
#36847 = EDGE_LOOP ( 'NONE', ( #34476, #37157, #32030, #5108 ) ) ;
#36848 = ORIENTED_EDGE ( 'NONE', *, *, #29160, .F. ) ;
#36849 = CARTESIAN_POINT ( 'NONE',  ( 21.00000000000000000, -6.928203230275506996, -3.881249998770961884 ) ) ;
#36850 = CARTESIAN_POINT ( 'NONE',  ( 26.75643035624999655, 3.323476615752271268, -3.028124999385441107 ) ) ;
#36851 = CARTESIAN_POINT ( 'NONE',  ( 0.000000000000000000, 200.0000000000000000, 0.000000000000000000 ) ) ;
#36852 = DIRECTION ( 'NONE',  ( 1.000000000000000000, 0.000000000000000000, 0.000000000000000000 ) ) ;
#36853 = CARTESIAN_POINT ( 'NONE',  ( 15.24356964374999990, 249.2968750006145058, 0.000000000000000000 ) ) ;
#36854 = CARTESIAN_POINT ( 'NONE',  ( 2.660918448318279950, 61.29768628210143788, -12.46528703574805697 ) ) ;
#36855 = CARTESIAN_POINT ( 'NONE',  ( -61.87127896937849414, 216.5309553116392181, 1.626142955000506429 ) ) ;
#36856 = CARTESIAN_POINT ( 'NONE',  ( 15.15359421270862050, 225.5904154327813842, -1.363118671455028297 ) ) ;
#36857 = CARTESIAN_POINT ( 'NONE',  ( -44.25669563604517265, 209.8844732041982297, -4.499999999999996447 ) ) ;
#36858 = DIRECTION ( 'NONE',  ( 0.000000000000000000, 0.000000000000000000, 1.000000000000000000 ) ) ;
#36859 = CARTESIAN_POINT ( 'NONE',  ( 31.10570837169731817, 6.928203230275506996, 165.5087752449623224 ) ) ;
#36860 = CARTESIAN_POINT ( 'NONE',  ( -2.311890736173448424, 124.0773137178985621, 12.53471296425189330 ) ) ;
#36861 = CARTESIAN_POINT ( 'NONE',  ( -66.23288769728823411, 205.5309553116392465, -1.321298161741839117 ) ) ;
#36862 = CARTESIAN_POINT ( 'NONE',  ( -60.88913769728824121, 205.8500491399820760, -7.418979330068584233 ) ) ;
#36863 = CARTESIAN_POINT ( 'NONE',  ( 23.87821517812499650, 4.985214923628404904, -0.8531249993854739255 ) ) ;
#36864 = CARTESIAN_POINT ( 'NONE',  ( -13.62178482187500528, 196.1281250006145171, -23.59362340125807123 ) ) ;
#36865 = CARTESIAN_POINT ( 'NONE',  ( -14.38691631536193860, 89.86481371789855643, -5.770363421894132649 ) ) ;
#36866 = CARTESIAN_POINT ( 'NONE',  ( -32.57961230271183695, 211.8571965466040297, 6.469044688360755302 ) ) ;
#36867 = VERTEX_POINT ( 'NONE', #5384 ) ;
#36868 = CARTESIAN_POINT ( 'NONE',  ( 21.00000000000000000, 249.0437500012290570, -5.999999999999998224 ) ) ;
#36869 = CARTESIAN_POINT ( 'NONE',  ( 10.49813415415989581, 119.3726862821014549, 7.228626920339068285 ) ) ;
#36870 = CARTESIAN_POINT ( 'NONE',  ( 14.25334919248782661, 63.88518628210145778, 6.092822981423971385 ) ) ;
#36871 = PLANE ( 'NONE',  #27738 ) ;
#36872 = CARTESIAN_POINT ( 'NONE',  ( 27.90674060888834518, -5.407089921784865361, 164.7628702620865226 ) ) ;
#36873 = CARTESIAN_POINT ( 'NONE',  ( 15.53471296425195369, 90.62268628210145494, -2.908627838312120684 ) ) ;
#36874 = CARTESIAN_POINT ( 'NONE',  ( -48.02455436395489841, 205.1570982666397640, 4.673758765035199048 ) ) ;
#36875 = CARTESIAN_POINT ( 'NONE',  ( 10.31873187879411269, -3.604726614523240613, -6.403124999385521043 ) ) ;
#36876 = CARTESIAN_POINT ( 'NONE',  ( -1.715153634034234598, 23.92268628210143788, -9.534712964251941258 ) ) ;
#36877 = CARTESIAN_POINT ( 'NONE',  ( 36.67760235647196509, -3.464101615137322288, 160.3535354423497949 ) ) ;
#36878 = CARTESIAN_POINT ( 'NONE',  ( -65.44122103062157692, 208.3738570449993404, -6.530955311639226935 ) ) ;
#36879 = CARTESIAN_POINT ( 'NONE',  ( 20.99999999999999645, 250.0000000000000000, 8.000000000000000000 ) ) ;
#36880 = CARTESIAN_POINT ( 'NONE',  ( -11.48171059495397373, 59.28518628210144215, -4.944772684328680334 ) ) ;
#36881 = CARTESIAN_POINT ( 'NONE',  ( -27.00000000000000355, 197.2624999999999886, -15.58845726811989429 ) ) ;
#36882 = DIRECTION ( 'NONE',  ( 0.08715574274765150453, 0.000000000000000000, 0.9961946980917461003 ) ) ;
#36884 = CARTESIAN_POINT ( 'NONE',  ( 22.80587116629412847, 3.604726614523243278, -1.734374999385497551 ) ) ;
#36883 = CARTESIAN_POINT ( 'NONE',  ( 7.954856959092191815, 18.17268628210144499, 5.529263428287477744 ) ) ;
#36885 = CARTESIAN_POINT ( 'NONE',  ( 26.75643035624999655, 249.6343750006145399, -7.049594010296217766E-16 ) ) ;
#36886 = EDGE_LOOP ( 'NONE', ( #9689, #32270, #2857, #29004 ) ) ;
#36887 = CARTESIAN_POINT ( 'NONE',  ( 15.00000000000000000, 3.464101615137752166, -2.737500000000003375 ) ) ;
#36888 =( BOUNDED_CURVE ( )  B_SPLINE_CURVE ( 2, ( #18018, #7208, #32782, #21055, #30131, #35996, #35431 ),
 .UNSPECIFIED., .F., .F. ) 
 B_SPLINE_CURVE_WITH_KNOTS ( ( 3, 2, 2, 3 ),
 ( 0.1739130434782605039, 0.1811594202898547945, 0.1884057971014491129, 0.1956521739130434034 ),
 .UNSPECIFIED. ) 
 CURVE ( )  GEOMETRIC_REPRESENTATION_ITEM ( )  RATIONAL_B_SPLINE_CURVE ( ( 1.000000000000006661, 0.8660254037844320463, 1.000000000000000000, 0.8660254037844387076, 1.000000000000000000, 0.8660254037844402619, 0.9999999999999984457 ) ) 
 REPRESENTATION_ITEM ( '' )  );
#36889 = CARTESIAN_POINT ( 'NONE',  ( 20.96843863229867821, -5.998110342775703430, -8.000000000000003553 ) ) ;
#36890 = CARTESIAN_POINT ( 'NONE',  ( 24.51902619074504130, -3.604726614523244610, 161.8595811367679573 ) ) ;
#36891 = CARTESIAN_POINT ( 'NONE',  ( 13.44051670066911441, -5.407089921784859143, -2.315624999385534899 ) ) ;
#36892 = CARTESIAN_POINT ( 'NONE',  ( 37.60414536301047406, -3.604726614523235284, 168.1493222201144704 ) ) ;
#36893 = CARTESIAN_POINT ( 'NONE',  ( 21.00000000000000000, 243.8124999999999716, 6.928203230275506996 ) ) ;
#36894 = CARTESIAN_POINT ( 'NONE',  ( 0.1745138560725515708, 79.41018628210144925, -12.50000000000000355 ) ) ;
#36895 = ORIENTED_EDGE ( 'NONE', *, *, #352, .F. ) ;
#36896 = ORIENTED_EDGE ( 'NONE', *, *, #21200, .F. ) ;
#36897 = CARTESIAN_POINT ( 'NONE',  ( -13.50000000000000533, 196.8875000012290286, -23.38268590217984411 ) ) ;
#36898 = CARTESIAN_POINT ( 'NONE',  ( 20.99999999999999645, 185.0294372515228645, 0.000000000000000000 ) ) ;
#36899 = CARTESIAN_POINT ( 'NONE',  ( -13.23911966647199812, 62.55231371789854222, -8.632099005475788900 ) ) ;
#36900 = CARTESIAN_POINT ( 'NONE',  ( 15.24356964374999990, 0.000000000000000000, -10.15312499938547575 ) ) ;
#36901 = CARTESIAN_POINT ( 'NONE',  ( 15.24356964374999990, 242.1718750006145342, -3.323476615752268604 ) ) ;
#36902 = CARTESIAN_POINT ( 'NONE',  ( -38.12872103062156270, 205.4690446883607535, 1.090244570138264368 ) ) ;
#36903 = CARTESIAN_POINT ( 'NONE',  ( -3.474262827703527901, 32.36481371789854933, 8.843639120294245259 ) ) ;
#36904 = CARTESIAN_POINT ( 'NONE',  ( 11.28998163430637725, -3.344369132205555317, -9.999999999999998224 ) ) ;
#36905 = ADVANCED_FACE ( 'NONE', ( #23721 ), #22468, .F. ) ;
#36906 = VECTOR ( 'NONE', #9717, 1000.000000000000000 ) ;
#36907 = CARTESIAN_POINT ( 'NONE',  ( 8.843639120294245259, 103.6648137178985678, 3.474262827703527901 ) ) ;
#36908 = CARTESIAN_POINT ( 'NONE',  ( 5.778771075727756162E-15, 198.1718750006145342, 31.45816453501075927 ) ) ;
#36909 = CARTESIAN_POINT ( 'NONE',  ( -15.50000000000000533, 144.4898137178985280, 0.1745138560722471477 ) ) ;
#36910 = CARTESIAN_POINT ( 'NONE',  ( -4.944772684328673229, 66.18518628210144072, 11.48171059495397728 ) ) ;
#36911 = EDGE_CURVE ( 'NONE', #11078, #24827, #12502, .T. ) ;
#36912 = CARTESIAN_POINT ( 'NONE',  ( 0.000000000000000000, 200.0000000000000000, 0.000000000000000000 ) ) ;
#36913 = CARTESIAN_POINT ( 'NONE',  ( 30.80910648460565682, 7.209453229046475009, 162.1186001624066932 ) ) ;
#36914 = CARTESIAN_POINT ( 'NONE',  ( 19.68408634441911431, -5.407089921784861808, -9.946874999385540761 ) ) ;
#36915 = CARTESIAN_POINT ( 'NONE',  ( 22.80587116629411426, 7.646167579472024665E-16, -6.721874999385535787 ) ) ;
#36916 = DIRECTION ( 'NONE',  ( 0.000000000000000000, 0.000000000000000000, 1.000000000000000000 ) ) ;
#36917 = AXIS2_PLACEMENT_3D ( 'NONE', #19205, #33591, #36980 ) ;
#36918 = CARTESIAN_POINT ( 'NONE',  ( -1.045839947578415010E-13, 195.7250000012290343, 27.00000000000000355 ) ) ;
#36919 = CARTESIAN_POINT ( 'NONE',  ( -9.465287035748065847, 68.19768628210142936, -2.064181346179273735 ) ) ;
#36920 = CARTESIAN_POINT ( 'NONE',  ( 16.56230152254411792, 6.928203230275514990, -5.962500000000031442 ) ) ;
#36921 = EDGE_CURVE ( 'NONE', #17495, #26168, #26358, .T. ) ;
#36922 = CARTESIAN_POINT ( 'NONE',  ( -2.311890736173176641, 115.9226862821014521, -12.53471296425194836 ) ) ;
#36923 = DIRECTION ( 'NONE',  ( 0.000000000000000000, 1.000000000000000000, 0.000000000000000000 ) ) ;
#36924 = FACE_OUTER_BOUND ( 'NONE', #30095, .T. ) ;
#36925 = ORIENTED_EDGE ( 'NONE', *, *, #7484, .T. ) ;
#36926 = CARTESIAN_POINT ( 'NONE',  ( 24.60236886974748671, -3.604726614523240613, 162.8121923168181695 ) ) ;
#36927 = CARTESIAN_POINT ( 'NONE',  ( 21.00000000000000000, -6.646953231504538984, -6.328124999385495997 ) ) ;
#36928 = ADVANCED_FACE ( 'NONE', ( #3242 ), #26549, .F. ) ;
#36929 = CARTESIAN_POINT ( 'NONE',  ( -27.24356964375000345, 196.6718750006145342, -15.72908226750537786 ) ) ;
#36930 = CARTESIAN_POINT ( 'NONE',  ( 25.06157068934917120, 3.604726614523240613, 168.0608931323890829 ) ) ;
#36931 =( BOUNDED_CURVE ( )  B_SPLINE_CURVE ( 3, ( #23511, #7576, #7024, #21431 ),
 .UNSPECIFIED., .F., .F. ) 
 B_SPLINE_CURVE_WITH_KNOTS ( ( 4, 4 ),
 ( 1.224646799147353454E-16, 1.570796326794895448 ),
 .UNSPECIFIED. ) 
 CURVE ( )  GEOMETRIC_REPRESENTATION_ITEM ( )  RATIONAL_B_SPLINE_CURVE ( ( 1.000000000000000000, 0.8047378541243652705, 0.8047378541243652705, 1.000000000000000000 ) ) 
 REPRESENTATION_ITEM ( '' )  );
#36932 = CARTESIAN_POINT ( 'NONE',  ( 25.20698035151260896, 0.000000000000000000, 166.9282849285064856 ) ) ;
#36933 = DIRECTION ( 'NONE',  ( 0.000000000000000000, 0.000000000000000000, -1.000000000000000000 ) ) ;
#36934 = CARTESIAN_POINT ( 'NONE',  ( 23.87821517812499650, 240.2593750006145399, -4.985214923628404904 ) ) ;
#36935 = EDGE_CURVE ( 'NONE', #2167, #12999, #22706, .T. ) ;
#36936 = CARTESIAN_POINT ( 'NONE',  ( 11.61527771782809637, 131.2648137178985621, 4.622313124798827388 ) ) ;
#36937 = CARTESIAN_POINT ( 'NONE',  ( -6.932735513423968321, 133.7476862821014549, -10.69584247140445221 ) ) ;
#36938 = PRESENTATION_LAYER_ASSIGNMENT (  '', '', ( #13958 ) ) ;
#36940 = ORIENTED_EDGE ( 'NONE', *, *, #29389, .F. ) ;
#36939 = ORIENTED_EDGE ( 'NONE', *, *, #4577, .F. ) ;
#36941 = CARTESIAN_POINT ( 'NONE',  ( 26.75643035624999655, 244.1593750006145171, -3.323476615752271712 ) ) ;
#36942 = DIRECTION ( 'NONE',  ( -0.000000000000000000, -1.000000000000000000, -0.000000000000000000 ) ) ;
#36943 = CARTESIAN_POINT ( 'NONE',  ( 23.87821517812500005, -4.985214923628404016, -4.940624999385468286 ) ) ;
#36944 = CARTESIAN_POINT ( 'NONE',  ( -8.632099005475794229, 115.4523137178985479, 13.23911966647199812 ) ) ;
#36945 = CARTESIAN_POINT ( 'NONE',  ( 10.56230152254410726, 0.000000000000000000, -9.900000000000048317 ) ) ;
#36946 = CARTESIAN_POINT ( 'NONE',  ( 15.24356964374999990, 3.323476615752268604, -0.7406249993854975289 ) ) ;
#36947 = CARTESIAN_POINT ( 'NONE',  ( 19.68408634441910721, 5.407089921784862696, -8.896874999385516958 ) ) ;
#36948 = CARTESIAN_POINT ( 'NONE',  ( -13.50000000000000533, 197.7875000012290627, -23.38268590217984411 ) ) ;
#36949 = CARTESIAN_POINT ( 'NONE',  ( -10.49813415415989581, 105.5726862821014578, -7.228626920339068285 ) ) ;
#36950 = CARTESIAN_POINT ( 'NONE',  ( 22.80587116629411071, 3.604726614523238837, -2.128124999385546001 ) ) ;
#36951 =( BOUNDED_CURVE ( )  B_SPLINE_CURVE ( 3, ( #35483, #35673, #18258, #30377 ),
 .UNSPECIFIED., .F., .F. ) 
 B_SPLINE_CURVE_WITH_KNOTS ( ( 4, 4 ),
 ( 4.712388980384648818, 6.283185307179586232 ),
 .UNSPECIFIED. ) 
 CURVE ( )  GEOMETRIC_REPRESENTATION_ITEM ( )  RATIONAL_B_SPLINE_CURVE ( ( 1.000000000000000000, 0.8047378541243555006, 0.8047378541243555006, 1.000000000000000000 ) ) 
 REPRESENTATION_ITEM ( '' )  );
#36952 = CARTESIAN_POINT ( 'NONE',  ( -48.41294563604517265, 216.1378603801729241, -6.307003348498026796 ) ) ;
#36953 = CARTESIAN_POINT ( 'NONE',  ( 26.75643035624999655, 244.5718750006145115, -7.049594010296217766E-16 ) ) ;
#36954 = CARTESIAN_POINT ( 'NONE',  ( 20.99999999999999289, 240.4374999999999716, -5.999999999999997335 ) ) ;
#36955 = EDGE_CURVE ( 'NONE', #19175, #11807, #19823, .T. ) ;
#36956 = CARTESIAN_POINT ( 'NONE',  ( -67.01711230271183695, 216.4690446883607535, -1.857196546604089393 ) ) ;
#36957 = CARTESIAN_POINT ( 'NONE',  ( 11.61527771782819940, 127.1351862821014578, -4.622313124798573369 ) ) ;
#36958 = CARTESIAN_POINT ( 'NONE',  ( 22.56230152254410370, 3.464101615137755275, -1.424999998770983600 ) ) ;
#36959 = ADVANCED_FACE ( 'NONE', ( #2363 ), #14815, .T. ) ;
#36960 = CARTESIAN_POINT ( 'NONE',  ( -48.02455436395488420, 205.1570982666397356, 4.673758765035198159 ) ) ;
#36961 = DIRECTION ( 'NONE',  ( 0.9961946980917462113, 0.000000000000000000, -0.08715574274765118534 ) ) ;
#36962 = VECTOR ( 'NONE', #22885, 999.9999999999998863 ) ;
#36963 = SURFACE_SIDE_STYLE ('',( #13297 ) ) ;
#36964 = CARTESIAN_POINT ( 'NONE',  ( -13.04141134922759804, 123.9726862821014493, -8.927990412390657937 ) ) ;
#36965 = CARTESIAN_POINT ( 'NONE',  ( 2.660918448318279950, 24.49768628210144428, -12.46528703574805874 ) ) ;
#36966 = EDGE_CURVE ( 'NONE', #8971, #590, #5956, .T. ) ;
#36967 = CARTESIAN_POINT ( 'NONE',  ( 26.99999999999999645, 7.347880794884117764E-16, -2.418749998770952647 ) ) ;
#36968 = CARTESIAN_POINT ( 'NONE',  ( -3.474262827703337830, 134.0351862821014493, -8.843639120294326972 ) ) ;
#36969 = CARTESIAN_POINT ( 'NONE',  ( 22.80587116629410360, -3.604726614523235284, -0.4031249993855248182 ) ) ;
#36970 = CARTESIAN_POINT ( 'NONE',  ( 22.56230152254410726, 7.347880794884117764E-16, -9.112499998771033560 ) ) ;
#36971 = VERTEX_POINT ( 'NONE', #18230 ) ;
#36972 = CARTESIAN_POINT ( 'NONE',  ( 5.499999999999994671, 244.5000000000000000, 0.000000000000000000 ) ) ;
#36973 = CARTESIAN_POINT ( 'NONE',  ( -2.064181346179269738, 75.09768628210143504, 9.465287035748067623 ) ) ;
#36974 = CARTESIAN_POINT ( 'NONE',  ( 10.56230152254521037, 3.464101615138387658, -2.174999998771001142 ) ) ;
#36975 = EDGE_CURVE ( 'NONE', #32162, #3136, #23911, .T. ) ;
#36976 = CARTESIAN_POINT ( 'NONE',  ( 13.62178482187501416, 196.3531250006145115, 23.59362340125806767 ) ) ;
#36977 = DIRECTION ( 'NONE',  ( 0.08715574274765150453, 0.000000000000000000, 0.9961946980917461003 ) ) ;
#36978 = CARTESIAN_POINT ( 'NONE',  ( -27.24356964374999635, 195.8468750006145171, 15.72908226750539384 ) ) ;
#36979 = DIRECTION ( 'NONE',  ( 0.000000000000000000, 0.000000000000000000, 1.000000000000000000 ) ) ;
#36980 = DIRECTION ( 'NONE',  ( 1.000000000000000000, 0.000000000000000000, -0.000000000000000000 ) ) ;
#36981 = CARTESIAN_POINT ( 'NONE',  ( 6.840914352311949109, 49.03981371789855359, 6.594114490232462877 ) ) ;
#36982 = CARTESIAN_POINT ( 'NONE',  ( 18.00000000000000000, 5.196152422706630247, -8.624999999999992895 ) ) ;
#36983 = EDGE_LOOP ( 'NONE', ( #2995, #16085, #18555, #25920 ) ) ;
#36984 = CARTESIAN_POINT ( 'NONE',  ( 18.00000000000000000, 242.3312500012290513, -5.196152422706630247 ) ) ;
#36985 = CARTESIAN_POINT ( 'NONE',  ( 4.622313124798831829, 64.56481371789855928, -11.61527771782809282 ) ) ;
#36986 = CARTESIAN_POINT ( 'NONE',  ( 13.44051670066911086, 5.407089921784862696, -6.121874999385518379 ) ) ;
#36987 = CARTESIAN_POINT ( 'NONE',  ( 23.87821517812500005, -4.985214923628404016, -7.753124999385491378 ) ) ;
#36988 = CARTESIAN_POINT ( 'NONE',  ( -12.46528703574811558, 24.60231371789854649, 2.660918448318003726 ) ) ;
#36989 = VECTOR ( 'NONE', #3029, 1000.000000000000000 ) ;
#36990 = ORIENTED_EDGE ( 'NONE', *, *, #13782, .F. ) ;
#36991 = CARTESIAN_POINT ( 'NONE',  ( 22.80587116629411781, 7.646167579472024665E-16, -0.8718749993855412495 ) ) ;
#36992 = CARTESIAN_POINT ( 'NONE',  ( 11.48171059495397728, 8.685186282101437172, 4.944772684328674117 ) ) ;
#36993 = CARTESIAN_POINT ( 'NONE',  ( 25.10732745429168489, -3.604726614523244610, 168.5838953488872676 ) ) ;
#36994 = CARTESIAN_POINT ( 'NONE',  ( -46.03794563604517265, 205.3262412349647832, 4.842901733360250205 ) ) ;
#36995 = CARTESIAN_POINT ( 'NONE',  ( 20.99999999999999645, 185.0294372515228645, 5.999999999999999112 ) ) ;
#36996 = CARTESIAN_POINT ( 'NONE',  ( 22.56230152254412502, 7.347880794884125653E-16, -2.925000000000066436 ) ) ;
#36997 = ADVANCED_FACE ( 'NONE', ( #29770 ), #26928, .F. ) ;
#36998 = CARTESIAN_POINT ( 'NONE',  ( -40.70163769728823411, 213.9548777149308592, -2.149950860017830756 ) ) ;
#36999 = CARTESIAN_POINT ( 'NONE',  ( -41.29538769728821990, 211.8571965466039444, -6.469044688360768625 ) ) ;
#37000 = ORIENTED_EDGE ( 'NONE', *, *, #19700, .T. ) ;
#37001 = DIRECTION ( 'NONE',  ( 0.000000000000000000, 0.000000000000000000, -1.000000000000000000 ) ) ;
#37002 = CARTESIAN_POINT ( 'NONE',  ( 28.30668801779110311, 5.196152422706636465, 167.9369659403305093 ) ) ;
#37003 = CARTESIAN_POINT ( 'NONE',  ( -14.38691631536193860, 34.66481371789854649, -5.770363421894132649 ) ) ;
#37004 = CARTESIAN_POINT ( 'NONE',  ( -35.35044563604517265, 203.6929966515019430, -6.137860380172892150 ) ) ;
#37005 = CARTESIAN_POINT ( 'NONE',  ( -8.962234695871760692, 11.56018628210145316, 8.715434833791933400 ) ) ;
#37006 = VECTOR ( 'NONE', #17132, 1000.000000000000000 ) ;
#37007 = CARTESIAN_POINT ( 'NONE',  ( -10.49813415415989581, 68.77268628210146062, -7.228626920339068285 ) ) ;
#37008 = CARTESIAN_POINT ( 'NONE',  ( -8.632099005475501130, 14.14768628210144286, -13.23911966647218996 ) ) ;
#37009 = CARTESIAN_POINT ( 'NONE',  ( 13.56230152254411436, -5.196152422706638241, -2.625000000000043965 ) ) ;
#37010 = CARTESIAN_POINT ( 'NONE',  ( 18.00000000000000355, 247.8812500012290343, 5.196152422706632912 ) ) ;
#37011 = ORIENTED_EDGE ( 'NONE', *, *, #26262, .F. ) ;
#37012 = CARTESIAN_POINT ( 'NONE',  ( -12.50000000000000355, 141.5101862821014720, -0.1745138560725492671 ) ) ;
#37013 = AXIS2_PLACEMENT_3D ( 'NONE', #19847, #25511, #8637 ) ;
#37014 = CARTESIAN_POINT ( 'NONE',  ( -69.00000000000002842, 209.9999999999999716, -6.500000000000000888 ) ) ;
#37015 = CARTESIAN_POINT ( 'NONE',  ( 27.24356964375000700, 198.6968750006145115, 15.72908226750537075 ) ) ;
#37016 = CARTESIAN_POINT ( 'NONE',  ( 15.00000000000047606, 3.464101615138028389, -5.381249998770973875 ) ) ;
#37017 = CARTESIAN_POINT ( 'NONE',  ( -8.715434833791929847, 4.660186282101435928, -8.962234695871762469 ) ) ;
#37018 = CARTESIAN_POINT ( 'NONE',  ( 26.75643035624999655, 248.7718750006145569, -3.323476615752271712 ) ) ;
#37019 = CARTESIAN_POINT ( 'NONE',  ( -9.534712964251895073, 107.9773137178985394, -1.715153634034446428 ) ) ;
#37020 = CARTESIAN_POINT ( 'NONE',  ( 15.24356964374999990, 242.2093750006145285, 0.000000000000000000 ) ) ;
#37021 = ORIENTED_EDGE ( 'NONE', *, *, #17731, .T. ) ;
#37022 = LINE ( 'NONE', #28674, #17575 ) ;
#37023 = LINE ( 'NONE', #34375, #10546 ) ;
#37024 = CARTESIAN_POINT ( 'NONE',  ( 26.99999999999999645, 248.9312500012290457, -7.347880794884117764E-16 ) ) ;
#37025 = CARTESIAN_POINT ( 'NONE',  ( 0.1745138560722779009, 114.5898137178985650, 12.50000000000000355 ) ) ;
#37026 = CARTESIAN_POINT ( 'NONE',  ( 13.44051670066910908, 5.407089921784856479, -10.11562499938553650 ) ) ;
#37027 = CARTESIAN_POINT ( 'NONE',  ( 27.74168942105997360, 5.407089921784856479, 162.8763265525752786 ) ) ;
#37028 = CARTESIAN_POINT ( 'NONE',  ( 0.000000000000000000, 2.000000000000000000, 0.000000000000000000 ) ) ;
#37029 = CARTESIAN_POINT ( 'NONE',  ( 13.49999999999999645, 195.3500000000000227, -23.38268590217984766 ) ) ;
#37030 = ORIENTED_EDGE ( 'NONE', *, *, #32089, .T. ) ;
#37031 = ORIENTED_EDGE ( 'NONE', *, *, #34192, .T. ) ;
#37032 = ORIENTED_EDGE ( 'NONE', *, *, #4375, .T. ) ;
#37033 = CARTESIAN_POINT ( 'NONE',  ( 26.99999999999999645, -3.464101615137751278, -5.606249998770950427 ) ) ;
#37034 = CARTESIAN_POINT ( 'NONE',  ( 26.75643035624999655, 7.049594010296217766E-16, -2.165624999385467930 ) ) ;
#37035 = DIRECTION ( 'NONE',  ( 0.000000000000000000, 1.000000000000000000, 0.000000000000000000 ) ) ;
#37036 = CARTESIAN_POINT ( 'NONE',  ( 37.25936693920468201, 7.347880794884125653E-16, 167.0031350508878631 ) ) ;
#37037 = CARTESIAN_POINT ( 'NONE',  ( 15.24356964374999990, 3.323476615752268604, -10.07812499938544804 ) ) ;
#37038 = CARTESIAN_POINT ( 'NONE',  ( 2.311890736173175753, 65.32268628210144357, 12.53471296425194836 ) ) ;
#37039 = EDGE_CURVE ( 'NONE', #21823, #31726, #12533, .T. ) ;
#37040 = CARTESIAN_POINT ( 'NONE',  ( -66.02752896937849414, 213.3500491399821613, 5.571401726697954970 ) ) ;
#37041 = CARTESIAN_POINT ( 'NONE',  ( 14.97710761593534556, 216.0228923840610094, -0.2612666680235000150 ) ) ;
#37042 = CARTESIAN_POINT ( 'NONE',  ( -37.52752896937849414, 212.3500491399821613, 3.839350919129088435 ) ) ;
#37043 = EDGE_CURVE ( 'NONE', #32692, #32805, #31646, .T. ) ;
#37044 = CARTESIAN_POINT ( 'NONE',  ( 27.00000000000000355, 197.0749999999999886, -3.306546357697854128E-15 ) ) ;
#37045 = CARTESIAN_POINT ( 'NONE',  ( 30.94882803475154986, 6.928203230275506996, 163.7156247883972355 ) ) ;
#37046 = CARTESIAN_POINT ( 'NONE',  ( 7.228626920338837358, 113.7273137178985820, 10.49813415416005036 ) ) ;
#37047 = CARTESIAN_POINT ( 'NONE',  ( -34.17038769728823411, 208.1428034533959703, 6.469044688360770401 ) ) ;
#37049 = ADVANCED_FACE ( 'NONE', ( #1147, #18613 ), #9871, .F. ) ;
#37048 = CARTESIAN_POINT ( 'NONE',  ( -45.05580436395490551, 218.5000000000000000, 0.1155267958017064944 ) ) ;
#37050 = CARTESIAN_POINT ( 'NONE',  ( 15.24356964374999990, 3.323476615752268604, -4.790624999385491023 ) ) ;
#37051 = CARTESIAN_POINT ( 'NONE',  ( 27.24356964374999635, 195.1156250006145001, -15.72908226750539029 ) ) ;
#37052 = CARTESIAN_POINT ( 'NONE',  ( -13.23911966647199812, 99.35231371789856780, -8.632099005475788900 ) ) ;
#37053 = CARTESIAN_POINT ( 'NONE',  ( -36.34002896937850124, 204.4285982733020433, 3.350049139982171020 ) ) ;
#37054 = PRODUCT_DEFINITION ( 'UNKNOWN', '', #35947, #14535 ) ;
#37055 = VERTEX_POINT ( 'NONE', #35643 ) ;
#37056 = DIRECTION ( 'NONE',  ( 1.000000000000000000, 0.000000000000000000, 0.000000000000000000 ) ) ;
#37057 = CARTESIAN_POINT ( 'NONE',  ( 4.622313124798573369, 129.4351862821014549, 11.61527771782819940 ) ) ;
#37058 = CARTESIAN_POINT ( 'NONE',  ( 8.927990412390657937, 61.87268628210144783, -13.04141134922759804 ) ) ;
#37059 = FACE_OUTER_BOUND ( 'NONE', #25901, .T. ) ;
#37060 = CARTESIAN_POINT ( 'NONE',  ( 37.13513852234969193, 3.604726614523243278, 162.7885495010082764 ) ) ;
#37061 = CARTESIAN_POINT ( 'NONE',  ( -2.908627838312119351, 79.12268628210145494, -15.53471296425195369 ) ) ;
#37062 = CARTESIAN_POINT ( 'NONE',  ( 22.80587116629411071, -3.604726614523235284, -5.803124999385537386 ) ) ;
#37063 = CARTESIAN_POINT ( 'NONE',  ( 9.465287035748067623, 26.79768628210144144, 2.064181346179272847 ) ) ;
#37064 = LINE ( 'NONE', #28531, #6146 ) ;
#37065 = CARTESIAN_POINT ( 'NONE',  ( -59.70163769728823411, 215.6869285224996986, -3.149950860017881382 ) ) ;
#37066 = CARTESIAN_POINT ( 'NONE',  ( -70.80918835584510873, 215.2843023367891249, 7.500000000000000000 ) ) ;
#37067 = CARTESIAN_POINT ( 'NONE',  ( 4.622313124798573369, 55.83518628210144641, 11.61527771782819940 ) ) ;
#37068 = CARTESIAN_POINT ( 'NONE',  ( 27.00000000000000355, 197.5250000000000057, -3.306546357697854128E-15 ) ) ;
#37069 = CARTESIAN_POINT ( 'NONE',  ( 27.00000000000001421, 197.6000000012290627, 15.58845726811988897 ) ) ;
#37071 = CARTESIAN_POINT ( 'NONE',  ( 16.56230152254411436, 7.209453229046482114, -2.559374999385494842 ) ) ;
#37070 = CARTESIAN_POINT ( 'NONE',  ( -7.954856959092191815, 22.77268628210143220, -5.529263428287477744 ) ) ;
#37072 = LINE ( 'NONE', #25889, #22117 ) ;
#37073 = ORIENTED_EDGE ( 'NONE', *, *, #2314, .F. ) ;
#37074 = CARTESIAN_POINT ( 'NONE',  ( 26.99999999999999645, 3.464101615137755275, -5.137500000000001066 ) ) ;
#37076 = CARTESIAN_POINT ( 'NONE',  ( 10.56230152254410903, 0.000000000000000000, -3.937499998770993770 ) ) ;
#37075 = PRODUCT_DEFINITION_SHAPE ( 'NONE', 'NONE',  #37514 ) ;
#37077 = CARTESIAN_POINT ( 'NONE',  ( 24.47326942580252407, 3.604726614523240613, 161.3365789202697727 ) ) ;
#37078 = CARTESIAN_POINT ( 'NONE',  ( 13.44051670066911441, 5.407089921784856479, -2.465624999385545912 ) ) ;
#37079 = CARTESIAN_POINT ( 'NONE',  ( 36.63184559142159458, 7.347880794884125653E-16, 159.8305332246273167 ) ) ;
#37080 = CARTESIAN_POINT ( 'NONE',  ( 26.99999999999999645, 243.0625000000000284, -3.464101615137755275 ) ) ;
#37081 = DIRECTION ( 'NONE',  ( 0.000000000000000000, 0.000000000000000000, 1.000000000000000000 ) ) ;
#37082 = CARTESIAN_POINT ( 'NONE',  ( -8.715434833791929847, 69.06018628210145494, -8.962234695871762469 ) ) ;
#37083 = ORIENTED_EDGE ( 'NONE', *, *, #5826, .T. ) ;
#37084 = EDGE_LOOP ( 'NONE', ( #26931, #37449, #36381, #37299 ) ) ;
#37085 = CARTESIAN_POINT ( 'NONE',  ( 5.727106289114498080E-15, 196.6250000012290400, 31.17691453623979214 ) ) ;
#37086 = PLANE ( 'NONE',  #3805 ) ;
#37087 = CARTESIAN_POINT ( 'NONE',  ( 0.1745138560722461762, 31.78981371789855004, 15.50000000000000533 ) ) ;
#37088 = CARTESIAN_POINT ( 'NONE',  ( 26.75643035624999655, -3.323476615752267715, -8.165624999385475036 ) ) ;
#37089 = CARTESIAN_POINT ( 'NONE',  ( 15.24356964375000167, 243.1468750006145285, 3.323476615752272600 ) ) ;
#37090 = CARTESIAN_POINT ( 'NONE',  ( -49.01413769728823411, 212.1499508600178387, 3.954877714930865817 ) ) ;
#37091 = CARTESIAN_POINT ( 'NONE',  ( 15.00000000000000000, 0.000000000000000000, -7.200000000000011724 ) ) ;
#37092 = CARTESIAN_POINT ( 'NONE',  ( 24.63668644345436931, -3.604726614523244610, 163.2044439791918080 ) ) ;
#37093 = CARTESIAN_POINT ( 'NONE',  ( 9.534712964251900402, 48.17731371789854222, 1.715153634034445540 ) ) ;
#37094 = CARTESIAN_POINT ( 'NONE',  ( 13.44051670066911619, -5.407089921784859143, -9.515624999385547511 ) ) ;
#37095 = VECTOR ( 'NONE', #10430, 1000.000000000000000 ) ;
#37096 = CARTESIAN_POINT ( 'NONE',  ( 5.529263428287300108, 86.12731371789853085, 7.954856959092309943 ) ) ;
#37097 = CARTESIAN_POINT ( 'NONE',  ( -27.24356964374999990, 198.4718750006145171, -15.72908226750537786 ) ) ;
#37098 = CARTESIAN_POINT ( 'NONE',  ( -12.53471296425189152, 15.97731371789853760, -2.311890736173453753 ) ) ;
#37099 = CARTESIAN_POINT ( 'NONE',  ( 12.53471296425194836, 72.22268628210143504, -2.311890736173178418 ) ) ;
#37100 = CARTESIAN_POINT ( 'NONE',  ( 22.56230152254411436, -3.464101615137751278, -10.04999999877099270 ) ) ;
#37101 = EDGE_CURVE ( 'NONE', #16873, #24643, #13499, .T. ) ;
#37102 = CYLINDRICAL_SURFACE ( 'NONE', #13250, 5.999999999999998224 ) ;
#37103 = CARTESIAN_POINT ( 'NONE',  ( 25.18249928241153413, 0.000000000000000000, 169.4431132759913794 ) ) ;
#37104 = CARTESIAN_POINT ( 'NONE',  ( 22.80587116629411781, -3.604726614523238837, -9.909374999385510918 ) ) ;
#37105 =( BOUNDED_CURVE ( )  B_SPLINE_CURVE ( 2, ( #9476, #12508, #15352, #32402, #23694, #35804, #742 ),
 .UNSPECIFIED., .F., .F. ) 
 B_SPLINE_CURVE_WITH_KNOTS ( ( 3, 2, 2, 3 ),
 ( 0.6521739130434789367, 0.6594202898550732828, 0.6666666666666674068, 0.6739130434782617529 ),
 .UNSPECIFIED. ) 
 CURVE ( )  GEOMETRIC_REPRESENTATION_ITEM ( )  RATIONAL_B_SPLINE_CURVE ( ( 0.9999999999999876765, 0.8660254037844510311, 1.000000000000000000, 0.8660254037844387076, 1.000000000000000000, 0.8660254037844222763, 1.000000000000016431 ) ) 
 REPRESENTATION_ITEM ( '' )  );
#37106 = CARTESIAN_POINT ( 'NONE',  ( 22.80587116629412137, 7.646167579472024665E-16, -9.421874999385515537 ) ) ;
#37107 = LINE ( 'NONE', #31246, #37409 ) ;
#37108 = CARTESIAN_POINT ( 'NONE',  ( -8.710071997420127943, 77.68518628210145494, -3.796722387233380402 ) ) ;
#37109 = DIRECTION ( 'NONE',  ( -0.000000000000000000, -1.000000000000000000, -0.000000000000000000 ) ) ;
#37110 = CARTESIAN_POINT ( 'NONE',  ( 7.228626920339068285, 107.8726862821014549, -10.49813415415989581 ) ) ;
#37111 = CARTESIAN_POINT ( 'NONE',  ( 1.120210788295102201E-13, 195.0500000012290798, -27.00000000000000711 ) ) ;
#37112 = DIRECTION ( 'NONE',  ( 0.000000000000000000, 0.000000000000000000, 1.000000000000000000 ) ) ;
#37113 = VERTEX_POINT ( 'NONE', #32804 ) ;
#37114 = CARTESIAN_POINT ( 'NONE',  ( 30.86793661096032082, -7.209453229046475009, 162.7910315836186328 ) ) ;
#37115 = CARTESIAN_POINT ( 'NONE',  ( 18.12178482187500350, -4.985214923628407568, -6.815624999385455851 ) ) ;
#37116 = CARTESIAN_POINT ( 'NONE',  ( 27.00000000000001421, 196.1375000000000171, 15.58845726811988897 ) ) ;
#37117 = CARTESIAN_POINT ( 'NONE',  ( 25.06810737005524103, -3.604726614523244610, 168.1356077347459461 ) ) ;
#37118 = CARTESIAN_POINT ( 'NONE',  ( 31.11551339264931570, -6.928203230275514990, 165.6208471472733095 ) ) ;
#37119 = CARTESIAN_POINT ( 'NONE',  ( 26.99999999999999645, 7.347880794884117764E-16, -0.2250000000000029754 ) ) ;
#37120 = CARTESIAN_POINT ( 'NONE',  ( 21.00000000000000000, 240.5218750006145285, 6.646953231504538984 ) ) ;
#37121 = CARTESIAN_POINT ( 'NONE',  ( -13.62178482187498396, 198.9781250006145399, 23.59362340125808188 ) ) ;
#37122 = EDGE_CURVE ( 'NONE', #26922, #23387, #20259, .T. ) ;
#37123 = CARTESIAN_POINT ( 'NONE',  ( 10.49813415416005213, 120.6273137178985735, -7.228626920338837358 ) ) ;
#37124 = CARTESIAN_POINT ( 'NONE',  ( -12.46528703574805874, 132.5976862821014777, -2.660918448318280838 ) ) ;
#37125 = EDGE_CURVE ( 'NONE', #17695, #8916, #637, .T. ) ;
#37127 = ORIENTED_EDGE ( 'NONE', *, *, #33864, .F. ) ;
#37126 = VERTEX_POINT ( 'NONE', #29704 ) ;
#37128 = CARTESIAN_POINT ( 'NONE',  ( 26.75643035624999655, 241.8718750006145228, -7.049594010296217766E-16 ) ) ;
#37129 = CARTESIAN_POINT ( 'NONE',  ( 0.000000000000000000, 210.0000000000000284, -27.00000000000000000 ) ) ;
#37130 = CARTESIAN_POINT ( 'NONE',  ( 5.770363421894130873, 101.3648137178985706, -14.38691631536193860 ) ) ;
#37131 = CARTESIAN_POINT ( 'NONE',  ( 10.56230152254423693, 3.464101615137833434, -2.287500000000041389 ) ) ;
#37132 = CARTESIAN_POINT ( 'NONE',  ( 23.87821517812500005, -4.985214923628404016, -1.903124999385497063 ) ) ;
#37133 = B_SPLINE_CURVE_WITH_KNOTS ( 'NONE', 3,
 ( #223, #28290, #19965, #11788, #23356, #2329, #31508, #22987, #17866, #9704, #26374, #21281, #14830, #32440, #29978, #21091, #32631, #24302, #6668, #29411, #3442, #29598, #6484, #9519 ),
 .UNSPECIFIED., .F., .F.,
 ( 4, 2, 2, 2, 2, 2, 2, 2, 2, 2, 2, 4 ),
 ( 0.01257025459185682689, 0.01413966516175825527, 0.01570907573165968366, 0.01649378101661039958, 0.01727848630156111204, 0.01806319158651182449, 0.01884789687146253695, 0.02041730744136390635, 0.02198671801126527575, 0.02355612858116664515, 0.02434083386611728822, 0.02512553915106793476 ),
 .UNSPECIFIED. ) ;
#37134 = CARTESIAN_POINT ( 'NONE',  ( 19.68408634441911786, -5.407089921784861808, -8.596874999385523353 ) ) ;
#37135 = CARTESIAN_POINT ( 'NONE',  ( -26.99999999999998934, 198.8000000012290513, 15.58845726811991561 ) ) ;
#37136 = CARTESIAN_POINT ( 'NONE',  ( -7.228626920339069173, 121.6726862821014521, 10.49813415415989581 ) ) ;
#37137 = CARTESIAN_POINT ( 'NONE',  ( 22.80587116629411426, -3.604726614523235284, -3.103124999385562521 ) ) ;
#37138 = AXIS2_PLACEMENT_3D ( 'NONE', #25477, #25292, #19628 ) ;
#37139 = ADVANCED_FACE ( 'NONE', ( #3175 ), #5835, .T. ) ;
#37140 = CARTESIAN_POINT ( 'NONE',  ( -40.89211230271183695, 201.5309553116392181, 2.393094931466368980 ) ) ;
#37141 = CARTESIAN_POINT ( 'NONE',  ( 15.24356964374999990, 243.4093750006145171, -3.323476615752268604 ) ) ;
#37142 = DIRECTION ( 'NONE',  ( 1.000000000000000000, 0.000000000000000000, 0.000000000000000000 ) ) ;
#37143 = CARTESIAN_POINT ( 'NONE',  ( -36.14211230271182984, 205.5309553116392465, 1.321298161741817356 ) ) ;
#37144 = CARTESIAN_POINT ( 'NONE',  ( -12.46528703574805697, 123.3976862821014606, -2.660918448318280838 ) ) ;
#37145 = CARTESIAN_POINT ( 'NONE',  ( 16.56230152254411081, 6.928203230275506996, -4.049999998770996257 ) ) ;
#37146 = EDGE_CURVE ( 'NONE', #18605, #22116, #1454, .T. ) ;
#37147 = CARTESIAN_POINT ( 'NONE',  ( -43.67038769728823411, 208.1428034533959703, 6.469044688360770401 ) ) ;
#37148 = LINE ( 'NONE', #37327, #7647 ) ;
#37149 = PRESENTATION_STYLE_ASSIGNMENT (( #36777 ) ) ;
#37150 = CARTESIAN_POINT ( 'NONE',  ( 6.092822981423978490, 98.38518628210145778, -14.25334919248782306 ) ) ;
#37151 = CARTESIAN_POINT ( 'NONE',  ( 2.311890736173175753, 19.32268628210144357, 12.53471296425194659 ) ) ;
#37152 =( BOUNDED_CURVE ( )  B_SPLINE_CURVE ( 2, ( #22539, #15257, #34086, #2938, #10965, #9196, #26619, #26810, #649 ),
 .UNSPECIFIED., .F., .F. ) 
 B_SPLINE_CURVE_WITH_KNOTS ( ( 3, 2, 2, 2, 3 ),
 ( 0.2282608695652173780, 0.2318840579710144956, 0.2391304347826087029, 0.2463768115942029102, 0.2500000000000000000 ),
 .UNSPECIFIED. ) 
 CURVE ( )  GEOMETRIC_REPRESENTATION_ITEM ( )  RATIONAL_B_SPLINE_CURVE ( ( 0.9330127018922194093, 0.9330127018922190762, 1.000000000000000000, 0.8660254037844387076, 1.000000000000000000, 0.8660254037844387076, 1.000000000000000000, 0.9330127018922196314, 0.9330127018922194093 ) ) 
 REPRESENTATION_ITEM ( '' )  );
#37153 = CARTESIAN_POINT ( 'NONE',  ( 18.00000000000000355, 241.5812500012290513, 5.196152422706632912 ) ) ;
#37154 = CARTESIAN_POINT ( 'NONE',  ( -8.843639120294326972, 140.9351862821014549, 3.474262827703335166 ) ) ;
#37155 = CARTESIAN_POINT ( 'NONE',  ( 13.44051670066911264, 5.407089921784856479, -1.115624999385556038 ) ) ;
#37156 = CARTESIAN_POINT ( 'NONE',  ( 1.120210788295102201E-13, 195.3875000000000455, -27.00000000000000711 ) ) ;
#37157 = ORIENTED_EDGE ( 'NONE', *, *, #23535, .T. ) ;
#37158 = CARTESIAN_POINT ( 'NONE',  ( 20.99999999999999289, 244.9374999999999716, -5.999999999999997335 ) ) ;
#37159=STYLED_ITEM('',(#37556),#7513);
#37160 = CARTESIAN_POINT ( 'NONE',  ( 0.1745138560725194299, 70.21018628210144641, -9.500000000000005329 ) ) ;
#37161 = COLOUR_RGB ( '',0.8941176470588234615, 0.8941176470588234615, 0.8941176470588234615 ) ;
#37162 = FACE_OUTER_BOUND ( 'NONE', #1602, .T. ) ;
#37163 = VECTOR ( 'NONE', #33648, 1000.000000000000000 ) ;
#37164 = DIRECTION ( 'NONE',  ( 0.000000000000000000, 0.000000000000000000, 1.000000000000000000 ) ) ;
#37165 = CARTESIAN_POINT ( 'NONE',  ( -27.24356964374999990, 196.2218750006145456, -15.72908226750537786 ) ) ;
#37166 = CARTESIAN_POINT ( 'NONE',  ( 22.56230152254278920, -3.464101615138517332, -8.699999998771023257 ) ) ;
#37167 = DIRECTION ( 'NONE',  ( 0.08715574274765150453, 0.000000000000000000, 0.9961946980917461003 ) ) ;
#37168 = CARTESIAN_POINT ( 'NONE',  ( -6.594114490232462877, 32.93981371789854506, 6.840914352311949109 ) ) ;
#37169 = CARTESIAN_POINT ( 'NONE',  ( 26.99999999999999645, 7.347880794884117764E-16, -8.324999999999999289 ) ) ;
#37170 = ORIENTED_EDGE ( 'NONE', *, *, #9417, .F. ) ;
#37171 = CARTESIAN_POINT ( 'NONE',  ( 26.99999999999999645, 240.7937500012290570, 3.464101615137751278 ) ) ;
#37172 = CARTESIAN_POINT ( 'NONE',  ( 10.49813415416005213, 56.22731371789854649, -7.228626920338837358 ) ) ;
#37173 = CARTESIAN_POINT ( 'NONE',  ( 10.31873187879410381, -3.604726614523244610, -7.809374999385488181 ) ) ;
#37174 = CARTESIAN_POINT ( 'NONE',  ( 15.24356964374999990, 0.000000000000000000, -8.803124999385486760 ) ) ;
#37175 = CARTESIAN_POINT ( 'NONE',  ( 7.228626920338837358, 21.72731371789854649, 10.49813415416005036 ) ) ;
#37176 =( BOUNDED_CURVE ( )  B_SPLINE_CURVE ( 2, ( #25935, #14377, #26116, #15123, #9064, #5838, #9437, #14564, #34831 ),
 .UNSPECIFIED., .F., .F. ) 
 B_SPLINE_CURVE_WITH_KNOTS ( ( 3, 2, 2, 2, 3 ),
 ( 0.1875000000000000000, 0.1944444444444444475, 0.2083333333333333426, 0.2222222222222222099, 0.2291666666666666574 ),
 .UNSPECIFIED. ) 
 CURVE ( )  GEOMETRIC_REPRESENTATION_ITEM ( )  RATIONAL_B_SPLINE_CURVE ( ( 0.9330127018922194093, 0.9330127018922194093, 1.000000000000000000, 0.8660254037844387076, 1.000000000000000000, 0.8660254037844387076, 1.000000000000000000, 0.9330127018922194093, 0.9330127018922194093 ) ) 
 REPRESENTATION_ITEM ( '' )  );
#37177 = VERTEX_POINT ( 'NONE', #14749 ) ;
#37178 = CARTESIAN_POINT ( 'NONE',  ( 22.80587116629411781, 3.604726614523243278, -0.8343749993855380520 ) ) ;
#37179 = CARTESIAN_POINT ( 'NONE',  ( -7.228626920339069173, 11.27268628210143042, 10.49813415415989581 ) ) ;
#37180 = CARTESIAN_POINT ( 'NONE',  ( 24.91122703310946918, -3.604726614523244610, 166.3424572781808024 ) ) ;
#37181 = CARTESIAN_POINT ( 'NONE',  ( -38.91294563604516554, 214.6737587650350747, -4.842901733360249317 ) ) ;
#37182 = EDGE_CURVE ( 'NONE', #8395, #13579, #9434, .T. ) ;
#37183 = CARTESIAN_POINT ( 'NONE',  ( 10.56230152254410903, 0.000000000000000000, -2.700000000000063238 ) ) ;
#37184 = CARTESIAN_POINT ( 'NONE',  ( -35.95163769728824121, 213.9548777149308592, -2.149950860017830756 ) ) ;
#37185 = CARTESIAN_POINT ( 'NONE',  ( -45.64955436395490551, 214.8429017333601792, -4.673758765035196383 ) ) ;
#37186 = CARTESIAN_POINT ( 'NONE',  ( 31.33857762179763995, -7.209453229046475009, 168.1704829533140355 ) ) ;
#37187 = ORIENTED_EDGE ( 'NONE', *, *, #22705, .T. ) ;
#37188 = LINE ( 'NONE', #26186, #8271 ) ;
#37189 = CYLINDRICAL_SURFACE ( 'NONE', #33142, 5.999999999999994671 ) ;
#37190 = CARTESIAN_POINT ( 'NONE',  ( -15.46528703574811736, 15.40231371789854720, 3.257655550456946436 ) ) ;
#37191 = CARTESIAN_POINT ( 'NONE',  ( -69.99330436395489130, 210.1155267958016850, -8.500000000000003553 ) ) ;
#37192 = CARTESIAN_POINT ( 'NONE',  ( -11.61527771782819940, 12.13518628210144534, 4.622313124798574258 ) ) ;
#37193 = CARTESIAN_POINT ( 'NONE',  ( 11.48171059495397728, 45.48518628210145209, 4.944772684328674117 ) ) ;
#37194 = CARTESIAN_POINT ( 'NONE',  ( 10.56230152254410903, -3.464101615137761048, -4.912500000000052047 ) ) ;
#37195 = PLANE ( 'NONE',  #19210 ) ;
#37196 = EDGE_LOOP ( 'NONE', ( #18366, #34704, #19576, #33831, #21059, #882 ) ) ;
#37197 = CARTESIAN_POINT ( 'NONE',  ( 13.04141134922759804, 18.17268628210144499, 8.927990412390657937 ) ) ;
#37198 = CARTESIAN_POINT ( 'NONE',  ( 13.62178482187501416, 195.4531250006145342, 23.59362340125806767 ) ) ;
#37199 = CARTESIAN_POINT ( 'NONE',  ( -13.62178482187500528, 197.5343750006145456, -23.59362340125807123 ) ) ;
#37200 = CARTESIAN_POINT ( 'NONE',  ( 34.24790446256528753, 5.196152422706631135, 167.0031011721061134 ) ) ;
#37201 = CYLINDRICAL_SURFACE ( 'NONE', #16536, 27.00000000000000355 ) ;
#37202 = CARTESIAN_POINT ( 'NONE',  ( 20.99999999999999289, 240.0437500012290570, -5.999999999999997335 ) ) ;
#37203 = CARTESIAN_POINT ( 'NONE',  ( 15.24356964374999990, 245.3593750006145342, 0.000000000000000000 ) ) ;
#37204 = CARTESIAN_POINT ( 'NONE',  ( 8.710071997420211432, 111.7148137178985792, -3.796722387233181895 ) ) ;
#37205 = CARTESIAN_POINT ( 'NONE',  ( 18.12178482187499640, 241.2343750006145342, -4.985214923628404904 ) ) ;
#37206 = ORIENTED_EDGE ( 'NONE', *, *, #4005, .T. ) ;
#37207 = DIRECTION ( 'NONE',  ( 0.000000000000000000, 1.000000000000000000, 0.000000000000000000 ) ) ;
#37208 = CARTESIAN_POINT ( 'NONE',  ( -29.50000000000000711, 237.0000000000000000, 2.500000000000005329 ) ) ;
#37209 = CARTESIAN_POINT ( 'NONE',  ( 18.00000000000000000, 247.7312500012290570, -5.196152422706630247 ) ) ;
#37210 = ORIENTED_EDGE ( 'NONE', *, *, #26862, .F. ) ;
#37211 = ADVANCED_FACE ( 'NONE', ( #26113 ), #23464, .F. ) ;
#37212 = CARTESIAN_POINT ( 'NONE',  ( -12.53471296425189152, 117.1773137178985706, -2.311890736173453309 ) ) ;
#37213 = CARTESIAN_POINT ( 'NONE',  ( 10.31873187879411091, -3.604726614523240613, -9.103124999385528326 ) ) ;
#37214 = CARTESIAN_POINT ( 'NONE',  ( 24.51739202056851852, 3.604726614523236616, 161.8409024861786918 ) ) ;
#37215 = VECTOR ( 'NONE', #17884, 1000.000000000000000 ) ;
#37216 = DIRECTION ( 'NONE',  ( 0.000000000000000000, -1.000000000000000000, 0.000000000000000000 ) ) ;
#37217 = CARTESIAN_POINT ( 'NONE',  ( 27.00000000000001066, 195.6875000000000000, 15.58845726811988897 ) ) ;
#37218 = ORIENTED_EDGE ( 'NONE', *, *, #15285, .T. ) ;
#37219 = CIRCLE ( 'NONE', #3350, 10.00000000000000888 ) ;
#37220 = VERTEX_POINT ( 'NONE', #14561 ) ;
#37221 = ORIENTED_EDGE ( 'NONE', *, *, #6337, .F. ) ;
#37222 = CARTESIAN_POINT ( 'NONE',  ( 15.00000000000000000, 3.464101615137752166, -6.731249998770956644 ) ) ;
#37223 = CARTESIAN_POINT ( 'NONE',  ( 18.12178482187500350, -4.985214923628407568, -2.765624999385457805 ) ) ;
#37224 = DIRECTION ( 'NONE',  ( 1.000000000000000000, 0.000000000000000000, 0.000000000000000000 ) ) ;
#37225 = DIRECTION ( 'NONE',  ( 0.000000000000000000, 0.000000000000000000, 1.000000000000000000 ) ) ;
#37226 = CARTESIAN_POINT ( 'NONE',  ( 26.75643035624999655, 249.0718750006145115, -7.049594010296217766E-16 ) ) ;
#37227 = CARTESIAN_POINT ( 'NONE',  ( 10.69584247140445221, 62.44768628210145778, -6.932735513423970097 ) ) ;
#37228 = CARTESIAN_POINT ( 'NONE',  ( -65.63169563604516554, 210.1155267958017703, 6.500000000000000888 ) ) ;
#37229 = CARTESIAN_POINT ( 'NONE',  ( 5.025722718613374163, 215.9903539805198420, 0.3926987779610276452 ) ) ;
#37230 = CARTESIAN_POINT ( 'NONE',  ( -46.03794563604517975, 206.7903428501025758, 3.378800118222471838 ) ) ;
#37231 = CARTESIAN_POINT ( 'NONE',  ( 36.91292286188986793, -3.464101615137751278, 163.0432611271975532 ) ) ;
#37232 = CARTESIAN_POINT ( 'NONE',  ( -11.61527771782809282, 99.06481371789855928, -4.622313124798832717 ) ) ;
#37233 = CARTESIAN_POINT ( 'NONE',  ( -39.11830436395489841, 209.8844732041982581, 6.500000000000000888 ) ) ;
#37234 = CARTESIAN_POINT ( 'NONE',  ( -49.80580436395490551, 218.5000000000000000, 0.1155267958017064944 ) ) ;
#37235 = CARTESIAN_POINT ( 'NONE',  ( 26.75643035624999655, -3.323476615752267271, -4.115624999385481431 ) ) ;
#37236 = CARTESIAN_POINT ( 'NONE',  ( 10.56230152254458865, -3.464101615138036827, -5.362500000000041567 ) ) ;
#37237 = CARTESIAN_POINT ( 'NONE',  ( 2.908627838312458636, 82.67731371789852801, -15.53471296425188442 ) ) ;
#37238 = CARTESIAN_POINT ( 'NONE',  ( -37.52752896937850124, 213.3500491399821613, 5.571401726697954970 ) ) ;
#37239 = ORIENTED_EDGE ( 'NONE', *, *, #9691, .F. ) ;
#37240 = CARTESIAN_POINT ( 'NONE',  ( 26.97716818855048260, 0.000000000000000000, 49.47706554351410801 ) ) ;
#37241 = CARTESIAN_POINT ( 'NONE',  ( -2.311890736173176641, 97.52268628210144641, -12.53471296425194836 ) ) ;
#37242 = CARTESIAN_POINT ( 'NONE',  ( -8.927990412390661490, 66.47268628210146346, 13.04141134922759804 ) ) ;
#37243 = AXIS2_PLACEMENT_3D ( 'NONE', #31040, #24601, #1846 ) ;
#37244 = CARTESIAN_POINT ( 'NONE',  ( 19.56230152254412147, -5.196152422706635576, -0.7500000000000839329 ) ) ;
#37245 = CARTESIAN_POINT ( 'NONE',  ( 36.97172150469783958, -3.604726614523238837, 160.9206844420862694 ) ) ;
#37246 = CARTESIAN_POINT ( 'NONE',  ( -13.04141134922759804, 68.77268628210143220, -8.927990412390657937 ) ) ;
#37247 = EDGE_CURVE ( 'NONE', #31488, #37113, #3558, .T. ) ;
#37248 = CARTESIAN_POINT ( 'NONE',  ( 16.56230152254410726, -7.209453229046475009, -6.778124999385522820 ) ) ;
#37249 = CARTESIAN_POINT ( 'NONE',  ( -8.710071997420127943, 22.48518628210144499, -3.796722387233380402 ) ) ;
#37250 = CARTESIAN_POINT ( 'NONE',  ( 3.253724281355069334E-15, 199.8875000000000455, -27.00000000000000355 ) ) ;
#37251 = CARTESIAN_POINT ( 'NONE',  ( -60.09747103062156981, 213.3500491399821328, -5.571401726697985168 ) ) ;
#37252 =( LENGTH_UNIT ( ) NAMED_UNIT ( * ) SI_UNIT ( .MILLI., .METRE. ) );
#37253 = CARTESIAN_POINT ( 'NONE',  ( 4.622313124798573369, 37.43518628210144783, 11.61527771782819940 ) ) ;
#37254 = CARTESIAN_POINT ( 'NONE',  ( 27.00000000000001066, 198.8374999999999773, 15.58845726811988897 ) ) ;
#37255 = CARTESIAN_POINT ( 'NONE',  ( 7.234628195640337545, 197.7299038117967029, -26.99999999999999289 ) ) ;
#37256 = CARTESIAN_POINT ( 'NONE',  ( 7.954856959092191815, 27.37268628210144428, 5.529263428287477744 ) ) ;
#37257 = CARTESIAN_POINT ( 'NONE',  ( 18.12178482187499640, 249.3343750006145285, -4.985214923628404904 ) ) ;
#37258 = EDGE_LOOP ( 'NONE', ( #11161, #31353, #27858, #27371 ) ) ;
#37259 = CARTESIAN_POINT ( 'NONE',  ( 18.00000000000000355, -5.196152422706632912, -3.975000000000006306 ) ) ;
#37260 = CARTESIAN_POINT ( 'NONE',  ( -47.00000000000000711, 244.5000000000000000, -2.499999999999997780 ) ) ;
#37261 = EDGE_CURVE ( 'NONE', #21774, #1338, #28000, .T. ) ;
#37262 = CARTESIAN_POINT ( 'NONE',  ( 30.60810355289388696, 7.209453229046482114, 159.8211261399325736 ) ) ;
#37263 = CARTESIAN_POINT ( 'NONE',  ( 13.44051670066911264, 5.407089921784856479, -1.115624999385556038 ) ) ;
#37264 = CARTESIAN_POINT ( 'NONE',  ( 25.10896162446820412, 0.000000000000000000, 168.6025739994764479 ) ) ;
#37265 = CARTESIAN_POINT ( 'NONE',  ( 15.00000000000000000, 244.6000000000000227, 0.000000000000000000 ) ) ;
#37266 = CARTESIAN_POINT ( 'NONE',  ( 20.99999999999999289, 240.0437500012290570, -5.999999999999997335 ) ) ;
#37267 = EDGE_CURVE ( 'NONE', #27573, #1475, #34640, .T. ) ;
#37268 = CARTESIAN_POINT ( 'NONE',  ( 12.50000000000000355, 72.51018628210145778, 0.1745138560725507937 ) ) ;
#37269 = ORIENTED_EDGE ( 'NONE', *, *, #15863, .F. ) ;
#37270 = ORIENTED_EDGE ( 'NONE', *, *, #2926, .F. ) ;
#37271 = CARTESIAN_POINT ( 'NONE',  ( 5.727106289114498080E-15, 197.0750000012290570, 31.17691453623979214 ) ) ;
#37272 = FACE_OUTER_BOUND ( 'NONE', #28643, .T. ) ;
#37273 = CARTESIAN_POINT ( 'NONE',  ( -13.04141134922778456, 42.42731371789855643, 8.927990412390377273 ) ) ;
#37274 = CARTESIAN_POINT ( 'NONE',  ( 21.00000000000000000, -6.646953231504538984, -9.140624999385492444 ) ) ;
#37275 = VECTOR ( 'NONE', #14734, 1000.000000000000000 ) ;
#37276 = CARTESIAN_POINT ( 'NONE',  ( 15.24356964374999990, 241.7593750006145399, 0.000000000000000000 ) ) ;
#37277 = CARTESIAN_POINT ( 'NONE',  ( -44.46205436395490551, 213.2096571498974242, 3.378800118222489601 ) ) ;
#37278 = DIRECTION ( 'NONE',  ( -0.000000000000000000, -0.000000000000000000, 1.000000000000000000 ) ) ;
#37279 = CARTESIAN_POINT ( 'NONE',  ( 27.67142010346968561, -5.407089921784865361, 162.0731445772388213 ) ) ;
#37280 = CARTESIAN_POINT ( 'NONE',  ( -6.840914352311947333, 16.83981371789855430, -6.594114490232462877 ) ) ;
#37281 = CARTESIAN_POINT ( 'NONE',  ( 10.31873187879410736, -3.604726614523240613, -9.553124999385522287 ) ) ;
#37282 = CARTESIAN_POINT ( 'NONE',  ( 26.03202072822279334, 194.9999999999999716, -7.760941349413962520 ) ) ;
#37283 = CARTESIAN_POINT ( 'NONE',  ( -27.24356964374999990, 197.1218750006145228, -15.72908226750537786 ) ) ;
#37284 = CARTESIAN_POINT ( 'NONE',  ( 4.944772684328420986, 12.81481371789855395, 11.48171059495408208 ) ) ;
#37285 = CIRCLE ( 'NONE', #28812, 1.500000000000001332 ) ;
#37286 = ORIENTED_EDGE ( 'NONE', *, *, #35805, .F. ) ;
#37287 = CARTESIAN_POINT ( 'NONE',  ( 7.228626920339068285, 61.87268628210145494, -10.49813415415989581 ) ) ;
#37288 = CARTESIAN_POINT ( 'NONE',  ( 25.33117728503505361, 3.464101615137705981, 168.3478623745115783 ) ) ;
#37289 = DIRECTION ( 'NONE',  ( 1.000000000000000000, 0.000000000000000000, 0.000000000000000000 ) ) ;
#37290 = CARTESIAN_POINT ( 'NONE',  ( 30.63261610554165770, -7.209453229046475009, 160.1013058987709030 ) ) ;
#37291 = CARTESIAN_POINT ( 'NONE',  ( 15.00000000000000178, -3.464101615137757051, -3.506249998770959664 ) ) ;
#37292 = CARTESIAN_POINT ( 'NONE',  ( 22.80587116629411781, -3.604726614523238837, -9.909374999385510918 ) ) ;
#37293 = CARTESIAN_POINT ( 'NONE',  ( -4.500000000000002665, 244.5000000000000000, 2.500000000000000000 ) ) ;
#37294 = CARTESIAN_POINT ( 'NONE',  ( -5.529263428287477744, 84.87268628210145494, 7.954856959092191815 ) ) ;
#37295 = DIRECTION ( 'NONE',  ( 0.000000000000000000, 1.000000000000000000, 0.000000000000000000 ) ) ;
#37296 = CARTESIAN_POINT ( 'NONE',  ( 11.61527771782819940, 108.7351862821014663, -4.622313124798573369 ) ) ;
#37297 = CARTESIAN_POINT ( 'NONE',  ( -4.694659320240884604E-14, 197.4124999999999943, 27.00000000000000000 ) ) ;
#37298 = CARTESIAN_POINT ( 'NONE',  ( 22.56230152254484977, 3.464101615137326728, -3.674999998771035781 ) ) ;
#37299 = ORIENTED_EDGE ( 'NONE', *, *, #1973, .F. ) ;
#37300 = CARTESIAN_POINT ( 'NONE',  ( 27.78090950529641745, 5.407089921784856479, 163.3246141667165716 ) ) ;
#37301 = CARTESIAN_POINT ( 'NONE',  ( 15.24356964374999990, 0.000000000000000000, -7.340624999385481075 ) ) ;
#37302 = CARTESIAN_POINT ( 'NONE',  ( -13.62178482187500528, 195.7343750006145626, -23.59362340125807123 ) ) ;
#37303 = CARTESIAN_POINT ( 'NONE',  ( 37.56655944895057075, 3.604726614523243278, 167.7197132565624713 ) ) ;
#37304 = CARTESIAN_POINT ( 'NONE',  ( 25.12854018303972126, 0.000000000000000000, 166.0317097002238995 ) ) ;
#37305 = CARTESIAN_POINT ( 'NONE',  ( 15.00000000000000000, 0.000000000000000000, -5.849999999999994316 ) ) ;
#37306 = CARTESIAN_POINT ( 'NONE',  ( 15.24356964375000167, 241.3468750006145456, 3.323476615752272600 ) ) ;
#37307 = CARTESIAN_POINT ( 'NONE',  ( -13.62178482187500528, 197.4781250006145399, -23.59362340125807123 ) ) ;
#37308 = CARTESIAN_POINT ( 'NONE',  ( 12.50000000000000355, 130.6898137178985735, -0.1745138560722771515 ) ) ;
#37309 = CARTESIAN_POINT ( 'NONE',  ( -2.660918448318275509, 121.0976862821014635, 12.46528703574805874 ) ) ;
#37311 = VERTEX_POINT ( 'NONE', #12274 ) ;
#37310 = VERTEX_POINT ( 'NONE', #26482 ) ;
#37312 = CARTESIAN_POINT ( 'NONE',  ( 21.00000000000000000, 242.2093750006145285, 6.646953231504538984 ) ) ;
#37313 = VECTOR ( 'NONE', #13891, 1000.000000000000000 ) ;
#37314 = CARTESIAN_POINT ( 'NONE',  ( 10.56230152254397758, -3.464101615137684664, -2.212500000000047429 ) ) ;
#37315 = CARTESIAN_POINT ( 'NONE',  ( 13.04141134922778988, 102.2273137178985678, -8.927990412390371944 ) ) ;
#37316 = CARTESIAN_POINT ( 'NONE',  ( -12.53471296425194836, 95.22268628210146346, 2.311890736173176641 ) ) ;
#37317 = CARTESIAN_POINT ( 'NONE',  ( 23.87821517812499650, 4.985214923628404904, -1.303124999385479876 ) ) ;
#37318 = CARTESIAN_POINT ( 'NONE',  ( 27.00000000000001066, 196.2500000012290116, 15.58845726811988897 ) ) ;
#37319 = CARTESIAN_POINT ( 'NONE',  ( -10.69584247140444866, 113.0476862821014663, 6.932735513423972762 ) ) ;
#37320 = CARTESIAN_POINT ( 'NONE',  ( 22.80587116629410716, 3.604726614523238837, -2.578124999385541738 ) ) ;
#37321 = CARTESIAN_POINT ( 'NONE',  ( 20.99999999999999645, 245.1343750006145115, -6.646953231504538984 ) ) ;
#37322 = DIRECTION ( 'NONE',  ( 1.000000000000000000, 0.000000000000000000, 0.000000000000000000 ) ) ;
#37323 = CARTESIAN_POINT ( 'NONE',  ( -53.55877896937850124, 211.6261429550004607, -6.530955311639245586 ) ) ;
#37324 = CARTESIAN_POINT ( 'NONE',  ( -10.69584247140444866, 113.0476862821014663, 6.932735513423972762 ) ) ;
#37325 = CARTESIAN_POINT ( 'NONE',  ( 13.56230152254411792, -5.196152422706632912, -3.862499998771057541 ) ) ;
#37326 = CARTESIAN_POINT ( 'NONE',  ( -39.51413769728823411, 213.1499508600178672, 5.686928522499718142 ) ) ;
#37327 = CARTESIAN_POINT ( 'NONE',  ( 3.306546357697853733E-15, 210.0000000000000284, 27.00000000000000000 ) ) ;
#37328 = FACE_OUTER_BOUND ( 'NONE', #3664, .T. ) ;
#37329 = CARTESIAN_POINT ( 'NONE',  ( -5.770363421893818234, 106.4351862821014691, -14.38691631536207005 ) ) ;
#37330 = CARTESIAN_POINT ( 'NONE',  ( 11.48171059495397728, 17.88518628210143646, 4.944772684328674117 ) ) ;
#37331 = DIRECTION ( 'NONE',  ( 0.000000000000000000, 0.000000000000000000, -1.000000000000000000 ) ) ;
#37332 = CARTESIAN_POINT ( 'NONE',  ( 21.00000000000000000, 241.6187500012290457, 5.999999999999998224 ) ) ;
#37333 = CARTESIAN_POINT ( 'NONE',  ( 8.152565276336714462, 136.0476862821014379, -5.233372021372432847 ) ) ;
#37334 = CARTESIAN_POINT ( 'NONE',  ( 19.56230152254410370, 5.196152422706631135, -9.037499998771014731 ) ) ;
#37335 = VERTEX_POINT ( 'NONE', #35385 ) ;
#37336 = CARTESIAN_POINT ( 'NONE',  ( 31.39740774815230751, 7.209453229046475009, 168.8429143745259751 ) ) ;
#37337 = CARTESIAN_POINT ( 'NONE',  ( -6.840914352312096547, 66.76018628210144357, 6.594114490232313663 ) ) ;
#37338 = CARTESIAN_POINT ( 'NONE',  ( 15.24356964374999990, 0.000000000000000000, -0.1406249993854691294 ) ) ;
#37339 = CARTESIAN_POINT ( 'NONE',  ( 22.56230152254410370, 0.000000000000000000, -10.00000000000000000 ) ) ;
#37340 = CARTESIAN_POINT ( 'NONE',  ( -79.65000000000001990, 210.0000000000000000, 5.000000000000000000 ) ) ;
#37341 = CARTESIAN_POINT ( 'NONE',  ( 5.778771075727756162E-15, 196.3718750006145513, 31.45816453501075927 ) ) ;
#37342 = CARTESIAN_POINT ( 'NONE',  ( -7.102382295725191419, 195.0000000000001137, 26.31627238379491374 ) ) ;
#37343 = LINE ( 'NONE', #11393, #30286 ) ;
#37344 = CARTESIAN_POINT ( 'NONE',  ( 8.710071997420211432, 38.11481371789853512, -3.796722387233181895 ) ) ;
#37345 = CARTESIAN_POINT ( 'NONE',  ( 25.17102860762938832, -3.464101615137868073, 166.5173546155435815 ) ) ;
#37346 = EDGE_LOOP ( 'NONE', ( #18796, #16406, #26298, #30554 ) ) ;
#37347 = ORIENTED_EDGE ( 'NONE', *, *, #27231, .T. ) ;
#37348 = CARTESIAN_POINT ( 'NONE',  ( 15.00000000000000000, 239.6687500012290570, -3.464101615137752166 ) ) ;
#37349 = CARTESIAN_POINT ( 'NONE',  ( -12.46528703574811558, 43.00231371789854506, 2.660918448318004170 ) ) ;
#37350 = CARTESIAN_POINT ( 'NONE',  ( 22.80587116629411426, 7.646167579472024665E-16, -7.621874999385519267 ) ) ;
#37351 = CARTESIAN_POINT ( 'NONE',  ( 21.00000000000000000, 6.646953231504538984, -9.365624999385474325 ) ) ;
#37352 = CARTESIAN_POINT ( 'NONE',  ( 0.1745138560722461762, 142.1898137178985451, 15.50000000000000533 ) ) ;
#37353 = EDGE_LOOP ( 'NONE', ( #1274, #25206, #10492, #19607 ) ) ;
#37354 = CARTESIAN_POINT ( 'NONE',  ( 22.80587116629411426, 7.646167579472024665E-16, -1.771874999385525395 ) ) ;
#37355 = CIRCLE ( 'NONE', #34116, 8.000000000000000000 ) ;
#37356 = CARTESIAN_POINT ( 'NONE',  ( 0.000000000000000000, 210.0000000000000284, 0.000000000000000000 ) ) ;
#37357 = CARTESIAN_POINT ( 'NONE',  ( 34.38148213269554532, 5.407089921784862696, 167.1325768043071776 ) ) ;
#37358 = CARTESIAN_POINT ( 'NONE',  ( -42.27752896937850124, 213.3500491399821613, 5.571401726697954970 ) ) ;
#37359 = CARTESIAN_POINT ( 'NONE',  ( 3.061616997868383043E-15, 2.000000000000000000, 25.00000000000000000 ) ) ;
#37360 = CARTESIAN_POINT ( 'NONE',  ( 0.000000000000000000, 0.000000000000000000, -3.000000000000000000 ) ) ;
#37361 = CARTESIAN_POINT ( 'NONE',  ( -59.49627896937850835, 205.4690446883607535, -1.090244570138286351 ) ) ;
#37362 =( BOUNDED_CURVE ( )  B_SPLINE_CURVE ( 2, ( #8741, #34143, #19945, #28818, #8553, #23333, #20312 ),
 .UNSPECIFIED., .F., .F. ) 
 B_SPLINE_CURVE_WITH_KNOTS ( ( 3, 2, 2, 3 ),
 ( 0.5000000000000012212, 0.5072463768115955673, 0.5144927536231899134, 0.5217391304347842595 ),
 .UNSPECIFIED. ) 
 CURVE ( )  GEOMETRIC_REPRESENTATION_ITEM ( )  RATIONAL_B_SPLINE_CURVE ( ( 0.9999999999999774625, 0.8660254037844612451, 1.000000000000000000, 0.8660254037844387076, 1.000000000000000000, 0.8660254037844079544, 1.000000000000030864 ) ) 
 REPRESENTATION_ITEM ( '' )  );
#37364 = ADVANCED_FACE ( 'NONE', ( #6212, #8685 ), #14935, .F. ) ;
#37363 = CARTESIAN_POINT ( 'NONE',  ( -40.70163769728823411, 215.6869285224996986, -3.149950860017881382 ) ) ;
#37365 = CARTESIAN_POINT ( 'NONE',  ( 37.60414536301047406, -3.604726614523235284, 168.1493222201144704 ) ) ;
#37366 = VERTEX_POINT ( 'NONE', #12081 ) ;
#37367 = CARTESIAN_POINT ( 'NONE',  ( -13.50000000000000533, 196.7750000000000057, -23.38268590217984411 ) ) ;
#37368 = CARTESIAN_POINT ( 'NONE',  ( 20.99999999999997868, 210.0000000000000000, -5.999999999999999112 ) ) ;
#37369 = CARTESIAN_POINT ( 'NONE',  ( -5.770363421894122880, 23.16481371789855359, 14.38691631536194393 ) ) ;
#37370 = CARTESIAN_POINT ( 'NONE',  ( -36.14211230271182984, 201.5309553116392181, 2.393094931466368980 ) ) ;
#37371 = PRODUCT ( 'pusher', 'pusher', '', ( #30261 ) ) ;
#37372 = CARTESIAN_POINT ( 'NONE',  ( -7.228626920339069173, 11.27268628210143042, 10.49813415415989581 ) ) ;
#37373 = CARTESIAN_POINT ( 'NONE',  ( 8.715434833791931624, 55.26018628210144357, 8.962234695871760692 ) ) ;
#37375 = EDGE_CURVE ( 'NONE', #12783, #34986, #36572, .T. ) ;
#37374 = CARTESIAN_POINT ( 'NONE',  ( 22.56230152254412147, 3.464101615137759271, -4.237500000000042455 ) ) ;
#37376 = ORIENTED_EDGE ( 'NONE', *, *, #29096, .T. ) ;
#37377 = CARTESIAN_POINT ( 'NONE',  ( 27.24356964375000700, 195.9968750006145513, 15.72908226750537075 ) ) ;
#37378 = CARTESIAN_POINT ( 'NONE',  ( 10.56230152254411259, -3.464101615137757051, -6.599999998771014731 ) ) ;
#37379 = DIRECTION ( 'NONE',  ( 0.9961946980917462113, 0.000000000000000000, -0.08715574274765178209 ) ) ;
#37380 = CARTESIAN_POINT ( 'NONE',  ( 31.22336862440664618, 6.928203230275506996, 166.8536380873862015 ) ) ;
#37381 = CYLINDRICAL_SURFACE ( 'NONE', #8476, 6.000000000000001776 ) ;
#37382 =( BOUNDED_CURVE ( )  B_SPLINE_CURVE ( 2, ( #3905, #30061, #4466, #27032, #26840, #36296, #35555 ),
 .UNSPECIFIED., .F., .F. ) 
 B_SPLINE_CURVE_WITH_KNOTS ( ( 3, 2, 2, 3 ),
 ( 0.6521739130434772713, 0.6594202898550713954, 0.6666666666666655194, 0.6739130434782596435 ),
 .UNSPECIFIED. ) 
 CURVE ( )  GEOMETRIC_REPRESENTATION_ITEM ( )  RATIONAL_B_SPLINE_CURVE ( ( 1.000000000000018430, 0.8660254037844202779, 1.000000000000000000, 0.8660254037844387076, 1.000000000000000000, 0.8660254037844612451, 0.9999999999999774625 ) ) 
 REPRESENTATION_ITEM ( '' )  );
#37383 = CARTESIAN_POINT ( 'NONE',  ( 18.12178482187499640, 245.2843750006145456, -4.985214923628404904 ) ) ;
#37384 = CARTESIAN_POINT ( 'NONE',  ( 8.710071997420211432, 93.31481371789855928, -3.796722387233181895 ) ) ;
#37385 = CARTESIAN_POINT ( 'NONE',  ( 18.12178482187499640, 240.7843750006145171, -4.985214923628404904 ) ) ;
#37386 = VECTOR ( 'NONE', #947, 1000.000000000000000 ) ;
#37387 = ORIENTED_EDGE ( 'NONE', *, *, #30559, .T. ) ;
#37388 = CARTESIAN_POINT ( 'NONE',  ( -52.57663769728823411, 204.3130714775002730, 3.149950860017883603 ) ) ;
#37389 = CARTESIAN_POINT ( 'NONE',  ( -13.49999999999998401, 196.0250000000000057, 23.38268590217985476 ) ) ;
#37390 = ADVANCED_FACE ( 'NONE', ( #6018 ), #15311, .T. ) ;
#37391 = CARTESIAN_POINT ( 'NONE',  ( 26.99999999999999645, 245.2937500012290570, 3.464101615137751278 ) ) ;
#37392 = VERTEX_POINT ( 'NONE', #17602 ) ;
#37393 = CARTESIAN_POINT ( 'NONE',  ( -6.932735513424201912, 115.4523137178985621, 10.69584247140429412 ) ) ;
#37394 = CARTESIAN_POINT ( 'NONE',  ( 13.44051670066911086, 5.407089921784862696, -1.171874999385535965 ) ) ;
#37395 = CARTESIAN_POINT ( 'NONE',  ( 24.48144027668511669, 0.000000000000000000, 161.4299721732159014 ) ) ;
#37396 = CARTESIAN_POINT ( 'NONE',  ( 18.12178482187499640, 4.985214923628404904, -1.228124999385488136 ) ) ;
#37397 = CARTESIAN_POINT ( 'NONE',  ( 10.69584247140429589, 57.95231371789854791, 6.932735513424201024 ) ) ;
#37398 = CARTESIAN_POINT ( 'NONE',  ( 27.00000000000000355, 195.7250000000000227, -3.306546357697854128E-15 ) ) ;
#37399 = EDGE_LOOP ( 'NONE', ( #17569, #3361 ) ) ;
#37400 = ORIENTED_EDGE ( 'NONE', *, *, #8012, .T. ) ;
#37401 = ORIENTED_EDGE ( 'NONE', *, *, #18000, .F. ) ;
#37402 = CARTESIAN_POINT ( 'NONE',  ( 18.00000000000000000, 5.196152422706630247, -7.218749998770951137 ) ) ;
#37403 = CARTESIAN_POINT ( 'NONE',  ( 26.75643035624999655, 3.323476615752271268, -1.678124999385453897 ) ) ;
#37404 = CARTESIAN_POINT ( 'NONE',  ( 18.00000000000000000, 241.8812500012290343, -5.196152422706630247 ) ) ;
#37405 = CARTESIAN_POINT ( 'NONE',  ( 26.75643035624999655, 245.9218750006145342, -7.049594010296217766E-16 ) ) ;
#37406 = CARTESIAN_POINT ( 'NONE',  ( 4.944772684328679446, 61.58518628210145351, -11.48171059495397373 ) ) ;
#37407 = CARTESIAN_POINT ( 'NONE',  ( -52.96502896937850124, 215.5714017266979567, -3.350049139982168800 ) ) ;
#37408 = CARTESIAN_POINT ( 'NONE',  ( -47.00000000000000711, 244.5000000000000000, 2.500000000000000000 ) ) ;
#37409 = VECTOR ( 'NONE', #17224, 1000.000000000000000 ) ;
#37410 = CARTESIAN_POINT ( 'NONE',  ( -36.93377896937849414, 208.9097554298617183, 4.530955311639234040 ) ) ;
#37411 = FILL_AREA_STYLE_COLOUR ( '', #8069 ) ;
#37412 = CARTESIAN_POINT ( 'NONE',  ( 24.78536444607796341, 0.000000000000000000, 162.1091930777120069 ) ) ;
#37413 = CARTESIAN_POINT ( 'NONE',  ( -4.622313124798826500, 96.76481371789854791, 11.61527771782809637 ) ) ;
#37414 = CARTESIAN_POINT ( 'NONE',  ( -35.55580436395490551, 216.5000000000000000, 0.1155267958017343610 ) ) ;
#37415 = CARTESIAN_POINT ( 'NONE',  ( -42.68080436395489841, 201.5000000000000000, -0.1155267958017054536 ) ) ;
#37416 = CARTESIAN_POINT ( 'NONE',  ( 26.75643035624999655, -3.323476615752267271, -5.015624999385472904 ) ) ;
#37417 = CARTESIAN_POINT ( 'NONE',  ( 22.56230152254410370, 0.000000000000000000, -10.00000000000000000 ) ) ;
#37418 = CARTESIAN_POINT ( 'NONE',  ( 11.08355503943118769, 67.43981371789855928, 10.83675517735179028 ) ) ;
#37419 = CARTESIAN_POINT ( 'NONE',  ( -30.00669563604516910, 209.8844732041982013, -6.500000000000000888 ) ) ;
#37420 = ADVANCED_FACE ( 'NONE', ( #25306 ), #36678, .F. ) ;
#37421 = ORIENTED_EDGE ( 'NONE', *, *, #2863, .F. ) ;
#37422 = DIRECTION ( 'NONE',  ( 0.000000000000000000, 0.000000000000000000, 1.000000000000000000 ) ) ;
#37423 = CARTESIAN_POINT ( 'NONE',  ( -7.228626920339069173, 103.2726862821014606, 10.49813415415989581 ) ) ;
#37424 = CARTESIAN_POINT ( 'NONE',  ( -8.927990412390661490, 48.07268628210143646, 13.04141134922759804 ) ) ;
#37425 = DIRECTION ( 'NONE',  ( 0.000000000000000000, -1.000000000000000000, 0.000000000000000000 ) ) ;
#37426 = CARTESIAN_POINT ( 'NONE',  ( 27.63220001923324176, -5.407089921784865361, 161.6248569630975283 ) ) ;
#37427 = CARTESIAN_POINT ( 'NONE',  ( 14.38691631536207538, 62.73518628210145920, -5.770363421893813793 ) ) ;
#37428 = ADVANCED_FACE ( 'NONE', ( #13196 ), #16787, .F. ) ;
#37429 = CARTESIAN_POINT ( 'NONE',  ( 13.44051670066911441, -5.407089921784859143, -8.165624999385528326 ) ) ;
#37430 = CARTESIAN_POINT ( 'NONE',  ( 22.56230152254410370, 7.347880794884117764E-16, -1.462499998771016330 ) ) ;
#37431 = CARTESIAN_POINT ( 'NONE',  ( -49.01413769728823411, 213.1499508600178672, 5.686928522499718142 ) ) ;
#37432 = CARTESIAN_POINT ( 'NONE',  ( 10.56230152254410726, 0.000000000000000000, -3.600000000000047606 ) ) ;
#37433 = CARTESIAN_POINT ( 'NONE',  ( -8.962234695871760692, 48.36018628210145209, 8.715434833791933400 ) ) ;
#37434 = CARTESIAN_POINT ( 'NONE',  ( -27.00000000000000355, 196.8125000000000000, -15.58845726811989429 ) ) ;
#37435 = VECTOR ( 'NONE', #26474, 1000.000000000000000 ) ;
#37436 = CARTESIAN_POINT ( 'NONE',  ( 31.06648828746087787, 6.928203230275506996, 165.0604876308210578 ) ) ;
#37437 = CARTESIAN_POINT ( 'NONE',  ( -7.954856959092191815, 13.57268628210145422, -5.529263428287477744 ) ) ;
#37438 = CARTESIAN_POINT ( 'NONE',  ( 18.12178482187499640, 248.8843750006145399, -4.985214923628404904 ) ) ;
#37439 = ORIENTED_EDGE ( 'NONE', *, *, #5707, .F. ) ;
#37440 = CARTESIAN_POINT ( 'NONE',  ( 15.00000000000000000, 3.464101615137752166, -4.987500000000014921 ) ) ;
#37441 = CARTESIAN_POINT ( 'NONE',  ( -56.70466238434234185, 244.2363183625454894, 2.500000000000000000 ) ) ;
#37442 = CARTESIAN_POINT ( 'NONE',  ( 36.97498984505087805, 7.646167579472024665E-16, 160.9580417432647153 ) ) ;
#37443 = CARTESIAN_POINT ( 'NONE',  ( 10.31873187879411269, -3.604726614523240613, -5.503124999385529570 ) ) ;
#37444 = CARTESIAN_POINT ( 'NONE',  ( 29.54925771143595981, 5.908847357411728396, 159.6727445521698883 ) ) ;
#37445 = CARTESIAN_POINT ( 'NONE',  ( 15.00000000000000178, 240.5875000000000057, 3.464101615137757051 ) ) ;
#37446 = CARTESIAN_POINT ( 'NONE',  ( 1.069080835302379631E-14, 198.7624999999999886, 27.00000000000000000 ) ) ;
#37447 = CARTESIAN_POINT ( 'NONE',  ( 12.53471296425194659, 72.22268628210144925, -2.311890736173178418 ) ) ;
#37448 = EDGE_LOOP ( 'NONE', ( #14111, #28189, #33396, #10515 ) ) ;
#37449 = ORIENTED_EDGE ( 'NONE', *, *, #30955, .T. ) ;
#37450 = CARTESIAN_POINT ( 'NONE',  ( 27.96678062107526941, -5.196152422706638241, 164.0518066177726553 ) ) ;
#37451 = CARTESIAN_POINT ( 'NONE',  ( -27.00000000000000355, 195.5750000012290286, -15.58845726811989429 ) ) ;
#37452 = CARTESIAN_POINT ( 'NONE',  ( -26.99999999999999645, 196.5500000012290513, 15.58845726811991561 ) ) ;
#37453 = CARTESIAN_POINT ( 'NONE',  ( -8.632099005475794229, 32.65231371789855075, 13.23911966647199812 ) ) ;
#37454 = DIRECTION ( 'NONE',  ( 0.08715574274765143514, 0.000000000000000000, 0.9961946980917462113 ) ) ;
#37455 = CARTESIAN_POINT ( 'NONE',  ( 20.99999999999997868, 246.0625000000000284, 5.999999999999999112 ) ) ;
#37456 = CARTESIAN_POINT ( 'NONE',  ( -45.25372103062157692, 214.5309553116392749, -1.090244570138262148 ) ) ;
#37457 = CARTESIAN_POINT ( 'NONE',  ( 15.00000000000000178, 242.8937500012290229, 3.464101615137757051 ) ) ;
#37458 = CARTESIAN_POINT ( 'NONE',  ( 33.81932759197320593, -5.407089921784861808, 160.7071210016154055 ) ) ;
#37459 = CARTESIAN_POINT ( 'NONE',  ( -7.954856959092309943, 14.82731371789855324, 5.529263428287300108 ) ) ;
#37460 = CARTESIAN_POINT ( 'NONE',  ( -4.694659320240884604E-14, 197.0750000012290570, 27.00000000000000000 ) ) ;
#37461 = CARTESIAN_POINT ( 'NONE',  ( 0.000000000000000000, 0.000000000000000000, 0.000000000000000000 ) ) ;
#37462 = CARTESIAN_POINT ( 'NONE',  ( 13.47611835081543141, 194.9999999999999716, 23.69796585698624014 ) ) ;
#37463 = CARTESIAN_POINT ( 'NONE',  ( -27.24356964374999990, 195.7718750006145569, -15.72908226750537786 ) ) ;
#37464 = CARTESIAN_POINT ( 'NONE',  ( 11.08355503943118769, 131.8398137178985792, 10.83675517735179028 ) ) ;
#37465 = EDGE_CURVE ( 'NONE', #11399, #36527, #27965, .T. ) ;
#37466 = ORIENTED_EDGE ( 'NONE', *, *, #6157, .T. ) ;
#37467 = CARTESIAN_POINT ( 'NONE',  ( 6.932735513423970097, 37.14768628210143930, 10.69584247140445044 ) ) ;
#37468 = DIRECTION ( 'NONE',  ( 0.000000000000000000, 0.000000000000000000, -1.000000000000000000 ) ) ;
#37469 = CARTESIAN_POINT ( 'NONE',  ( 28.28586808984062628, 5.407089921784862696, 169.0963171987856128 ) ) ;
#37470 = EDGE_CURVE ( 'NONE', #21628, #26422, #31187, .T. ) ;
#37471 = CARTESIAN_POINT ( 'NONE',  ( 21.00000000000000000, -6.928203230275506996, -2.981249998770937992 ) ) ;
#37472 = CARTESIAN_POINT ( 'NONE',  ( 10.31873187879410558, 0.000000000000000000, -9.196874999385512339 ) ) ;
#37473 = CARTESIAN_POINT ( 'NONE',  ( 1.120210788295102201E-13, 196.8500000012290343, -27.00000000000000711 ) ) ;
#37474 = CARTESIAN_POINT ( 'NONE',  ( 5.529263428287477744, 71.07268628210144357, -7.954856959092191815 ) ) ;
#37475 = CARTESIAN_POINT ( 'NONE',  ( 6.123233995736767268E-16, 148.0000000000000000, 5.000000000000000888 ) ) ;
#37476 = CARTESIAN_POINT ( 'NONE',  ( -0.1745138560725500443, 93.21018628210146062, 12.50000000000000355 ) ) ;
#37477 = DIRECTION ( 'NONE',  ( -1.000000000000000000, -4.130293990420971855E-17, 0.000000000000000000 ) ) ;
#37478 = CARTESIAN_POINT ( 'NONE',  ( 0.000000000000000000, 150.0000000000000000, 0.000000000000000000 ) ) ;
#37479 = ORIENTED_EDGE ( 'NONE', *, *, #9772, .F. ) ;
#37480 = CARTESIAN_POINT ( 'NONE',  ( 27.63710252976279591, -5.407089921784859143, 161.6808929148651828 ) ) ;
#37481 = CARTESIAN_POINT ( 'NONE',  ( 21.00000000000000000, -6.646953231504538984, -6.778124999385457983 ) ) ;
#37482 = CARTESIAN_POINT ( 'NONE',  ( -27.24356964374999279, 196.2968750006145342, 15.72908226750539384 ) ) ;
#37483 = CARTESIAN_POINT ( 'NONE',  ( 31.23562490067698150, 7.209453229046482114, 166.9937279661931768 ) ) ;
#37484 = CARTESIAN_POINT ( 'NONE',  ( 34.08121910445329661, 5.196152422706637353, 165.0978788107812818 ) ) ;
#37485 = CARTESIAN_POINT ( 'NONE',  ( 15.00000000000000000, 0.000000000000000000, 0.000000000000000000 ) ) ;
#37486 = CARTESIAN_POINT ( 'NONE',  ( 15.24356964375000167, 240.4468750006145399, 3.323476615752272600 ) ) ;
#37487 = CARTESIAN_POINT ( 'NONE',  ( 13.62178482187501416, 199.0531250006145285, 23.59362340125806767 ) ) ;
#37488 = CARTESIAN_POINT ( 'NONE',  ( 6.932735513424201024, 129.2523137178985451, -10.69584247140429412 ) ) ;
#37489 = CARTESIAN_POINT ( 'NONE',  ( -12.50000000000000355, 123.1101862821014663, -0.1745138560725492671 ) ) ;
#37491 = VERTEX_POINT ( 'NONE', #28332 ) ;
#37490 = VERTEX_POINT ( 'NONE', #7694 ) ;
#37492 = CARTESIAN_POINT ( 'NONE',  ( 27.24356964375000345, 197.3281250006145342, -3.336375036156643733E-15 ) ) ;
#37493 = CARTESIAN_POINT ( 'NONE',  ( 26.75643035624999655, 242.3593750006145342, -3.323476615752271712 ) ) ;
#37494 = CARTESIAN_POINT ( 'NONE',  ( 21.00000000000000000, 243.8125000000000284, 5.999999999999998224 ) ) ;
#37495 = CARTESIAN_POINT ( 'NONE',  ( -13.23911966647199812, 99.35231371789856780, -8.632099005475788900 ) ) ;
#37496 = CARTESIAN_POINT ( 'NONE',  ( 26.75643035624999655, 3.323476615752271712, -2.690624999385500260 ) ) ;
#37497 = CARTESIAN_POINT ( 'NONE',  ( -27.00000000000000355, 196.0250000012290457, -15.58845726811989429 ) ) ;
#37498 = CARTESIAN_POINT ( 'NONE',  ( -2.064181346179062349, 72.90231371789855075, -9.465287035748106703 ) ) ;
#37499 = CARTESIAN_POINT ( 'NONE',  ( 10.31873187879410736, 3.604726614523236616, -1.978124999385525662 ) ) ;
#37500 = CARTESIAN_POINT ( 'NONE',  ( 3.796722387233379514, 135.1851862821014549, -8.710071997420127943 ) ) ;
#37501 = NEXT_ASSEMBLY_USAGE_OCCURRENCE ( 'NAUO1', ' ', ' ', #13673, #15289, $ ) ;
#37502 = NEXT_ASSEMBLY_USAGE_OCCURRENCE ( 'NAUO2', ' ', ' ', #13673, #28710, $ ) ;
#37503 = NEXT_ASSEMBLY_USAGE_OCCURRENCE ( 'NAUO3', ' ', ' ', #13673, #37054, $ ) ;
#37504 = NEXT_ASSEMBLY_USAGE_OCCURRENCE ( 'NAUO4', ' ', ' ', #13673, #33139, $ ) ;
#37505 = NEXT_ASSEMBLY_USAGE_OCCURRENCE ( 'NAUO5', ' ', ' ', #13673, #10201, $ ) ;
#37506 = NEXT_ASSEMBLY_USAGE_OCCURRENCE ( 'NAUO6', ' ', ' ', #13673, #29920, $ ) ;
#37507 = NEXT_ASSEMBLY_USAGE_OCCURRENCE ( 'NAUO7', ' ', ' ', #13673, #18078, $ ) ;
#37508 = NEXT_ASSEMBLY_USAGE_OCCURRENCE ( 'NAUO8', ' ', ' ', #13673, #31497, $ ) ;
#37509 = NEXT_ASSEMBLY_USAGE_OCCURRENCE ( 'NAUO9', ' ', ' ', #13673, #18775, $ ) ;
#37510 = NEXT_ASSEMBLY_USAGE_OCCURRENCE ( 'NAUO10', ' ', ' ', #13673, #32183, $ ) ;
#37511 = NEXT_ASSEMBLY_USAGE_OCCURRENCE ( 'NAUO11', ' ', ' ', #13673, #32183, $ ) ;
#37512 = NEXT_ASSEMBLY_USAGE_OCCURRENCE ( 'NAUO12', ' ', ' ', #13673, #32183, $ ) ;
#37513 = NEXT_ASSEMBLY_USAGE_OCCURRENCE ( 'NAUO13', ' ', ' ', #13673, #7423, $ ) ;
#37514 = NEXT_ASSEMBLY_USAGE_OCCURRENCE ( 'NAUO14', ' ', ' ', #13673, #6956, $ ) ;
#37515=COLOUR_RGB('Dark Blue',0.08,0.2,0.34);
#37516=FILL_AREA_STYLE_COLOUR('',#37515);
#37517=FILL_AREA_STYLE('',(#37516));
#37518=SURFACE_STYLE_FILL_AREA(#37517);
#37519=SURFACE_SIDE_STYLE('',(#37518));
#37520=SURFACE_STYLE_USAGE(.BOTH.,#37519);
#37521=PRESENTATION_STYLE_ASSIGNMENT((#37520));
#37522=COLOUR_RGB('Light Blue',0.38,0.62,0.78);
#37523=FILL_AREA_STYLE_COLOUR('',#37522);
#37524=FILL_AREA_STYLE('',(#37523));
#37525=SURFACE_STYLE_FILL_AREA(#37524);
#37526=SURFACE_SIDE_STYLE('',(#37525));
#37527=SURFACE_STYLE_USAGE(.BOTH.,#37526);
#37528=PRESENTATION_STYLE_ASSIGNMENT((#37527));
#37529=COLOUR_RGB('Sky Blue',0.24,0.69,0.87);
#37530=FILL_AREA_STYLE_COLOUR('',#37529);
#37531=FILL_AREA_STYLE('',(#37530));
#37532=SURFACE_STYLE_FILL_AREA(#37531);
#37533=SURFACE_SIDE_STYLE('',(#37532));
#37534=SURFACE_STYLE_USAGE(.BOTH.,#37533);
#37535=PRESENTATION_STYLE_ASSIGNMENT((#37534));
#37536=COLOUR_RGB('Grey',0.48,0.52,0.57);
#37537=FILL_AREA_STYLE_COLOUR('',#37536);
#37538=FILL_AREA_STYLE('',(#37537));
#37539=SURFACE_STYLE_FILL_AREA(#37538);
#37540=SURFACE_SIDE_STYLE('',(#37539));
#37541=SURFACE_STYLE_USAGE(.BOTH.,#37540);
#37542=PRESENTATION_STYLE_ASSIGNMENT((#37541));
#37543=COLOUR_RGB('Black',0.12,0.14,0.17);
#37544=FILL_AREA_STYLE_COLOUR('',#37543);
#37545=FILL_AREA_STYLE('',(#37544));
#37546=SURFACE_STYLE_FILL_AREA(#37545);
#37547=SURFACE_SIDE_STYLE('',(#37546));
#37548=SURFACE_STYLE_USAGE(.BOTH.,#37547);
#37549=PRESENTATION_STYLE_ASSIGNMENT((#37548));
#37550=COLOUR_RGB('Off White',0.89,0.88,0.83);
#37551=FILL_AREA_STYLE_COLOUR('',#37550);
#37552=FILL_AREA_STYLE('',(#37551));
#37553=SURFACE_STYLE_FILL_AREA(#37552);
#37554=SURFACE_SIDE_STYLE('',(#37553));
#37555=SURFACE_STYLE_USAGE(.BOTH.,#37554);
#37556=PRESENTATION_STYLE_ASSIGNMENT((#37555));
ENDSEC;
END-ISO-10303-21;
